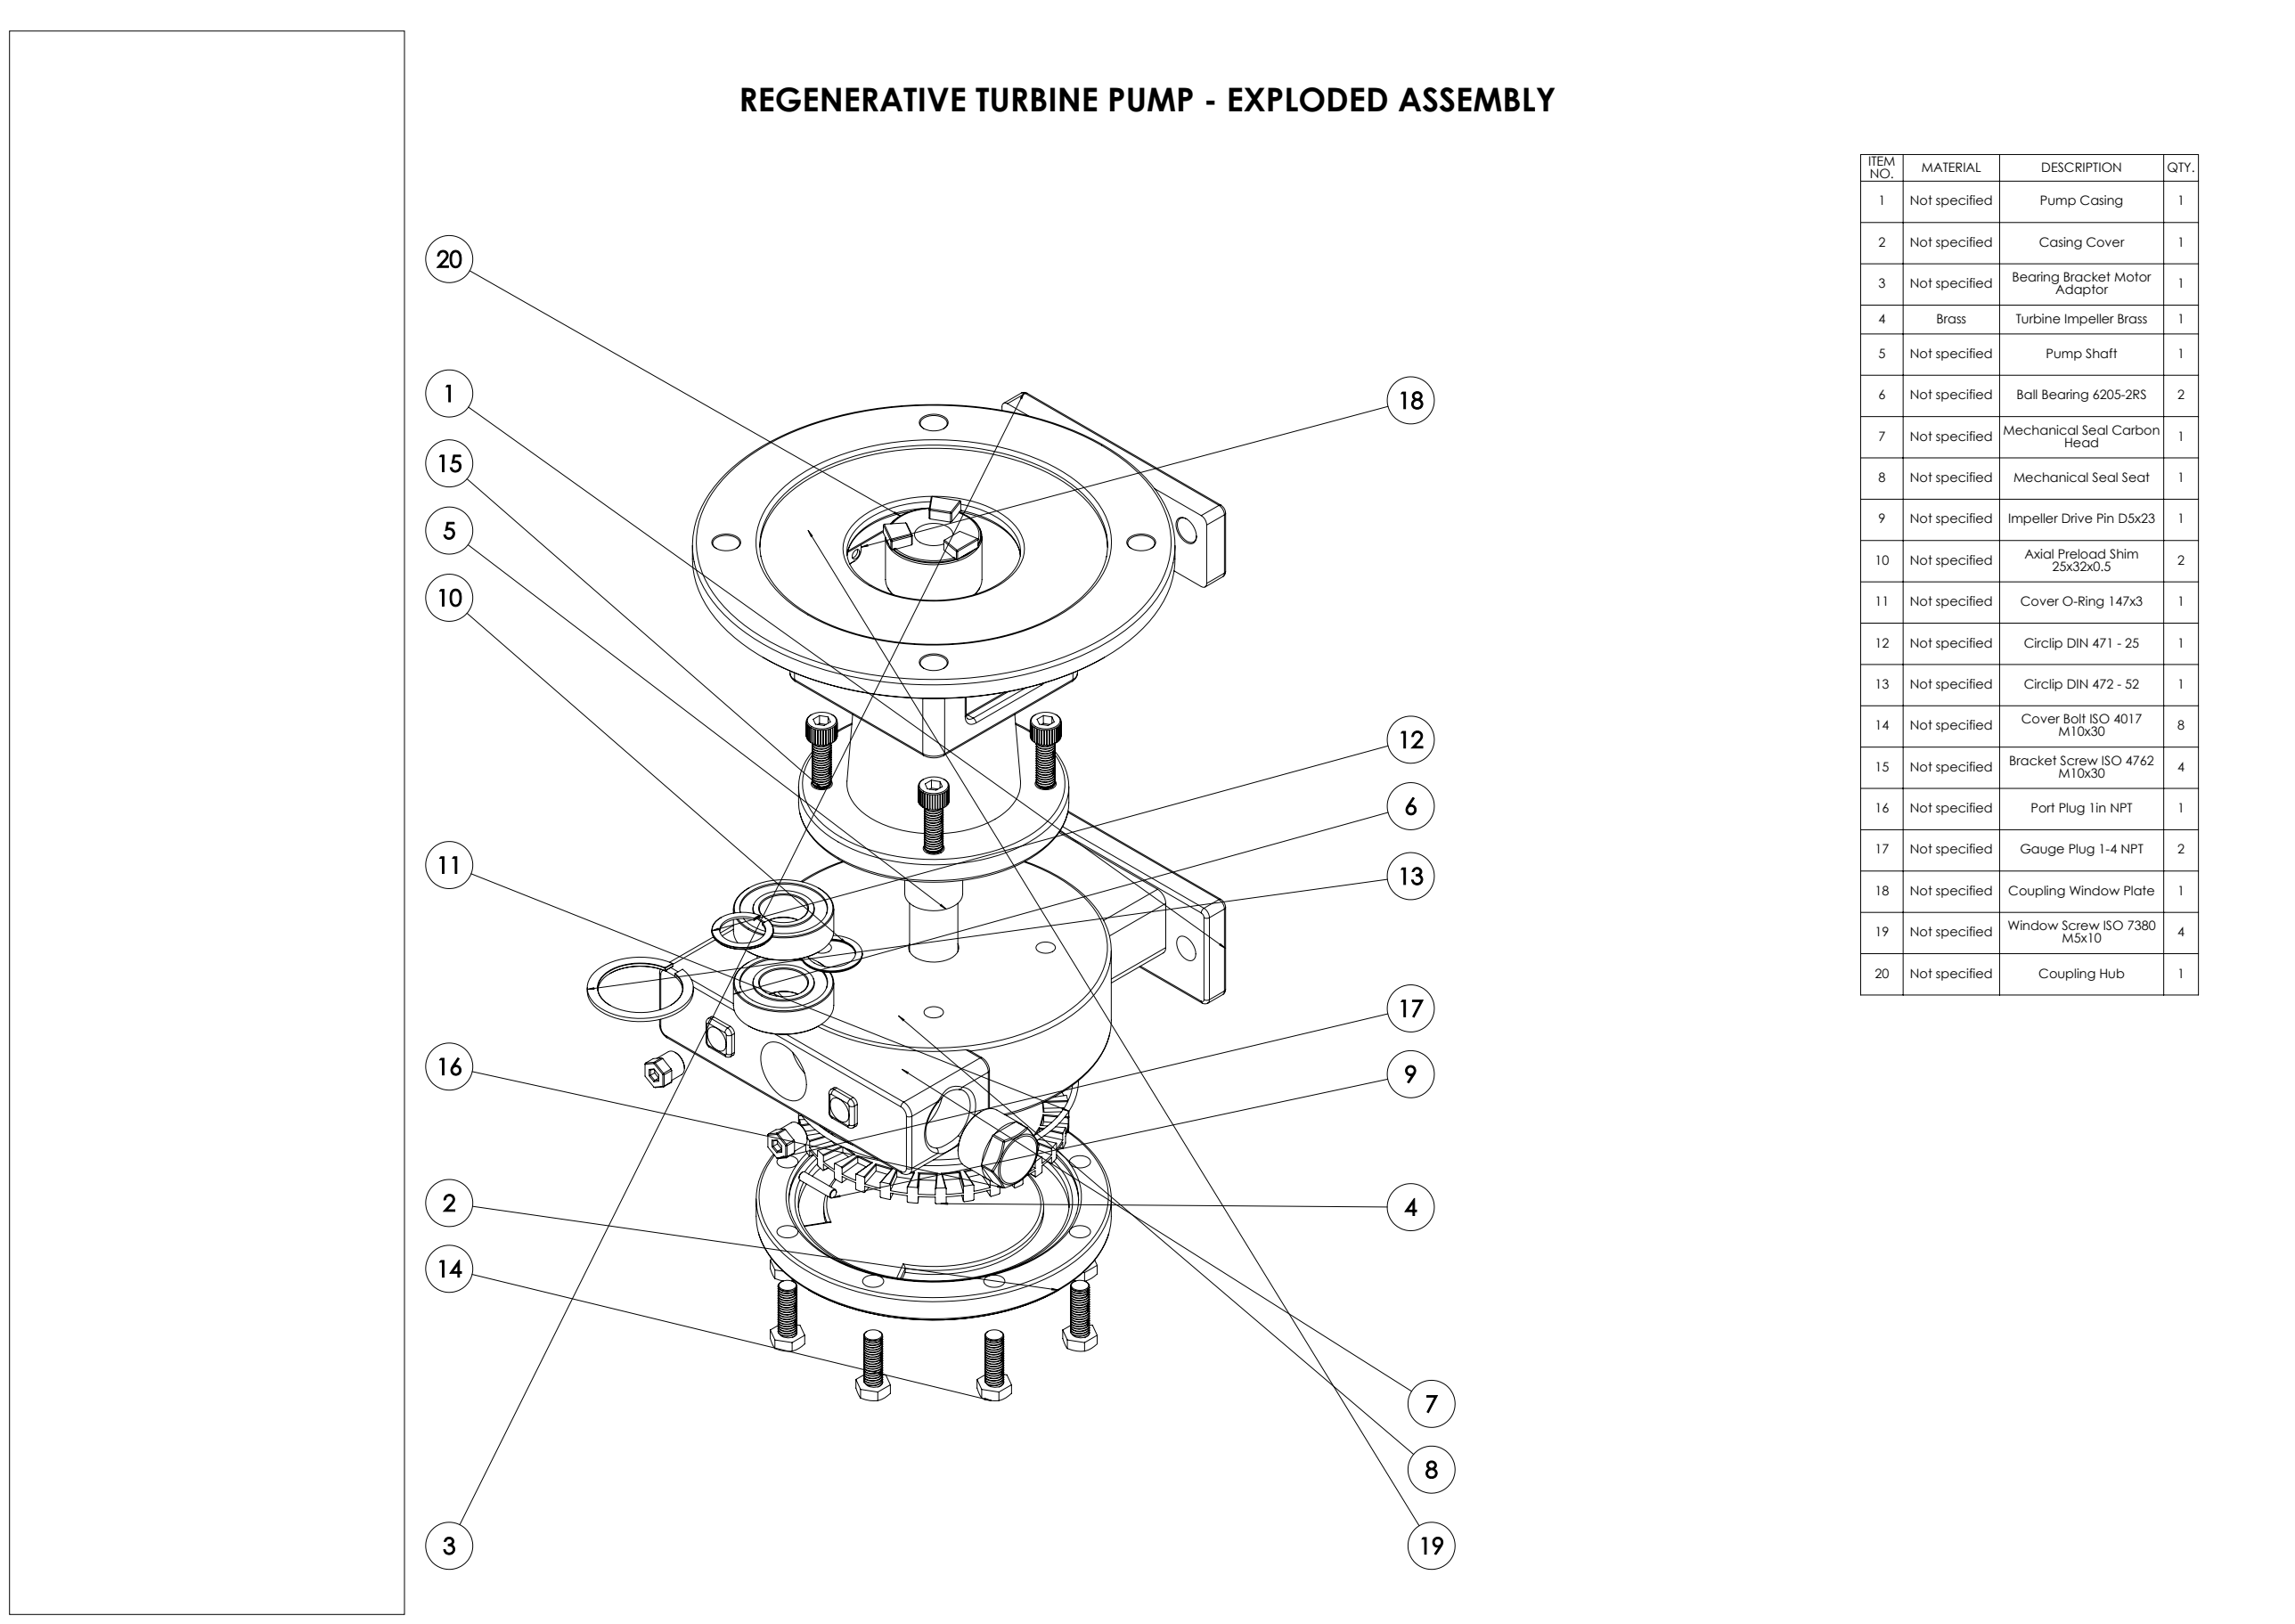
ISO-10303-21;
HEADER;
/* Generated by software containing ST-Developer
 * from STEP Tools, Inc. (www.steptools.com) 
 */

FILE_DESCRIPTION(
/* description */ (''),
/* implementation_level */ '2;1');

FILE_NAME(
/* name */ 'MAS-344',
/* time_stamp */ '2026-10-26T04:15:57-07:00',
/* author */ (''),
/* organization */ (''),
/* preprocessor_version */ 'ST-DEVELOPER v20.2',
/* originating_system */ 'Autodesk Translation Framework v15.15.0.0',
/* authorisation */ '');

FILE_SCHEMA (('AUTOMOTIVE_DESIGN { 1 0 10303 214 3 1 1 }'));
ENDSEC;

DATA;
#10=MECHANICAL_DESIGN_GEOMETRIC_PRESENTATION_REPRESENTATION('',(#452,#453,
#454,#455,#456,#457,#458,#459,#460,#461,#462,#463,#464,#465,#466,#467,#468,
#469,#470,#471),#55737);
#11=ITEM_DEFINED_TRANSFORMATION($,$,#27463,#29940);
#12=ITEM_DEFINED_TRANSFORMATION($,$,#27785,#29941);
#13=ITEM_DEFINED_TRANSFORMATION($,$,#27989,#29942);
#14=ITEM_DEFINED_TRANSFORMATION($,$,#28371,#29943);
#15=ITEM_DEFINED_TRANSFORMATION($,$,#29069,#29944);
#16=ITEM_DEFINED_TRANSFORMATION($,$,#29111,#29945);
#17=ITEM_DEFINED_TRANSFORMATION($,$,#29111,#29946);
#18=ITEM_DEFINED_TRANSFORMATION($,$,#29144,#29947);
#19=ITEM_DEFINED_TRANSFORMATION($,$,#29166,#29948);
#20=ITEM_DEFINED_TRANSFORMATION($,$,#29177,#29949);
#21=ITEM_DEFINED_TRANSFORMATION($,$,#29187,#29950);
#22=ITEM_DEFINED_TRANSFORMATION($,$,#29187,#29951);
#23=ITEM_DEFINED_TRANSFORMATION($,$,#29196,#29952);
#24=ITEM_DEFINED_TRANSFORMATION($,$,#29200,#29953);
#25=ITEM_DEFINED_TRANSFORMATION($,$,#29223,#29954);
#26=ITEM_DEFINED_TRANSFORMATION($,$,#29252,#29955);
#27=ITEM_DEFINED_TRANSFORMATION($,$,#29306,#29956);
#28=ITEM_DEFINED_TRANSFORMATION($,$,#29390,#29957);
#29=ITEM_DEFINED_TRANSFORMATION($,$,#29496,#29958);
#30=ITEM_DEFINED_TRANSFORMATION($,$,#29496,#29959);
#31=ITEM_DEFINED_TRANSFORMATION($,$,#29496,#29960);
#32=ITEM_DEFINED_TRANSFORMATION($,$,#29496,#29961);
#33=ITEM_DEFINED_TRANSFORMATION($,$,#29496,#29962);
#34=ITEM_DEFINED_TRANSFORMATION($,$,#29496,#29963);
#35=ITEM_DEFINED_TRANSFORMATION($,$,#29496,#29964);
#36=ITEM_DEFINED_TRANSFORMATION($,$,#29496,#29965);
#37=ITEM_DEFINED_TRANSFORMATION($,$,#29560,#29966);
#38=ITEM_DEFINED_TRANSFORMATION($,$,#29560,#29967);
#39=ITEM_DEFINED_TRANSFORMATION($,$,#29560,#29968);
#40=ITEM_DEFINED_TRANSFORMATION($,$,#29560,#29969);
#41=ITEM_DEFINED_TRANSFORMATION($,$,#29846,#29970);
#42=ITEM_DEFINED_TRANSFORMATION($,$,#29846,#29971);
#43=ITEM_DEFINED_TRANSFORMATION($,$,#29892,#29972);
#44=ITEM_DEFINED_TRANSFORMATION($,$,#29892,#29973);
#45=ITEM_DEFINED_TRANSFORMATION($,$,#29892,#29974);
#46=ITEM_DEFINED_TRANSFORMATION($,$,#29892,#29975);
#47=(
REPRESENTATION_RELATIONSHIP($,$,#55821,#55820)
REPRESENTATION_RELATIONSHIP_WITH_TRANSFORMATION(#11)
SHAPE_REPRESENTATION_RELATIONSHIP()
);
#48=(
REPRESENTATION_RELATIONSHIP($,$,#55822,#55820)
REPRESENTATION_RELATIONSHIP_WITH_TRANSFORMATION(#12)
SHAPE_REPRESENTATION_RELATIONSHIP()
);
#49=(
REPRESENTATION_RELATIONSHIP($,$,#55823,#55820)
REPRESENTATION_RELATIONSHIP_WITH_TRANSFORMATION(#13)
SHAPE_REPRESENTATION_RELATIONSHIP()
);
#50=(
REPRESENTATION_RELATIONSHIP($,$,#55824,#55820)
REPRESENTATION_RELATIONSHIP_WITH_TRANSFORMATION(#14)
SHAPE_REPRESENTATION_RELATIONSHIP()
);
#51=(
REPRESENTATION_RELATIONSHIP($,$,#55825,#55820)
REPRESENTATION_RELATIONSHIP_WITH_TRANSFORMATION(#15)
SHAPE_REPRESENTATION_RELATIONSHIP()
);
#52=(
REPRESENTATION_RELATIONSHIP($,$,#55826,#55820)
REPRESENTATION_RELATIONSHIP_WITH_TRANSFORMATION(#16)
SHAPE_REPRESENTATION_RELATIONSHIP()
);
#53=(
REPRESENTATION_RELATIONSHIP($,$,#55826,#55820)
REPRESENTATION_RELATIONSHIP_WITH_TRANSFORMATION(#17)
SHAPE_REPRESENTATION_RELATIONSHIP()
);
#54=(
REPRESENTATION_RELATIONSHIP($,$,#55827,#55820)
REPRESENTATION_RELATIONSHIP_WITH_TRANSFORMATION(#18)
SHAPE_REPRESENTATION_RELATIONSHIP()
);
#55=(
REPRESENTATION_RELATIONSHIP($,$,#55828,#55820)
REPRESENTATION_RELATIONSHIP_WITH_TRANSFORMATION(#19)
SHAPE_REPRESENTATION_RELATIONSHIP()
);
#56=(
REPRESENTATION_RELATIONSHIP($,$,#55829,#55820)
REPRESENTATION_RELATIONSHIP_WITH_TRANSFORMATION(#20)
SHAPE_REPRESENTATION_RELATIONSHIP()
);
#57=(
REPRESENTATION_RELATIONSHIP($,$,#55830,#55820)
REPRESENTATION_RELATIONSHIP_WITH_TRANSFORMATION(#21)
SHAPE_REPRESENTATION_RELATIONSHIP()
);
#58=(
REPRESENTATION_RELATIONSHIP($,$,#55830,#55820)
REPRESENTATION_RELATIONSHIP_WITH_TRANSFORMATION(#22)
SHAPE_REPRESENTATION_RELATIONSHIP()
);
#59=(
REPRESENTATION_RELATIONSHIP($,$,#55831,#55820)
REPRESENTATION_RELATIONSHIP_WITH_TRANSFORMATION(#23)
SHAPE_REPRESENTATION_RELATIONSHIP()
);
#60=(
REPRESENTATION_RELATIONSHIP($,$,#55832,#55820)
REPRESENTATION_RELATIONSHIP_WITH_TRANSFORMATION(#24)
SHAPE_REPRESENTATION_RELATIONSHIP()
);
#61=(
REPRESENTATION_RELATIONSHIP($,$,#55833,#55820)
REPRESENTATION_RELATIONSHIP_WITH_TRANSFORMATION(#25)
SHAPE_REPRESENTATION_RELATIONSHIP()
);
#62=(
REPRESENTATION_RELATIONSHIP($,$,#55834,#55820)
REPRESENTATION_RELATIONSHIP_WITH_TRANSFORMATION(#26)
SHAPE_REPRESENTATION_RELATIONSHIP()
);
#63=(
REPRESENTATION_RELATIONSHIP($,$,#55835,#55820)
REPRESENTATION_RELATIONSHIP_WITH_TRANSFORMATION(#27)
SHAPE_REPRESENTATION_RELATIONSHIP()
);
#64=(
REPRESENTATION_RELATIONSHIP($,$,#55836,#55820)
REPRESENTATION_RELATIONSHIP_WITH_TRANSFORMATION(#28)
SHAPE_REPRESENTATION_RELATIONSHIP()
);
#65=(
REPRESENTATION_RELATIONSHIP($,$,#55837,#55820)
REPRESENTATION_RELATIONSHIP_WITH_TRANSFORMATION(#29)
SHAPE_REPRESENTATION_RELATIONSHIP()
);
#66=(
REPRESENTATION_RELATIONSHIP($,$,#55837,#55820)
REPRESENTATION_RELATIONSHIP_WITH_TRANSFORMATION(#30)
SHAPE_REPRESENTATION_RELATIONSHIP()
);
#67=(
REPRESENTATION_RELATIONSHIP($,$,#55837,#55820)
REPRESENTATION_RELATIONSHIP_WITH_TRANSFORMATION(#31)
SHAPE_REPRESENTATION_RELATIONSHIP()
);
#68=(
REPRESENTATION_RELATIONSHIP($,$,#55837,#55820)
REPRESENTATION_RELATIONSHIP_WITH_TRANSFORMATION(#32)
SHAPE_REPRESENTATION_RELATIONSHIP()
);
#69=(
REPRESENTATION_RELATIONSHIP($,$,#55837,#55820)
REPRESENTATION_RELATIONSHIP_WITH_TRANSFORMATION(#33)
SHAPE_REPRESENTATION_RELATIONSHIP()
);
#70=(
REPRESENTATION_RELATIONSHIP($,$,#55837,#55820)
REPRESENTATION_RELATIONSHIP_WITH_TRANSFORMATION(#34)
SHAPE_REPRESENTATION_RELATIONSHIP()
);
#71=(
REPRESENTATION_RELATIONSHIP($,$,#55837,#55820)
REPRESENTATION_RELATIONSHIP_WITH_TRANSFORMATION(#35)
SHAPE_REPRESENTATION_RELATIONSHIP()
);
#72=(
REPRESENTATION_RELATIONSHIP($,$,#55837,#55820)
REPRESENTATION_RELATIONSHIP_WITH_TRANSFORMATION(#36)
SHAPE_REPRESENTATION_RELATIONSHIP()
);
#73=(
REPRESENTATION_RELATIONSHIP($,$,#55838,#55820)
REPRESENTATION_RELATIONSHIP_WITH_TRANSFORMATION(#37)
SHAPE_REPRESENTATION_RELATIONSHIP()
);
#74=(
REPRESENTATION_RELATIONSHIP($,$,#55838,#55820)
REPRESENTATION_RELATIONSHIP_WITH_TRANSFORMATION(#38)
SHAPE_REPRESENTATION_RELATIONSHIP()
);
#75=(
REPRESENTATION_RELATIONSHIP($,$,#55838,#55820)
REPRESENTATION_RELATIONSHIP_WITH_TRANSFORMATION(#39)
SHAPE_REPRESENTATION_RELATIONSHIP()
);
#76=(
REPRESENTATION_RELATIONSHIP($,$,#55838,#55820)
REPRESENTATION_RELATIONSHIP_WITH_TRANSFORMATION(#40)
SHAPE_REPRESENTATION_RELATIONSHIP()
);
#77=(
REPRESENTATION_RELATIONSHIP($,$,#55839,#55820)
REPRESENTATION_RELATIONSHIP_WITH_TRANSFORMATION(#41)
SHAPE_REPRESENTATION_RELATIONSHIP()
);
#78=(
REPRESENTATION_RELATIONSHIP($,$,#55839,#55820)
REPRESENTATION_RELATIONSHIP_WITH_TRANSFORMATION(#42)
SHAPE_REPRESENTATION_RELATIONSHIP()
);
#79=(
REPRESENTATION_RELATIONSHIP($,$,#55840,#55820)
REPRESENTATION_RELATIONSHIP_WITH_TRANSFORMATION(#43)
SHAPE_REPRESENTATION_RELATIONSHIP()
);
#80=(
REPRESENTATION_RELATIONSHIP($,$,#55840,#55820)
REPRESENTATION_RELATIONSHIP_WITH_TRANSFORMATION(#44)
SHAPE_REPRESENTATION_RELATIONSHIP()
);
#81=(
REPRESENTATION_RELATIONSHIP($,$,#55840,#55820)
REPRESENTATION_RELATIONSHIP_WITH_TRANSFORMATION(#45)
SHAPE_REPRESENTATION_RELATIONSHIP()
);
#82=(
REPRESENTATION_RELATIONSHIP($,$,#55840,#55820)
REPRESENTATION_RELATIONSHIP_WITH_TRANSFORMATION(#46)
SHAPE_REPRESENTATION_RELATIONSHIP()
);
#83=CONTEXT_DEPENDENT_SHAPE_REPRESENTATION(#47,#55784);
#84=CONTEXT_DEPENDENT_SHAPE_REPRESENTATION(#48,#55785);
#85=CONTEXT_DEPENDENT_SHAPE_REPRESENTATION(#49,#55786);
#86=CONTEXT_DEPENDENT_SHAPE_REPRESENTATION(#50,#55787);
#87=CONTEXT_DEPENDENT_SHAPE_REPRESENTATION(#51,#55788);
#88=CONTEXT_DEPENDENT_SHAPE_REPRESENTATION(#52,#55789);
#89=CONTEXT_DEPENDENT_SHAPE_REPRESENTATION(#53,#55790);
#90=CONTEXT_DEPENDENT_SHAPE_REPRESENTATION(#54,#55791);
#91=CONTEXT_DEPENDENT_SHAPE_REPRESENTATION(#55,#55792);
#92=CONTEXT_DEPENDENT_SHAPE_REPRESENTATION(#56,#55793);
#93=CONTEXT_DEPENDENT_SHAPE_REPRESENTATION(#57,#55794);
#94=CONTEXT_DEPENDENT_SHAPE_REPRESENTATION(#58,#55795);
#95=CONTEXT_DEPENDENT_SHAPE_REPRESENTATION(#59,#55796);
#96=CONTEXT_DEPENDENT_SHAPE_REPRESENTATION(#60,#55797);
#97=CONTEXT_DEPENDENT_SHAPE_REPRESENTATION(#61,#55798);
#98=CONTEXT_DEPENDENT_SHAPE_REPRESENTATION(#62,#55799);
#99=CONTEXT_DEPENDENT_SHAPE_REPRESENTATION(#63,#55800);
#100=CONTEXT_DEPENDENT_SHAPE_REPRESENTATION(#64,#55801);
#101=CONTEXT_DEPENDENT_SHAPE_REPRESENTATION(#65,#55802);
#102=CONTEXT_DEPENDENT_SHAPE_REPRESENTATION(#66,#55803);
#103=CONTEXT_DEPENDENT_SHAPE_REPRESENTATION(#67,#55804);
#104=CONTEXT_DEPENDENT_SHAPE_REPRESENTATION(#68,#55805);
#105=CONTEXT_DEPENDENT_SHAPE_REPRESENTATION(#69,#55806);
#106=CONTEXT_DEPENDENT_SHAPE_REPRESENTATION(#70,#55807);
#107=CONTEXT_DEPENDENT_SHAPE_REPRESENTATION(#71,#55808);
#108=CONTEXT_DEPENDENT_SHAPE_REPRESENTATION(#72,#55809);
#109=CONTEXT_DEPENDENT_SHAPE_REPRESENTATION(#73,#55810);
#110=CONTEXT_DEPENDENT_SHAPE_REPRESENTATION(#74,#55811);
#111=CONTEXT_DEPENDENT_SHAPE_REPRESENTATION(#75,#55812);
#112=CONTEXT_DEPENDENT_SHAPE_REPRESENTATION(#76,#55813);
#113=CONTEXT_DEPENDENT_SHAPE_REPRESENTATION(#77,#55814);
#114=CONTEXT_DEPENDENT_SHAPE_REPRESENTATION(#78,#55815);
#115=CONTEXT_DEPENDENT_SHAPE_REPRESENTATION(#79,#55816);
#116=CONTEXT_DEPENDENT_SHAPE_REPRESENTATION(#80,#55817);
#117=CONTEXT_DEPENDENT_SHAPE_REPRESENTATION(#81,#55818);
#118=CONTEXT_DEPENDENT_SHAPE_REPRESENTATION(#82,#55819);
#119=NEXT_ASSEMBLY_USAGE_OCCURRENCE('01_Pump_Casing:2',
'01_Pump_Casing:2','01_Pump_Casing:2',#55842,#55843,'01_Pump_Casing:2');
#120=NEXT_ASSEMBLY_USAGE_OCCURRENCE('02_Casing_Cover:2',
'02_Casing_Cover:2','02_Casing_Cover:2',#55842,#55844,
'02_Casing_Cover:2');
#121=NEXT_ASSEMBLY_USAGE_OCCURRENCE(
'03_Bearing_Bracket_Motor_Adaptor:2',
'03_Bearing_Bracket_Motor_Adaptor:2',
'03_Bearing_Bracket_Motor_Adaptor:2',#55842,#55845,
'03_Bearing_Bracket_Motor_Adaptor:2');
#122=NEXT_ASSEMBLY_USAGE_OCCURRENCE('04_Turbine_Impeller_Brass:2',
'04_Turbine_Impeller_Brass:2','04_Turbine_Impeller_Brass:2',#55842,#55846,
'04_Turbine_Impeller_Brass:2');
#123=NEXT_ASSEMBLY_USAGE_OCCURRENCE('05_Pump_Shaft:2','05_Pump_Shaft:2',
'05_Pump_Shaft:2',#55842,#55847,'05_Pump_Shaft:2');
#124=NEXT_ASSEMBLY_USAGE_OCCURRENCE('06_Ball_Bearing_6205-2RS:2',
'06_Ball_Bearing_6205-2RS:2','06_Ball_Bearing_6205-2RS:2',#55842,#55848,
'06_Ball_Bearing_6205-2RS:2');
#125=NEXT_ASSEMBLY_USAGE_OCCURRENCE('06_Ball_Bearing_6205-2RS:3',
'06_Ball_Bearing_6205-2RS:3','06_Ball_Bearing_6205-2RS:3',#55842,#55848,
'06_Ball_Bearing_6205-2RS:3');
#126=NEXT_ASSEMBLY_USAGE_OCCURRENCE('07_Mechanical_Seal_Carbon_Head:2',
'07_Mechanical_Seal_Carbon_Head:2','07_Mechanical_Seal_Carbon_Head:2',#55842,
#55849,'07_Mechanical_Seal_Carbon_Head:2');
#127=NEXT_ASSEMBLY_USAGE_OCCURRENCE('08_Mechanical_Seal_Seat:2',
'08_Mechanical_Seal_Seat:2','08_Mechanical_Seal_Seat:2',#55842,#55850,
'08_Mechanical_Seal_Seat:2');
#128=NEXT_ASSEMBLY_USAGE_OCCURRENCE('09_Impeller_Drive_Pin_D5x23:2',
'09_Impeller_Drive_Pin_D5x23:2','09_Impeller_Drive_Pin_D5x23:2',#55842,
#55851,'09_Impeller_Drive_Pin_D5x23:2');
#129=NEXT_ASSEMBLY_USAGE_OCCURRENCE('10_Axial_Preload_Shim_25x32x0.5:2',
'10_Axial_Preload_Shim_25x32x0.5:2','10_Axial_Preload_Shim_25x32x0.5:2',
#55842,#55852,'10_Axial_Preload_Shim_25x32x0.5:2');
#130=NEXT_ASSEMBLY_USAGE_OCCURRENCE('10_Axial_Preload_Shim_25x32x0.5:3',
'10_Axial_Preload_Shim_25x32x0.5:3','10_Axial_Preload_Shim_25x32x0.5:3',
#55842,#55852,'10_Axial_Preload_Shim_25x32x0.5:3');
#131=NEXT_ASSEMBLY_USAGE_OCCURRENCE('11_Cover_O-Ring_147x3:2',
'11_Cover_O-Ring_147x3:2','11_Cover_O-Ring_147x3:2',#55842,#55853,
'11_Cover_O-Ring_147x3:2');
#132=NEXT_ASSEMBLY_USAGE_OCCURRENCE('12_Circlip_DIN_471_-_25:2',
'12_Circlip_DIN_471_-_25:2','12_Circlip_DIN_471_-_25:2',#55842,#55854,
'12_Circlip_DIN_471_-_25:2');
#133=NEXT_ASSEMBLY_USAGE_OCCURRENCE('13_Circlip_DIN_472_-_52:2',
'13_Circlip_DIN_472_-_52:2','13_Circlip_DIN_472_-_52:2',#55842,#55855,
'13_Circlip_DIN_472_-_52:2');
#134=NEXT_ASSEMBLY_USAGE_OCCURRENCE('16_Port_Plug_1in_NPT:2',
'16_Port_Plug_1in_NPT:2','16_Port_Plug_1in_NPT:2',#55842,#55856,
'16_Port_Plug_1in_NPT:2');
#135=NEXT_ASSEMBLY_USAGE_OCCURRENCE('18_Coupling_Window_Plate:2',
'18_Coupling_Window_Plate:2','18_Coupling_Window_Plate:2',#55842,#55857,
'18_Coupling_Window_Plate:2');
#136=NEXT_ASSEMBLY_USAGE_OCCURRENCE('20_Coupling_Hub:2',
'20_Coupling_Hub:2','20_Coupling_Hub:2',#55842,#55858,
'20_Coupling_Hub:2');
#137=NEXT_ASSEMBLY_USAGE_OCCURRENCE('14_Cover_Bolt_ISO_4017_M10x30:2',
'14_Cover_Bolt_ISO_4017_M10x30:2','14_Cover_Bolt_ISO_4017_M10x30:2',#55842,
#55859,'14_Cover_Bolt_ISO_4017_M10x30:2');
#138=NEXT_ASSEMBLY_USAGE_OCCURRENCE('14_Cover_Bolt_ISO_4017_M10x30:3',
'14_Cover_Bolt_ISO_4017_M10x30:3','14_Cover_Bolt_ISO_4017_M10x30:3',#55842,
#55859,'14_Cover_Bolt_ISO_4017_M10x30:3');
#139=NEXT_ASSEMBLY_USAGE_OCCURRENCE('14_Cover_Bolt_ISO_4017_M10x30:4',
'14_Cover_Bolt_ISO_4017_M10x30:4','14_Cover_Bolt_ISO_4017_M10x30:4',#55842,
#55859,'14_Cover_Bolt_ISO_4017_M10x30:4');
#140=NEXT_ASSEMBLY_USAGE_OCCURRENCE('14_Cover_Bolt_ISO_4017_M10x30:5',
'14_Cover_Bolt_ISO_4017_M10x30:5','14_Cover_Bolt_ISO_4017_M10x30:5',#55842,
#55859,'14_Cover_Bolt_ISO_4017_M10x30:5');
#141=NEXT_ASSEMBLY_USAGE_OCCURRENCE('14_Cover_Bolt_ISO_4017_M10x30:6',
'14_Cover_Bolt_ISO_4017_M10x30:6','14_Cover_Bolt_ISO_4017_M10x30:6',#55842,
#55859,'14_Cover_Bolt_ISO_4017_M10x30:6');
#142=NEXT_ASSEMBLY_USAGE_OCCURRENCE('14_Cover_Bolt_ISO_4017_M10x30:7',
'14_Cover_Bolt_ISO_4017_M10x30:7','14_Cover_Bolt_ISO_4017_M10x30:7',#55842,
#55859,'14_Cover_Bolt_ISO_4017_M10x30:7');
#143=NEXT_ASSEMBLY_USAGE_OCCURRENCE('14_Cover_Bolt_ISO_4017_M10x30:8',
'14_Cover_Bolt_ISO_4017_M10x30:8','14_Cover_Bolt_ISO_4017_M10x30:8',#55842,
#55859,'14_Cover_Bolt_ISO_4017_M10x30:8');
#144=NEXT_ASSEMBLY_USAGE_OCCURRENCE('14_Cover_Bolt_ISO_4017_M10x30:9',
'14_Cover_Bolt_ISO_4017_M10x30:9','14_Cover_Bolt_ISO_4017_M10x30:9',#55842,
#55859,'14_Cover_Bolt_ISO_4017_M10x30:9');
#145=NEXT_ASSEMBLY_USAGE_OCCURRENCE(
'15_Bracket_Screw_ISO_4762_M10x30:2',
'15_Bracket_Screw_ISO_4762_M10x30:2',
'15_Bracket_Screw_ISO_4762_M10x30:2',#55842,#55860,
'15_Bracket_Screw_ISO_4762_M10x30:2');
#146=NEXT_ASSEMBLY_USAGE_OCCURRENCE(
'15_Bracket_Screw_ISO_4762_M10x30:3',
'15_Bracket_Screw_ISO_4762_M10x30:3',
'15_Bracket_Screw_ISO_4762_M10x30:3',#55842,#55860,
'15_Bracket_Screw_ISO_4762_M10x30:3');
#147=NEXT_ASSEMBLY_USAGE_OCCURRENCE(
'15_Bracket_Screw_ISO_4762_M10x30:4',
'15_Bracket_Screw_ISO_4762_M10x30:4',
'15_Bracket_Screw_ISO_4762_M10x30:4',#55842,#55860,
'15_Bracket_Screw_ISO_4762_M10x30:4');
#148=NEXT_ASSEMBLY_USAGE_OCCURRENCE(
'15_Bracket_Screw_ISO_4762_M10x30:5',
'15_Bracket_Screw_ISO_4762_M10x30:5',
'15_Bracket_Screw_ISO_4762_M10x30:5',#55842,#55860,
'15_Bracket_Screw_ISO_4762_M10x30:5');
#149=NEXT_ASSEMBLY_USAGE_OCCURRENCE('17_Gauge_Plug_1-4_NPT:2',
'17_Gauge_Plug_1-4_NPT:2','17_Gauge_Plug_1-4_NPT:2',#55842,#55861,
'17_Gauge_Plug_1-4_NPT:2');
#150=NEXT_ASSEMBLY_USAGE_OCCURRENCE('17_Gauge_Plug_1-4_NPT:3',
'17_Gauge_Plug_1-4_NPT:3','17_Gauge_Plug_1-4_NPT:3',#55842,#55861,
'17_Gauge_Plug_1-4_NPT:3');
#151=NEXT_ASSEMBLY_USAGE_OCCURRENCE('19_Window_Screw_ISO_7380_M5x10:2',
'19_Window_Screw_ISO_7380_M5x10:2','19_Window_Screw_ISO_7380_M5x10:2',#55842,
#55862,'19_Window_Screw_ISO_7380_M5x10:2');
#152=NEXT_ASSEMBLY_USAGE_OCCURRENCE('19_Window_Screw_ISO_7380_M5x10:3',
'19_Window_Screw_ISO_7380_M5x10:3','19_Window_Screw_ISO_7380_M5x10:3',#55842,
#55862,'19_Window_Screw_ISO_7380_M5x10:3');
#153=NEXT_ASSEMBLY_USAGE_OCCURRENCE('19_Window_Screw_ISO_7380_M5x10:4',
'19_Window_Screw_ISO_7380_M5x10:4','19_Window_Screw_ISO_7380_M5x10:4',#55842,
#55862,'19_Window_Screw_ISO_7380_M5x10:4');
#154=NEXT_ASSEMBLY_USAGE_OCCURRENCE('19_Window_Screw_ISO_7380_M5x10:5',
'19_Window_Screw_ISO_7380_M5x10:5','19_Window_Screw_ISO_7380_M5x10:5',#55842,
#55862,'19_Window_Screw_ISO_7380_M5x10:5');
#155=(
BOUNDED_CURVE()
B_SPLINE_CURVE(2,(#41789,#41790,#41791),.UNSPECIFIED.,.F.,.F.)
B_SPLINE_CURVE_WITH_KNOTS((3,3),(0.,1.18679419303782),.UNSPECIFIED.)
CURVE()
GEOMETRIC_REPRESENTATION_ITEM()
RATIONAL_B_SPLINE_CURVE((1.,1.03980835236638,1.06956749269866))
REPRESENTATION_ITEM('')
);
#156=(
BOUNDED_CURVE()
B_SPLINE_CURVE(2,(#41805,#41806,#41807),.UNSPECIFIED.,.F.,.F.)
B_SPLINE_CURVE_WITH_KNOTS((3,3),(8.21579802265979,9.40259221569659),
 .UNSPECIFIED.)
CURVE()
GEOMETRIC_REPRESENTATION_ITEM()
RATIONAL_B_SPLINE_CURVE((1.06956749269861,1.03980835236634,1.))
REPRESENTATION_ITEM('')
);
#157=(
BOUNDED_CURVE()
B_SPLINE_CURVE(2,(#41985,#41986,#41987),.UNSPECIFIED.,.F.,.F.)
B_SPLINE_CURVE_WITH_KNOTS((3,3),(0.,0.694054630120424),.UNSPECIFIED.)
CURVE()
GEOMETRIC_REPRESENTATION_ITEM()
RATIONAL_B_SPLINE_CURVE((1.,1.02328050763935,1.04312410261717))
REPRESENTATION_ITEM('')
);
#158=(
BOUNDED_CURVE()
B_SPLINE_CURVE(2,(#42011,#42012,#42013),.UNSPECIFIED.,.F.,.F.)
B_SPLINE_CURVE_WITH_KNOTS((3,3),(8.21579802265979,9.40259221569658),
 .UNSPECIFIED.)
CURVE()
GEOMETRIC_REPRESENTATION_ITEM()
RATIONAL_B_SPLINE_CURVE((1.06956749269861,1.03980835236634,1.))
REPRESENTATION_ITEM('')
);
#159=(
BOUNDED_CURVE()
B_SPLINE_CURVE(2,(#42017,#42018,#42019),.UNSPECIFIED.,.F.,.F.)
B_SPLINE_CURVE_WITH_KNOTS((3,3),(0.,1.18679419303782),.UNSPECIFIED.)
CURVE()
GEOMETRIC_REPRESENTATION_ITEM()
RATIONAL_B_SPLINE_CURVE((1.,1.03980835236638,1.06956749269866))
REPRESENTATION_ITEM('')
);
#160=(
BOUNDED_CURVE()
B_SPLINE_CURVE(2,(#42032,#42033,#42034),.UNSPECIFIED.,.F.,.F.)
B_SPLINE_CURVE_WITH_KNOTS((3,3),(8.21579802265979,9.40259221569659),
 .UNSPECIFIED.)
CURVE()
GEOMETRIC_REPRESENTATION_ITEM()
RATIONAL_B_SPLINE_CURVE((1.06956749269861,1.03980835236634,1.))
REPRESENTATION_ITEM('')
);
#161=(
BOUNDED_CURVE()
B_SPLINE_CURVE(2,(#42038,#42039,#42040),.UNSPECIFIED.,.F.,.F.)
B_SPLINE_CURVE_WITH_KNOTS((3,3),(0.,1.18679419303782),.UNSPECIFIED.)
CURVE()
GEOMETRIC_REPRESENTATION_ITEM()
RATIONAL_B_SPLINE_CURVE((1.,1.03980835236638,1.06956749269866))
REPRESENTATION_ITEM('')
);
#162=(
BOUNDED_CURVE()
B_SPLINE_CURVE(2,(#42053,#42054,#42055),.UNSPECIFIED.,.F.,.F.)
B_SPLINE_CURVE_WITH_KNOTS((3,3),(8.70853758557616,9.40259221569658),
 .UNSPECIFIED.)
CURVE()
GEOMETRIC_REPRESENTATION_ITEM()
RATIONAL_B_SPLINE_CURVE((1.04312410261717,1.02328050763935,1.))
REPRESENTATION_ITEM('')
);
#163=(
BOUNDED_CURVE()
B_SPLINE_CURVE(2,(#45353,#45354,#45355),.UNSPECIFIED.,.F.,.F.)
B_SPLINE_CURVE_WITH_KNOTS((3,3),(0.25768579992867,0.284744725788376),
 .UNSPECIFIED.)
CURVE()
GEOMETRIC_REPRESENTATION_ITEM()
RATIONAL_B_SPLINE_CURVE((1.00026246290895,1.0001450117334,1.))
REPRESENTATION_ITEM('')
);
#164=(
BOUNDED_CURVE()
B_SPLINE_CURVE(2,(#45362,#45363,#45364),.UNSPECIFIED.,.F.,.F.)
B_SPLINE_CURVE_WITH_KNOTS((3,3),(0.,0.0284560379907694),.UNSPECIFIED.)
CURVE()
GEOMETRIC_REPRESENTATION_ITEM()
RATIONAL_B_SPLINE_CURVE((1.,1.00001378568341,1.))
REPRESENTATION_ITEM('')
);
#165=(
BOUNDED_CURVE()
B_SPLINE_CURVE(2,(#45374,#45375,#45376),.UNSPECIFIED.,.F.,.F.)
B_SPLINE_CURVE_WITH_KNOTS((3,3),(0.,0.0270589258586405),.UNSPECIFIED.)
CURVE()
GEOMETRIC_REPRESENTATION_ITEM()
RATIONAL_B_SPLINE_CURVE((1.,1.00014501173361,1.00026246290934))
REPRESENTATION_ITEM('')
);
#166=(
BOUNDED_CURVE()
B_SPLINE_CURVE(2,(#45385,#45386,#45387),.UNSPECIFIED.,.F.,.F.)
B_SPLINE_CURVE_WITH_KNOTS((3,3),(0.,0.0284560379907693),.UNSPECIFIED.)
CURVE()
GEOMETRIC_REPRESENTATION_ITEM()
RATIONAL_B_SPLINE_CURVE((1.,1.00001378474395,1.))
REPRESENTATION_ITEM('')
);
#167=(
BOUNDED_CURVE()
B_SPLINE_CURVE(2,(#46093,#46094,#46095),.UNSPECIFIED.,.F.,.F.)
B_SPLINE_CURVE_WITH_KNOTS((3,3),(0.,0.0933927438985777),.UNSPECIFIED.)
CURVE()
GEOMETRIC_REPRESENTATION_ITEM()
RATIONAL_B_SPLINE_CURVE((1.,1.00016319148553,1.))
REPRESENTATION_ITEM('')
);
#168=(
BOUNDED_CURVE()
B_SPLINE_CURVE(2,(#46101,#46102,#46103),.UNSPECIFIED.,.F.,.F.)
B_SPLINE_CURVE_WITH_KNOTS((3,3),(0.,0.0933927438985944),.UNSPECIFIED.)
CURVE()
GEOMETRIC_REPRESENTATION_ITEM()
RATIONAL_B_SPLINE_CURVE((1.,1.00016318991919,1.))
REPRESENTATION_ITEM('')
);
#169=(
BOUNDED_CURVE()
B_SPLINE_CURVE(2,(#46107,#46108,#46109),.UNSPECIFIED.,.F.,.F.)
B_SPLINE_CURVE_WITH_KNOTS((3,3),(0.0409294620252543,0.0910167227867222),
 .UNSPECIFIED.)
CURVE()
GEOMETRIC_REPRESENTATION_ITEM()
RATIONAL_B_SPLINE_CURVE((1.00010930039025,1.0001537829794,1.0001434531036))
REPRESENTATION_ITEM('')
);
#170=(
BOUNDED_CURVE()
B_SPLINE_CURVE(2,(#46116,#46117,#46118),.UNSPECIFIED.,.F.,.F.)
B_SPLINE_CURVE_WITH_KNOTS((3,3),(0.0721379811442756,0.122225241901496),
 .UNSPECIFIED.)
CURVE()
GEOMETRIC_REPRESENTATION_ITEM()
RATIONAL_B_SPLINE_CURVE((1.00014345310532,1.00015378298122,1.00010930039153))
REPRESENTATION_ITEM('')
);
#171=(
BOUNDED_CURVE()
B_SPLINE_CURVE(2,(#46120,#46121,#46122),.UNSPECIFIED.,.F.,.F.)
B_SPLINE_CURVE_WITH_KNOTS((3,3),(0.137750552840512,0.208869663053062),
 .UNSPECIFIED.)
CURVE()
GEOMETRIC_REPRESENTATION_ITEM()
RATIONAL_B_SPLINE_CURVE((1.00067579562359,1.00074006560275,1.00069056303564))
REPRESENTATION_ITEM('')
);
#172=(
BOUNDED_CURVE()
B_SPLINE_CURVE(2,(#46124,#46125,#46126),.UNSPECIFIED.,.F.,.F.)
B_SPLINE_CURVE_WITH_KNOTS((3,3),(0.190074031647834,0.281492140864205),
 .UNSPECIFIED.)
CURVE()
GEOMETRIC_REPRESENTATION_ITEM()
RATIONAL_B_SPLINE_CURVE((1.,1.,1.))
REPRESENTATION_ITEM('')
);
#173=(
BOUNDED_CURVE()
B_SPLINE_CURVE(2,(#46130,#46131,#46132),.UNSPECIFIED.,.F.,.F.)
B_SPLINE_CURVE_WITH_KNOTS((3,3),(0.232349708196804,0.282582386132944),
 .UNSPECIFIED.)
CURVE()
GEOMETRIC_REPRESENTATION_ITEM()
RATIONAL_B_SPLINE_CURVE((1.00153573820897,1.00157480000264,1.00155897131611))
REPRESENTATION_ITEM('')
);
#174=(
BOUNDED_CURVE()
B_SPLINE_CURVE(2,(#46136,#46137,#46138),.UNSPECIFIED.,.F.,.F.)
B_SPLINE_CURVE_WITH_KNOTS((3,3),(0.0721379811237271,0.122225241884583),
 .UNSPECIFIED.)
CURVE()
GEOMETRIC_REPRESENTATION_ITEM()
RATIONAL_B_SPLINE_CURVE((1.00014345306605,1.00015378293915,1.00010930036165))
REPRESENTATION_ITEM('')
);
#175=(
BOUNDED_CURVE()
B_SPLINE_CURVE(2,(#46140,#46141,#46142),.UNSPECIFIED.,.F.,.F.)
B_SPLINE_CURVE_WITH_KNOTS((3,3),(0.137750552841826,0.208869663054022),
 .UNSPECIFIED.)
CURVE()
GEOMETRIC_REPRESENTATION_ITEM()
RATIONAL_B_SPLINE_CURVE((1.00067579561801,1.00074006559664,1.00069056302993))
REPRESENTATION_ITEM('')
);
#176=(
BOUNDED_CURVE()
B_SPLINE_CURVE(2,(#46144,#46145,#46146),.UNSPECIFIED.,.F.,.F.)
B_SPLINE_CURVE_WITH_KNOTS((3,3),(0.190074031647831,0.281492140864202),
 .UNSPECIFIED.)
CURVE()
GEOMETRIC_REPRESENTATION_ITEM()
RATIONAL_B_SPLINE_CURVE((1.,1.,1.))
REPRESENTATION_ITEM('')
);
#177=(
BOUNDED_CURVE()
B_SPLINE_CURVE(2,(#46150,#46151,#46152),.UNSPECIFIED.,.F.,.F.)
B_SPLINE_CURVE_WITH_KNOTS((3,3),(0.176442821371904,0.267860930592077),
 .UNSPECIFIED.)
CURVE()
GEOMETRIC_REPRESENTATION_ITEM()
RATIONAL_B_SPLINE_CURVE((1.,1.,1.))
REPRESENTATION_ITEM('')
);
#178=(
BOUNDED_CURVE()
B_SPLINE_CURVE(2,(#46154,#46155,#46156),.UNSPECIFIED.,.F.,.F.)
B_SPLINE_CURVE_WITH_KNOTS((3,3),(0.146981648032891,0.218100758246257),
 .UNSPECIFIED.)
CURVE()
GEOMETRIC_REPRESENTATION_ITEM()
RATIONAL_B_SPLINE_CURVE((1.00069056304666,1.00074006561458,1.00067579563438))
REPRESENTATION_ITEM('')
);
#179=(
BOUNDED_CURVE()
B_SPLINE_CURVE(2,(#46158,#46159,#46160),.UNSPECIFIED.,.F.,.F.)
B_SPLINE_CURVE_WITH_KNOTS((3,3),(0.0409294620291145,0.0910167227899698),
 .UNSPECIFIED.)
CURVE()
GEOMETRIC_REPRESENTATION_ITEM()
RATIONAL_B_SPLINE_CURVE((1.00010930036165,1.00015378293915,1.00014345306605))
REPRESENTATION_ITEM('')
);
#180=(
BOUNDED_CURVE()
B_SPLINE_CURVE(2,(#46164,#46165,#46166),.UNSPECIFIED.,.F.,.F.)
B_SPLINE_CURVE_WITH_KNOTS((3,3),(0.0721379811487405,0.122225241904615),
 .UNSPECIFIED.)
CURVE()
GEOMETRIC_REPRESENTATION_ITEM()
RATIONAL_B_SPLINE_CURVE((1.00014345309917,1.00015378297462,1.00010930038684))
REPRESENTATION_ITEM('')
);
#181=(
BOUNDED_CURVE()
B_SPLINE_CURVE(2,(#46168,#46169,#46170),.UNSPECIFIED.,.F.,.F.)
B_SPLINE_CURVE_WITH_KNOTS((3,3),(0.137750552840201,0.208869663052662),
 .UNSPECIFIED.)
CURVE()
GEOMETRIC_REPRESENTATION_ITEM()
RATIONAL_B_SPLINE_CURVE((1.00067579562257,1.00074006560165,1.0006905630346))
REPRESENTATION_ITEM('')
);
#182=(
BOUNDED_CURVE()
B_SPLINE_CURVE(2,(#46172,#46173,#46174),.UNSPECIFIED.,.F.,.F.)
B_SPLINE_CURVE_WITH_KNOTS((3,3),(0.190074031647822,0.281492140864193),
 .UNSPECIFIED.)
CURVE()
GEOMETRIC_REPRESENTATION_ITEM()
RATIONAL_B_SPLINE_CURVE((1.,1.,1.))
REPRESENTATION_ITEM('')
);
#183=(
BOUNDED_CURVE()
B_SPLINE_CURVE(2,(#46178,#46179,#46180),.UNSPECIFIED.,.F.,.F.)
B_SPLINE_CURVE_WITH_KNOTS((3,3),(0.176442821371898,0.267860930592071),
 .UNSPECIFIED.)
CURVE()
GEOMETRIC_REPRESENTATION_ITEM()
RATIONAL_B_SPLINE_CURVE((1.,1.,1.))
REPRESENTATION_ITEM('')
);
#184=(
BOUNDED_CURVE()
B_SPLINE_CURVE(2,(#46181,#46182,#46183),.UNSPECIFIED.,.F.,.F.)
B_SPLINE_CURVE_WITH_KNOTS((3,3),(0.146981648038779,0.218100758251144),
 .UNSPECIFIED.)
CURVE()
GEOMETRIC_REPRESENTATION_ITEM()
RATIONAL_B_SPLINE_CURVE((1.00069056303571,1.00074006560282,1.00067579562364))
REPRESENTATION_ITEM('')
);
#185=(
BOUNDED_CURVE()
B_SPLINE_CURVE(2,(#46203,#46204,#46205),.UNSPECIFIED.,.F.,.F.)
B_SPLINE_CURVE_WITH_KNOTS((3,3),(0.500185502314131,0.592696752727807),
 .UNSPECIFIED.)
CURVE()
GEOMETRIC_REPRESENTATION_ITEM()
RATIONAL_B_SPLINE_CURVE((1.00953952216291,1.0095311894073,1.00919344691327))
REPRESENTATION_ITEM('')
);
#186=(
BOUNDED_CURVE()
B_SPLINE_CURVE(2,(#46208,#46209,#46210),.UNSPECIFIED.,.F.,.F.)
B_SPLINE_CURVE_WITH_KNOTS((3,3),(0.,0.0933927438985674),.UNSPECIFIED.)
CURVE()
GEOMETRIC_REPRESENTATION_ITEM()
RATIONAL_B_SPLINE_CURVE((1.,1.00016319114243,1.))
REPRESENTATION_ITEM('')
);
#187=(
BOUNDED_CURVE()
B_SPLINE_CURVE(2,(#46213,#46214,#46215),.UNSPECIFIED.,.F.,.F.)
B_SPLINE_CURVE_WITH_KNOTS((3,3),(0.,0.093392743898585),.UNSPECIFIED.)
CURVE()
GEOMETRIC_REPRESENTATION_ITEM()
RATIONAL_B_SPLINE_CURVE((1.,1.0001631911814,1.))
REPRESENTATION_ITEM('')
);
#188=(
BOUNDED_CURVE()
B_SPLINE_CURVE(2,(#46217,#46218,#46219),.UNSPECIFIED.,.F.,.F.)
B_SPLINE_CURVE_WITH_KNOTS((3,3),(0.,0.093392743898585),.UNSPECIFIED.)
CURVE()
GEOMETRIC_REPRESENTATION_ITEM()
RATIONAL_B_SPLINE_CURVE((1.,1.00016319331587,1.))
REPRESENTATION_ITEM('')
);
#189=(
BOUNDED_CURVE()
B_SPLINE_CURVE(2,(#49665,#49666,#49667),.UNSPECIFIED.,.F.,.F.)
B_SPLINE_CURVE_WITH_KNOTS((3,3),(0.15318694727023,1.15036825851539),
 .UNSPECIFIED.)
CURVE()
GEOMETRIC_REPRESENTATION_ITEM()
RATIONAL_B_SPLINE_CURVE((1.05801270189225,1.221687836487,1.05801270189225))
REPRESENTATION_ITEM('')
);
#190=(
BOUNDED_CURVE()
B_SPLINE_CURVE(2,(#49669,#49670,#49671),.UNSPECIFIED.,.F.,.F.)
B_SPLINE_CURVE_WITH_KNOTS((3,3),(0.15318694727023,1.15036825851539),
 .UNSPECIFIED.)
CURVE()
GEOMETRIC_REPRESENTATION_ITEM()
RATIONAL_B_SPLINE_CURVE((1.05801270189225,1.221687836487,1.05801270189225))
REPRESENTATION_ITEM('')
);
#191=(
BOUNDED_CURVE()
B_SPLINE_CURVE(2,(#49673,#49674,#49675),.UNSPECIFIED.,.F.,.F.)
B_SPLINE_CURVE_WITH_KNOTS((3,3),(0.15318694727023,1.15036825851539),
 .UNSPECIFIED.)
CURVE()
GEOMETRIC_REPRESENTATION_ITEM()
RATIONAL_B_SPLINE_CURVE((1.05801270189225,1.221687836487,1.05801270189225))
REPRESENTATION_ITEM('')
);
#192=(
BOUNDED_CURVE()
B_SPLINE_CURVE(2,(#49677,#49678,#49679),.UNSPECIFIED.,.F.,.F.)
B_SPLINE_CURVE_WITH_KNOTS((3,3),(0.15318694727023,1.15036825851539),
 .UNSPECIFIED.)
CURVE()
GEOMETRIC_REPRESENTATION_ITEM()
RATIONAL_B_SPLINE_CURVE((1.05801270189225,1.221687836487,1.05801270189225))
REPRESENTATION_ITEM('')
);
#193=(
BOUNDED_CURVE()
B_SPLINE_CURVE(2,(#49681,#49682,#49683),.UNSPECIFIED.,.F.,.F.)
B_SPLINE_CURVE_WITH_KNOTS((3,3),(0.651777602892793,1.15036825851539),
 .UNSPECIFIED.)
CURVE()
GEOMETRIC_REPRESENTATION_ITEM()
RATIONAL_B_SPLINE_CURVE((1.13985026918963,1.13985026918963,1.05801270189225))
REPRESENTATION_ITEM('')
);
#194=(
BOUNDED_CURVE()
B_SPLINE_CURVE(2,(#49688,#49689,#49690),.UNSPECIFIED.,.F.,.F.)
B_SPLINE_CURVE_WITH_KNOTS((3,3),(0.15318694727023,0.651777602892793),
 .UNSPECIFIED.)
CURVE()
GEOMETRIC_REPRESENTATION_ITEM()
RATIONAL_B_SPLINE_CURVE((1.05801270189225,1.13985026918962,1.13985026918963))
REPRESENTATION_ITEM('')
);
#195=(
BOUNDED_CURVE()
B_SPLINE_CURVE(2,(#49691,#49692,#49693),.UNSPECIFIED.,.F.,.F.)
B_SPLINE_CURVE_WITH_KNOTS((3,3),(0.15318694727023,1.15036825851539),
 .UNSPECIFIED.)
CURVE()
GEOMETRIC_REPRESENTATION_ITEM()
RATIONAL_B_SPLINE_CURVE((1.05801270189225,1.221687836487,1.05801270189225))
REPRESENTATION_ITEM('')
);
#196=(
BOUNDED_CURVE()
B_SPLINE_CURVE(2,(#55655,#55656,#55657),.UNSPECIFIED.,.F.,.F.)
B_SPLINE_CURVE_WITH_KNOTS((3,3),(-1.3174441897901,-0.379169323323544),
 .UNSPECIFIED.)
CURVE()
GEOMETRIC_REPRESENTATION_ITEM()
RATIONAL_B_SPLINE_CURVE((0.987233104755384,0.885817457260044,1.))
REPRESENTATION_ITEM('')
);
#197=ELLIPSE('',#27930,1.60681112727484,1.5);
#198=ELLIPSE('',#27931,1.86380959388014,1.5);
#199=ELLIPSE('',#27932,1.60681112727484,1.5);
#200=ELLIPSE('',#27934,1.62076900489975,1.5);
#201=ELLIPSE('',#27935,1.62076900489975,1.5);
#202=ELLIPSE('',#28373,98.9949493661168,70.);
#203=ELLIPSE('',#28377,98.9949493661169,70.);
#204=ELLIPSE('',#28379,98.994949366116,70.);
#205=ELLIPSE('',#28381,98.9949493661166,70.);
#206=ELLIPSE('',#28383,98.9949493661167,70.);
#207=ELLIPSE('',#28386,98.9949493661165,70.);
#208=ELLIPSE('',#28388,98.9949493661168,70.);
#209=ELLIPSE('',#28390,98.9949493661164,70.);
#210=ELLIPSE('',#28392,98.9949493661164,70.);
#211=ELLIPSE('',#28394,98.9949493661161,70.);
#212=ELLIPSE('',#28396,98.9949493661166,70.);
#213=ELLIPSE('',#28398,98.9949493661183,70.);
#214=ELLIPSE('',#28400,98.9949493661177,70.);
#215=ELLIPSE('',#28402,98.9949493661167,70.);
#216=ELLIPSE('',#28404,98.9949493661162,70.);
#217=ELLIPSE('',#28406,98.9949493661183,70.);
#218=ELLIPSE('',#28408,98.9949493661169,70.);
#219=ELLIPSE('',#28410,98.9949493661158,70.);
#220=ELLIPSE('',#28412,98.9949493661173,70.);
#221=ELLIPSE('',#28414,98.9949493661164,70.);
#222=ELLIPSE('',#28416,98.9949493661164,70.);
#223=ELLIPSE('',#28418,98.9949493661165,70.);
#224=ELLIPSE('',#28420,98.9949493661166,70.);
#225=ELLIPSE('',#28422,98.9949493661157,70.);
#226=ELLIPSE('',#28424,98.9949493661165,70.);
#227=ELLIPSE('',#28426,98.9949493661161,70.);
#228=ELLIPSE('',#28428,98.9949493661176,70.);
#229=ELLIPSE('',#28430,98.9949493661175,70.);
#230=ELLIPSE('',#28432,98.9949493661175,70.);
#231=ELLIPSE('',#28434,98.9949493661157,70.);
#232=ELLIPSE('',#28436,98.9949493661157,70.);
#233=ELLIPSE('',#28438,98.9949493661164,70.);
#234=ELLIPSE('',#28440,98.9949493661164,70.);
#235=ELLIPSE('',#28442,98.9949493661168,70.);
#236=ELLIPSE('',#28444,98.9949493661168,70.);
#237=ELLIPSE('',#28446,98.9949493661169,70.);
#238=ELLIPSE('',#28448,98.9949493661168,70.);
#239=ELLIPSE('',#28450,98.9949493661164,70.);
#240=ELLIPSE('',#28452,98.9949493661169,70.);
#241=ELLIPSE('',#28454,98.9949493661162,70.);
#242=ELLIPSE('',#28456,98.9949493661177,70.);
#243=ELLIPSE('',#28458,98.9949493661175,70.);
#244=ELLIPSE('',#28460,98.9949493661171,70.);
#245=ELLIPSE('',#28462,98.9949493661161,70.);
#246=ELLIPSE('',#28464,98.9949493661165,70.);
#247=ELLIPSE('',#28466,98.9949493661153,70.);
#248=ELLIPSE('',#28468,98.9949493661177,70.);
#249=ELLIPSE('',#28470,98.9949493661165,70.);
#250=ELLIPSE('',#28472,98.9949493661174,70.);
#251=ELLIPSE('',#28474,98.9949493661164,70.);
#252=ELLIPSE('',#28476,98.9949493661164,70.);
#253=ELLIPSE('',#28478,98.9949493661163,70.);
#254=ELLIPSE('',#28480,98.9949493661165,70.);
#255=ELLIPSE('',#28482,98.994949366118,70.);
#256=ELLIPSE('',#28484,98.9949493661142,70.);
#257=ELLIPSE('',#28486,98.9949493661172,70.);
#258=ELLIPSE('',#28488,98.9949493661162,70.);
#259=ELLIPSE('',#28490,98.9949493661172,70.);
#260=ELLIPSE('',#28492,98.9949493661145,70.);
#261=ELLIPSE('',#28494,98.9949493661177,70.);
#262=ELLIPSE('',#28496,98.9949493661172,70.);
#263=ELLIPSE('',#28498,98.9949493661164,70.);
#264=ELLIPSE('',#28500,98.9949493661167,70.);
#265=ELLIPSE('',#28502,98.9949493661168,70.);
#266=ELLIPSE('',#28504,98.9949493661167,70.);
#267=ELLIPSE('',#28507,98.9949493661169,70.);
#268=ELLIPSE('',#28509,98.9949493661168,70.);
#269=ELLIPSE('',#28511,98.9949493661169,70.);
#270=ELLIPSE('',#28513,98.9949493661159,70.);
#271=ELLIPSE('',#28515,98.9949493661171,70.);
#272=ELLIPSE('',#28517,98.994949366117,70.);
#273=ELLIPSE('',#28519,98.9949493661175,70.);
#274=ELLIPSE('',#28521,98.9949493661167,70.);
#275=ELLIPSE('',#28523,98.9949493661162,70.);
#276=ELLIPSE('',#28525,98.9949493661158,70.);
#277=ELLIPSE('',#28527,98.9949493661165,70.);
#278=ELLIPSE('',#28529,98.9949493661165,70.);
#279=ELLIPSE('',#28531,98.9949493661172,70.);
#280=ELLIPSE('',#28533,98.9949493661169,70.);
#281=ELLIPSE('',#28535,98.9949493661167,70.);
#282=ELLIPSE('',#28537,98.9949493661167,70.);
#283=ELLIPSE('',#28539,98.9949493661169,70.);
#284=ELLIPSE('',#28541,98.9949493661168,70.);
#285=ELLIPSE('',#28543,98.9949493661168,70.);
#286=ELLIPSE('',#28545,98.9949493661165,70.);
#287=ELLIPSE('',#28547,98.9949493661166,70.);
#288=ELLIPSE('',#28549,98.9949493661168,70.);
#289=ELLIPSE('',#28551,98.9949493661175,70.);
#290=ELLIPSE('',#28553,98.9949493661167,70.);
#291=ELLIPSE('',#28555,98.994949366117,70.);
#292=ELLIPSE('',#28557,98.9949493661167,70.);
#293=ELLIPSE('',#28559,98.9949493661163,70.);
#294=ELLIPSE('',#28561,98.9949493661166,70.);
#295=ELLIPSE('',#28563,98.9949493661168,70.);
#296=ELLIPSE('',#28565,98.9949493661167,70.);
#297=ELLIPSE('',#28567,98.9949493661168,70.);
#298=ELLIPSE('',#28569,98.9949493661169,70.);
#299=ELLIPSE('',#28571,98.9949493661166,70.);
#300=ELLIPSE('',#28573,98.9949493661162,70.);
#301=ELLIPSE('',#28575,98.994949366117,70.);
#302=ELLIPSE('',#28577,98.9949493661165,70.);
#303=ELLIPSE('',#28579,98.9949493661173,70.);
#304=ELLIPSE('',#28581,98.9949493661167,70.);
#305=ELLIPSE('',#28583,98.9949493661156,70.);
#306=ELLIPSE('',#28585,98.9949493661166,70.);
#307=ELLIPSE('',#28587,98.9949493661165,70.);
#308=ELLIPSE('',#28589,98.9949493661157,70.);
#309=ELLIPSE('',#28591,98.9949493661168,70.);
#310=ELLIPSE('',#28593,98.9949493661167,70.);
#311=ELLIPSE('',#28595,98.9949493661167,70.);
#312=ELLIPSE('',#28597,98.9949493661167,70.);
#313=ELLIPSE('',#28599,98.9949493661168,70.);
#314=ELLIPSE('',#28601,98.9949493661165,70.);
#315=ELLIPSE('',#28603,98.9949493661168,70.);
#316=ELLIPSE('',#28605,98.994949366117,70.);
#317=ELLIPSE('',#28607,98.9949493661166,70.);
#318=ELLIPSE('',#28609,98.9949493661156,70.);
#319=ELLIPSE('',#28611,98.9949493661171,70.);
#320=ELLIPSE('',#28613,98.9949493661167,70.);
#321=ELLIPSE('',#28615,98.9949493661169,70.);
#322=ELLIPSE('',#28899,14.1562777593547,10.01);
#323=ELLIPSE('',#28901,14.1562777593547,10.01);
#324=ELLIPSE('',#28906,14.1562777593547,10.01);
#325=ELLIPSE('',#28907,14.1562777593547,10.01);
#326=ELLIPSE('',#28908,14.1562777593547,10.01);
#327=ELLIPSE('',#28912,14.1562777593547,10.01);
#328=ELLIPSE('',#28914,14.1562777593547,10.01);
#329=ELLIPSE('',#28921,14.1562777593547,10.01);
#330=ELLIPSE('',#29202,16.8998520703585,11.95);
#331=ELLIPSE('',#29207,16.8998520703585,11.95);
#332=ELLIPSE('',#29211,16.8998520703585,11.95);
#333=ELLIPSE('',#29213,16.8998520703585,11.95);
#334=ELLIPSE('',#29227,38.8908729652601,27.5);
#335=ELLIPSE('',#29234,38.8908729652601,27.5);
#336=ELLIPSE('',#29237,38.8908729652601,27.5);
#337=ELLIPSE('',#29243,38.8908729652601,27.5);
#338=SPHERICAL_SURFACE('',#27885,1.5);
#339=CONICAL_SURFACE('',#27821,91.5,0.785398163397447);
#340=CONICAL_SURFACE('',#27879,56.,0.785398163397451);
#341=CONICAL_SURFACE('',#27990,26.26,0.785398163397439);
#342=CONICAL_SURFACE('',#28000,26.26,0.785398163397439);
#343=CONICAL_SURFACE('',#28004,7.25,0.785398163397439);
#344=CONICAL_SURFACE('',#28019,7.25,0.785398163397439);
#345=CONICAL_SURFACE('',#28023,2.8,0.785398163397448);
#346=CONICAL_SURFACE('',#28036,2.8,0.785398163397448);
#347=CONICAL_SURFACE('',#28043,2.8,0.785398163397448);
#348=CONICAL_SURFACE('',#28047,2.8,0.785398163397448);
#349=CONICAL_SURFACE('',#28052,2.8,0.785398163397448);
#350=CONICAL_SURFACE('',#28062,2.8,0.785398163397448);
#351=CONICAL_SURFACE('',#28063,2.8,0.785398163397448);
#352=CONICAL_SURFACE('',#28064,2.8,0.785398163397448);
#353=CONICAL_SURFACE('',#28065,7.25,0.785398163397439);
#354=CONICAL_SURFACE('',#28076,7.25,0.785398163397439);
#355=CONICAL_SURFACE('',#28080,7.25000000000001,0.785398163397448);
#356=CONICAL_SURFACE('',#28084,7.25,0.785398163397448);
#357=CONICAL_SURFACE('',#28088,7.25,0.785398163397439);
#358=CONICAL_SURFACE('',#28096,7.25,0.785398163397439);
#359=CONICAL_SURFACE('',#28122,121.5,1.37340076694501);
#360=CONICAL_SURFACE('',#28124,124.5,0.785398163397457);
#361=CONICAL_SURFACE('',#28129,91.5,1.50724565536944);
#362=CONICAL_SURFACE('',#28370,42.5,0.0693331336882086);
#363=CONICAL_SURFACE('',#29080,9.8,0.785398163397448);
#364=CONICAL_SURFACE('',#29084,11.25,1.37340076694502);
#365=CONICAL_SURFACE('',#29108,9.75,0.785398163397442);
#366=CONICAL_SURFACE('',#29112,15.9,0.278299659005112);
#367=CONICAL_SURFACE('',#29117,22.7,0.278299659005112);
#368=CONICAL_SURFACE('',#29121,25.775,0.785398163397448);
#369=CONICAL_SURFACE('',#29125,25.775,0.785398163397448);
#370=CONICAL_SURFACE('',#29129,22.7,0.278299659005112);
#371=CONICAL_SURFACE('',#29133,15.9,0.278299659005112);
#372=CONICAL_SURFACE('',#29137,12.725,0.785398163397448);
#373=CONICAL_SURFACE('',#29141,12.725,0.785398163397448);
#374=CONICAL_SURFACE('',#29145,17.75,0.785398163397448);
#375=CONICAL_SURFACE('',#29158,17.5,0.785398163397449);
#376=CONICAL_SURFACE('',#29172,19.75,0.785398163397451);
#377=CONICAL_SURFACE('',#29180,2.35,0.785398163397447);
#378=CONICAL_SURFACE('',#29184,2.35,0.785398163397447);
#379=CONICAL_SURFACE('',#29203,15.9,0.78539816339744);
#380=CONICAL_SURFACE('',#29214,15.9,0.78539816339744);
#381=CONICAL_SURFACE('',#29230,22.1,0.785398163397444);
#382=CONICAL_SURFACE('',#29238,22.1,0.785398163397444);
#383=CONICAL_SURFACE('',#29253,13.9397047631572,1.30899058790991);
#384=CONICAL_SURFACE('',#29256,16.15,1.04718484902493);
#385=CONICAL_SURFACE('',#29303,16.45,0.785398163397448);
#386=CONICAL_SURFACE('',#29308,4.90000000000002,0.785398163397446);
#387=CONICAL_SURFACE('',#29312,4.90000000000001,0.785398163397446);
#388=CONICAL_SURFACE('',#29316,4.90000000000003,0.785398163397493);
#389=CONICAL_SURFACE('',#29320,4.9,0.785398163397493);
#390=CONICAL_SURFACE('',#29339,4.9,0.785398163397493);
#391=CONICAL_SURFACE('',#29343,4.90000000000003,0.785398163397493);
#392=CONICAL_SURFACE('',#29347,4.90000000000001,0.785398163397446);
#393=CONICAL_SURFACE('',#29350,4.90000000000002,0.785398163397446);
#394=CONICAL_SURFACE('',#29361,3.90000000000002,0.785398163397454);
#395=CONICAL_SURFACE('',#29365,3.90000000000002,0.785398163397446);
#396=CONICAL_SURFACE('',#29369,3.89999999999998,0.785398163397493);
#397=CONICAL_SURFACE('',#29373,3.89999999999997,0.785398163397493);
#398=CONICAL_SURFACE('',#29391,23.9267766952966,1.17809724509616);
#399=CONICAL_SURFACE('',#29395,24.5,0.785398163397442);
#400=CONICAL_SURFACE('',#29403,23.9267766952966,1.17809724509616);
#401=CONICAL_SURFACE('',#29407,24.5,0.785398163397442);
#402=CONICAL_SURFACE('',#29412,23.9267766952966,1.17809724509616);
#403=CONICAL_SURFACE('',#29414,23.9267766952966,1.17809724509616);
#404=CONICAL_SURFACE('',#29437,24.8232233047034,0.392699081698705);
#405=CONICAL_SURFACE('',#29443,24.8232233047034,0.392699081698705);
#406=CONICAL_SURFACE('',#29545,8.83380215351701,1.04669145110647);
#407=CONICAL_SURFACE('',#29558,4.75,0.78539816339745);
#408=CONICAL_SURFACE('',#29836,4.75,0.78539816339745);
#409=CONICAL_SURFACE('',#29843,7.75,0.785398163397448);
#410=CONICAL_SURFACE('',#29889,6.6,0.785398163397447);
#411=CONICAL_SURFACE('',#29935,2.35,0.785398163397447);
#412=SHAPE_REPRESENTATION_RELATIONSHIP('SRR','None',#55821,#432);
#413=SHAPE_REPRESENTATION_RELATIONSHIP('SRR','None',#55822,#433);
#414=SHAPE_REPRESENTATION_RELATIONSHIP('SRR','None',#55823,#434);
#415=SHAPE_REPRESENTATION_RELATIONSHIP('SRR','None',#55824,#435);
#416=SHAPE_REPRESENTATION_RELATIONSHIP('SRR','None',#55825,#436);
#417=SHAPE_REPRESENTATION_RELATIONSHIP('SRR','None',#55826,#437);
#418=SHAPE_REPRESENTATION_RELATIONSHIP('SRR','None',#55827,#438);
#419=SHAPE_REPRESENTATION_RELATIONSHIP('SRR','None',#55828,#439);
#420=SHAPE_REPRESENTATION_RELATIONSHIP('SRR','None',#55829,#440);
#421=SHAPE_REPRESENTATION_RELATIONSHIP('SRR','None',#55830,#441);
#422=SHAPE_REPRESENTATION_RELATIONSHIP('SRR','None',#55831,#442);
#423=SHAPE_REPRESENTATION_RELATIONSHIP('SRR','None',#55832,#443);
#424=SHAPE_REPRESENTATION_RELATIONSHIP('SRR','None',#55833,#444);
#425=SHAPE_REPRESENTATION_RELATIONSHIP('SRR','None',#55834,#445);
#426=SHAPE_REPRESENTATION_RELATIONSHIP('SRR','None',#55835,#446);
#427=SHAPE_REPRESENTATION_RELATIONSHIP('SRR','None',#55836,#447);
#428=SHAPE_REPRESENTATION_RELATIONSHIP('SRR','None',#55837,#448);
#429=SHAPE_REPRESENTATION_RELATIONSHIP('SRR','None',#55838,#449);
#430=SHAPE_REPRESENTATION_RELATIONSHIP('SRR','None',#55839,#450);
#431=SHAPE_REPRESENTATION_RELATIONSHIP('SRR','None',#55840,#451);
#432=ADVANCED_BREP_SHAPE_REPRESENTATION('',(#472),#55717);
#433=ADVANCED_BREP_SHAPE_REPRESENTATION('',(#473),#55718);
#434=ADVANCED_BREP_SHAPE_REPRESENTATION('',(#474),#55719);
#435=ADVANCED_BREP_SHAPE_REPRESENTATION('',(#475),#55720);
#436=ADVANCED_BREP_SHAPE_REPRESENTATION('',(#476),#55721);
#437=ADVANCED_BREP_SHAPE_REPRESENTATION('',(#477),#55722);
#438=ADVANCED_BREP_SHAPE_REPRESENTATION('',(#478),#55723);
#439=ADVANCED_BREP_SHAPE_REPRESENTATION('',(#479),#55724);
#440=ADVANCED_BREP_SHAPE_REPRESENTATION('',(#480),#55725);
#441=ADVANCED_BREP_SHAPE_REPRESENTATION('',(#481),#55726);
#442=ADVANCED_BREP_SHAPE_REPRESENTATION('',(#482),#55727);
#443=ADVANCED_BREP_SHAPE_REPRESENTATION('',(#483),#55728);
#444=ADVANCED_BREP_SHAPE_REPRESENTATION('',(#484),#55729);
#445=ADVANCED_BREP_SHAPE_REPRESENTATION('',(#485),#55730);
#446=ADVANCED_BREP_SHAPE_REPRESENTATION('',(#486),#55731);
#447=ADVANCED_BREP_SHAPE_REPRESENTATION('',(#487),#55732);
#448=ADVANCED_BREP_SHAPE_REPRESENTATION('',(#488),#55733);
#449=ADVANCED_BREP_SHAPE_REPRESENTATION('',(#489),#55734);
#450=ADVANCED_BREP_SHAPE_REPRESENTATION('',(#490),#55735);
#451=ADVANCED_BREP_SHAPE_REPRESENTATION('',(#491),#55736);
#452=STYLED_ITEM('',(#56005),#472);
#453=STYLED_ITEM('',(#55977),#473);
#454=STYLED_ITEM('',(#55991),#474);
#455=STYLED_ITEM('',(#55984),#475);
#456=STYLED_ITEM('',(#55991),#476);
#457=STYLED_ITEM('',(#55991),#477);
#458=STYLED_ITEM('',(#55998),#478);
#459=STYLED_ITEM('',(#55998),#479);
#460=STYLED_ITEM('',(#55991),#480);
#461=STYLED_ITEM('',(#56005),#481);
#462=STYLED_ITEM('',(#55998),#482);
#463=STYLED_ITEM('',(#55991),#483);
#464=STYLED_ITEM('',(#55991),#484);
#465=STYLED_ITEM('',(#55977),#485);
#466=STYLED_ITEM('',(#55977),#486);
#467=STYLED_ITEM('',(#55984),#487);
#468=STYLED_ITEM('',(#55998),#488);
#469=STYLED_ITEM('',(#55998),#489);
#470=STYLED_ITEM('',(#55984),#490);
#471=STYLED_ITEM('',(#55998),#491);
#472=MANIFOLD_SOLID_BREP('Body1',#27221);
#473=MANIFOLD_SOLID_BREP('Body1',#27222);
#474=MANIFOLD_SOLID_BREP('Body1',#27223);
#475=MANIFOLD_SOLID_BREP('Body1',#27224);
#476=MANIFOLD_SOLID_BREP('Body1',#27225);
#477=MANIFOLD_SOLID_BREP('Body1',#27226);
#478=MANIFOLD_SOLID_BREP('Body1',#27227);
#479=MANIFOLD_SOLID_BREP('Body1',#27228);
#480=MANIFOLD_SOLID_BREP('Body1',#27229);
#481=MANIFOLD_SOLID_BREP('Body1',#27230);
#482=MANIFOLD_SOLID_BREP('Body1',#27231);
#483=MANIFOLD_SOLID_BREP('Body1',#27232);
#484=MANIFOLD_SOLID_BREP('Body1',#27233);
#485=MANIFOLD_SOLID_BREP('Body1',#27234);
#486=MANIFOLD_SOLID_BREP('Body1',#27235);
#487=MANIFOLD_SOLID_BREP('Body1',#27236);
#488=MANIFOLD_SOLID_BREP('Body1',#27237);
#489=MANIFOLD_SOLID_BREP('Body1',#27238);
#490=MANIFOLD_SOLID_BREP('Body1',#27239);
#491=MANIFOLD_SOLID_BREP('Body1',#27240);
#492=B_SPLINE_SURFACE_WITH_KNOTS('',3,3,((#38041,#38042,#38043,#38044,#38045,
#38046,#38047,#38048),(#38049,#38050,#38051,#38052,#38053,#38054,#38055,
#38056),(#38057,#38058,#38059,#38060,#38061,#38062,#38063,#38064),(#38065,
#38066,#38067,#38068,#38069,#38070,#38071,#38072),(#38073,#38074,#38075,
#38076,#38077,#38078,#38079,#38080),(#38081,#38082,#38083,#38084,#38085,
#38086,#38087,#38088)),.UNSPECIFIED.,.F.,.F.,.F.,(4,1,1,4),(4,1,1,1,1,4),
(0.,0.285714285714286,0.571428571428571,1.),(0.,0.532095912060411,0.798143868090616,
1.06419182412082,1.59628773618123,1.86233569221144),.UNSPECIFIED.);
#493=B_SPLINE_SURFACE_WITH_KNOTS('',3,3,((#38114,#38115,#38116,#38117,#38118,
#38119,#38120,#38121),(#38122,#38123,#38124,#38125,#38126,#38127,#38128,
#38129),(#38130,#38131,#38132,#38133,#38134,#38135,#38136,#38137),(#38138,
#38139,#38140,#38141,#38142,#38143,#38144,#38145),(#38146,#38147,#38148,
#38149,#38150,#38151,#38152,#38153),(#38154,#38155,#38156,#38157,#38158,
#38159,#38160,#38161)),.UNSPECIFIED.,.F.,.F.,.F.,(4,1,1,4),(4,1,1,1,1,4),
(0.,0.285714285714286,0.571428571428571,1.),(8.87358627225765E-17,0.532095912059373,
0.798143868089059,1.06419182411875,1.33023978014843,1.8623356922078),
 .UNSPECIFIED.);
#494=B_SPLINE_SURFACE_WITH_KNOTS('',3,3,((#38313,#38314,#38315,#38316,#38317,
#38318,#38319,#38320,#38321),(#38322,#38323,#38324,#38325,#38326,#38327,
#38328,#38329,#38330),(#38331,#38332,#38333,#38334,#38335,#38336,#38337,
#38338,#38339),(#38340,#38341,#38342,#38343,#38344,#38345,#38346,#38347,
#38348),(#38349,#38350,#38351,#38352,#38353,#38354,#38355,#38356,#38357),
(#38358,#38359,#38360,#38361,#38362,#38363,#38364,#38365,#38366)),
 .UNSPECIFIED.,.F.,.F.,.F.,(4,1,1,4),(4,1,1,1,1,1,4),(0.,0.285714285714286,
0.571428571428571,1.),(0.,0.266047956030205,0.798143868090615,1.06419182412082,
1.33023978015103,1.46326375816613,1.86233569221144),.UNSPECIFIED.);
#495=B_SPLINE_SURFACE_WITH_KNOTS('',3,3,((#38384,#38385,#38386,#38387,#38388,
#38389,#38390,#38391),(#38392,#38393,#38394,#38395,#38396,#38397,#38398,
#38399),(#38400,#38401,#38402,#38403,#38404,#38405,#38406,#38407),(#38408,
#38409,#38410,#38411,#38412,#38413,#38414,#38415),(#38416,#38417,#38418,
#38419,#38420,#38421,#38422,#38423),(#38424,#38425,#38426,#38427,#38428,
#38429,#38430,#38431)),.UNSPECIFIED.,.F.,.F.,.F.,(4,1,1,4),(4,1,1,1,1,4),
(0.,0.285714285714286,0.571428571428571,1.),(2.59005157847017E-16,0.532095912059373,
0.79814386808906,1.06419182411875,1.59628773617812,1.86233569220781),
 .UNSPECIFIED.);
#496=B_SPLINE_SURFACE_WITH_KNOTS('',3,3,((#38586,#38587,#38588,#38589,#38590,
#38591),(#38592,#38593,#38594,#38595,#38596,#38597),(#38598,#38599,#38600,
#38601,#38602,#38603),(#38604,#38605,#38606,#38607,#38608,#38609)),
 .UNSPECIFIED.,.F.,.F.,.F.,(4,4),(4,1,1,4),(0.,1.),(0.,0.571428571428571,
0.857142857142857,1.),.UNSPECIFIED.);
#497=B_SPLINE_SURFACE_WITH_KNOTS('',3,3,((#38729,#38730,#38731,#38732,#38733,
#38734),(#38735,#38736,#38737,#38738,#38739,#38740),(#38741,#38742,#38743,
#38744,#38745,#38746),(#38747,#38748,#38749,#38750,#38751,#38752)),
 .UNSPECIFIED.,.F.,.F.,.F.,(4,4),(4,1,1,4),(0.,1.),(-1.75610615531806,-1.00348923161032,
-0.501744615805159,2.22044604925036E-16),.UNSPECIFIED.);
#498=B_SPLINE_SURFACE_WITH_KNOTS('',3,3,((#38856,#38857,#38858,#38859,#38860,
#38861),(#38862,#38863,#38864,#38865,#38866,#38867),(#38868,#38869,#38870,
#38871,#38872,#38873),(#38874,#38875,#38876,#38877,#38878,#38879)),
 .UNSPECIFIED.,.F.,.F.,.F.,(4,4),(4,1,1,4),(0.,1.),(0.,0.571428571428571,
0.857142857142857,1.),.UNSPECIFIED.);
#499=B_SPLINE_SURFACE_WITH_KNOTS('',3,3,((#38940,#38941,#38942,#38943,#38944,
#38945,#38946),(#38947,#38948,#38949,#38950,#38951,#38952,#38953),(#38954,
#38955,#38956,#38957,#38958,#38959,#38960),(#38961,#38962,#38963,#38964,
#38965,#38966,#38967)),.UNSPECIFIED.,.F.,.F.,.F.,(4,4),(4,1,1,1,4),(0.,
1.),(-1.75610615531806,-1.2543615395129,-0.752616923707738,-0.501744615805159,
4.16333634234434E-16),.UNSPECIFIED.);
#500=B_SPLINE_SURFACE_WITH_KNOTS('',3,3,((#38998,#38999,#39000,#39001,#39002,
#39003),(#39004,#39005,#39006,#39007,#39008,#39009),(#39010,#39011,#39012,
#39013,#39014,#39015),(#39016,#39017,#39018,#39019,#39020,#39021)),
 .UNSPECIFIED.,.F.,.F.,.F.,(4,4),(4,1,1,4),(0.,1.),(0.,0.571428571428571,
0.857142857142857,1.),.UNSPECIFIED.);
#501=B_SPLINE_SURFACE_WITH_KNOTS('',3,3,((#39141,#39142,#39143,#39144,#39145,
#39146),(#39147,#39148,#39149,#39150,#39151,#39152),(#39153,#39154,#39155,
#39156,#39157,#39158),(#39159,#39160,#39161,#39162,#39163,#39164)),
 .UNSPECIFIED.,.F.,.F.,.F.,(4,4),(4,1,1,4),(0.,1.),(-1.75610615531806,-1.00348923161032,
-0.501744615805159,2.77555756156289E-17),.UNSPECIFIED.);
#502=B_SPLINE_SURFACE_WITH_KNOTS('',3,3,((#39202,#39203,#39204,#39205,#39206,
#39207),(#39208,#39209,#39210,#39211,#39212,#39213),(#39214,#39215,#39216,
#39217,#39218,#39219),(#39220,#39221,#39222,#39223,#39224,#39225)),
 .UNSPECIFIED.,.F.,.F.,.F.,(4,4),(4,1,1,4),(0.,1.),(0.,0.571428571428571,
0.857142857142857,1.),.UNSPECIFIED.);
#503=B_SPLINE_SURFACE_WITH_KNOTS('',3,3,((#39345,#39346,#39347,#39348,#39349,
#39350),(#39351,#39352,#39353,#39354,#39355,#39356),(#39357,#39358,#39359,
#39360,#39361,#39362),(#39363,#39364,#39365,#39366,#39367,#39368)),
 .UNSPECIFIED.,.F.,.F.,.F.,(4,4),(4,1,1,4),(0.,1.),(-1.75610615531806,-1.00348923161032,
-0.501744615805159,2.77555756156289E-17),.UNSPECIFIED.);
#504=B_SPLINE_SURFACE_WITH_KNOTS('',3,3,((#39469,#39470,#39471,#39472,#39473,
#39474),(#39475,#39476,#39477,#39478,#39479,#39480),(#39481,#39482,#39483,
#39484,#39485,#39486),(#39487,#39488,#39489,#39490,#39491,#39492)),
 .UNSPECIFIED.,.F.,.F.,.F.,(4,4),(4,1,1,4),(0.,1.),(0.,0.571428571428571,
0.857142857142857,1.),.UNSPECIFIED.);
#505=B_SPLINE_SURFACE_WITH_KNOTS('',3,3,((#39553,#39554,#39555,#39556,#39557,
#39558),(#39559,#39560,#39561,#39562,#39563,#39564),(#39565,#39566,#39567,
#39568,#39569,#39570),(#39571,#39572,#39573,#39574,#39575,#39576)),
 .UNSPECIFIED.,.F.,.F.,.F.,(4,4),(4,1,1,4),(0.,1.),(-1.75610615531806,-1.00348923161032,
-0.501744615805159,1.27116549159798E-31),.UNSPECIFIED.);
#506=B_SPLINE_SURFACE_WITH_KNOTS('',3,3,((#39606,#39607,#39608,#39609,#39610,
#39611),(#39612,#39613,#39614,#39615,#39616,#39617),(#39618,#39619,#39620,
#39621,#39622,#39623),(#39624,#39625,#39626,#39627,#39628,#39629)),
 .UNSPECIFIED.,.F.,.F.,.F.,(4,4),(4,1,1,4),(0.,1.),(0.,0.571428571428571,
0.857142857142857,1.),.UNSPECIFIED.);
#507=B_SPLINE_SURFACE_WITH_KNOTS('',3,3,((#39749,#39750,#39751,#39752,#39753,
#39754,#39755),(#39756,#39757,#39758,#39759,#39760,#39761,#39762),(#39763,
#39764,#39765,#39766,#39767,#39768,#39769),(#39770,#39771,#39772,#39773,
#39774,#39775,#39776)),.UNSPECIFIED.,.F.,.F.,.F.,(4,4),(4,1,1,1,4),(0.,
1.),(-1.75610615531805,-1.25436153951289,-0.752616923707736,-0.501744615805158,
1.11022302462516E-16),.UNSPECIFIED.);
#508=B_SPLINE_SURFACE_WITH_KNOTS('',3,3,((#39880,#39881,#39882,#39883,#39884,
#39885),(#39886,#39887,#39888,#39889,#39890,#39891),(#39892,#39893,#39894,
#39895,#39896,#39897),(#39898,#39899,#39900,#39901,#39902,#39903)),
 .UNSPECIFIED.,.F.,.F.,.F.,(4,4),(4,1,1,4),(0.,1.),(0.,0.571428571428571,
0.857142857142857,1.),.UNSPECIFIED.);
#509=B_SPLINE_SURFACE_WITH_KNOTS('',3,3,((#39964,#39965,#39966,#39967,#39968,
#39969,#39970),(#39971,#39972,#39973,#39974,#39975,#39976,#39977),(#39978,
#39979,#39980,#39981,#39982,#39983,#39984),(#39985,#39986,#39987,#39988,
#39989,#39990,#39991)),.UNSPECIFIED.,.F.,.F.,.F.,(4,4),(4,1,1,1,4),(0.,
1.),(-1.75610615531806,-1.2543615395129,-0.752616923707739,-0.501744615805159,
4.10679309198325E-32),.UNSPECIFIED.);
#510=B_SPLINE_SURFACE_WITH_KNOTS('',2,1,((#40770,#40771),(#40772,#40773),
(#40774,#40775)),.UNSPECIFIED.,.F.,.F.,.F.,(3,3),(2,2),(0.,1.),(0.,0.05),
 .UNSPECIFIED.);
#511=B_SPLINE_SURFACE_WITH_KNOTS('',2,1,((#40783,#40784),(#40785,#40786),
(#40787,#40788)),.UNSPECIFIED.,.F.,.F.,.F.,(3,3),(2,2),(0.,1.),(0.,0.05),
 .UNSPECIFIED.);
#512=B_SPLINE_SURFACE_WITH_KNOTS('',2,1,((#40794,#40795),(#40796,#40797),
(#40798,#40799)),.UNSPECIFIED.,.F.,.F.,.F.,(3,3),(2,2),(0.,1.),(0.,0.05),
 .UNSPECIFIED.);
#513=B_SPLINE_SURFACE_WITH_KNOTS('',2,1,((#40805,#40806),(#40807,#40808),
(#40809,#40810)),.UNSPECIFIED.,.F.,.F.,.F.,(3,3),(2,2),(0.,1.),(0.,0.05),
 .UNSPECIFIED.);
#514=B_SPLINE_SURFACE_WITH_KNOTS('',2,1,((#40816,#40817),(#40818,#40819),
(#40820,#40821)),.UNSPECIFIED.,.F.,.F.,.F.,(3,3),(2,2),(0.,1.),(0.,0.05),
 .UNSPECIFIED.);
#515=B_SPLINE_SURFACE_WITH_KNOTS('',2,1,((#40827,#40828),(#40829,#40830),
(#40831,#40832)),.UNSPECIFIED.,.F.,.F.,.F.,(3,3),(2,2),(0.,1.),(0.,0.05),
 .UNSPECIFIED.);
#516=B_SPLINE_SURFACE_WITH_KNOTS('',2,1,((#40838,#40839),(#40840,#40841),
(#40842,#40843)),.UNSPECIFIED.,.F.,.F.,.F.,(3,3),(2,2),(0.,1.),(0.,0.05),
 .UNSPECIFIED.);
#517=B_SPLINE_SURFACE_WITH_KNOTS('',2,1,((#40849,#40850),(#40851,#40852),
(#40853,#40854)),.UNSPECIFIED.,.F.,.F.,.F.,(3,3),(2,2),(0.,1.),(0.,0.05),
 .UNSPECIFIED.);
#518=B_SPLINE_SURFACE_WITH_KNOTS('',2,1,((#40860,#40861),(#40862,#40863),
(#40864,#40865)),.UNSPECIFIED.,.F.,.F.,.F.,(3,3),(2,2),(0.,1.),(0.,0.05),
 .UNSPECIFIED.);
#519=B_SPLINE_SURFACE_WITH_KNOTS('',2,1,((#40871,#40872),(#40873,#40874),
(#40875,#40876)),.UNSPECIFIED.,.F.,.F.,.F.,(3,3),(2,2),(0.,1.),(0.,0.05),
 .UNSPECIFIED.);
#520=B_SPLINE_SURFACE_WITH_KNOTS('',2,1,((#40888,#40889),(#40890,#40891),
(#40892,#40893)),.UNSPECIFIED.,.F.,.F.,.F.,(3,3),(2,2),(0.,1.),(0.,0.05),
 .UNSPECIFIED.);
#521=B_SPLINE_SURFACE_WITH_KNOTS('',2,1,((#40898,#40899),(#40900,#40901),
(#40902,#40903)),.UNSPECIFIED.,.F.,.F.,.F.,(3,3),(2,2),(0.,1.),(0.,0.05),
 .UNSPECIFIED.);
#522=B_SPLINE_SURFACE_WITH_KNOTS('',2,1,((#40911,#40912),(#40913,#40914),
(#40915,#40916)),.UNSPECIFIED.,.F.,.F.,.F.,(3,3),(2,2),(0.,1.),(0.,0.05),
 .UNSPECIFIED.);
#523=B_SPLINE_SURFACE_WITH_KNOTS('',2,1,((#40922,#40923),(#40924,#40925),
(#40926,#40927)),.UNSPECIFIED.,.F.,.F.,.F.,(3,3),(2,2),(0.,1.),(0.,0.05),
 .UNSPECIFIED.);
#524=B_SPLINE_SURFACE_WITH_KNOTS('',2,1,((#40933,#40934),(#40935,#40936),
(#40937,#40938)),.UNSPECIFIED.,.F.,.F.,.F.,(3,3),(2,2),(0.,1.),(0.,0.05),
 .UNSPECIFIED.);
#525=B_SPLINE_SURFACE_WITH_KNOTS('',2,1,((#40944,#40945),(#40946,#40947),
(#40948,#40949)),.UNSPECIFIED.,.F.,.F.,.F.,(3,3),(2,2),(0.,1.),(0.,0.05),
 .UNSPECIFIED.);
#526=B_SPLINE_SURFACE_WITH_KNOTS('',2,1,((#40955,#40956),(#40957,#40958),
(#40959,#40960)),.UNSPECIFIED.,.F.,.F.,.F.,(3,3),(2,2),(0.,1.),(0.,0.05),
 .UNSPECIFIED.);
#527=B_SPLINE_SURFACE_WITH_KNOTS('',2,1,((#40966,#40967),(#40968,#40969),
(#40970,#40971)),.UNSPECIFIED.,.F.,.F.,.F.,(3,3),(2,2),(0.,1.),(0.,0.05),
 .UNSPECIFIED.);
#528=B_SPLINE_SURFACE_WITH_KNOTS('',2,1,((#40977,#40978),(#40979,#40980),
(#40981,#40982)),.UNSPECIFIED.,.F.,.F.,.F.,(3,3),(2,2),(0.,1.),(0.,0.05),
 .UNSPECIFIED.);
#529=B_SPLINE_SURFACE_WITH_KNOTS('',2,1,((#40988,#40989),(#40990,#40991),
(#40992,#40993)),.UNSPECIFIED.,.F.,.F.,.F.,(3,3),(2,2),(0.,1.),(0.,0.05),
 .UNSPECIFIED.);
#530=B_SPLINE_SURFACE_WITH_KNOTS('',2,1,((#40999,#41000),(#41001,#41002),
(#41003,#41004)),.UNSPECIFIED.,.F.,.F.,.F.,(3,3),(2,2),(0.,1.),(0.,0.05),
 .UNSPECIFIED.);
#531=B_SPLINE_SURFACE_WITH_KNOTS('',2,1,((#41010,#41011),(#41012,#41013),
(#41014,#41015)),.UNSPECIFIED.,.F.,.F.,.F.,(3,3),(2,2),(0.,1.),(0.,0.05),
 .UNSPECIFIED.);
#532=B_SPLINE_SURFACE_WITH_KNOTS('',2,1,((#41021,#41022),(#41023,#41024),
(#41025,#41026)),.UNSPECIFIED.,.F.,.F.,.F.,(3,3),(2,2),(0.,1.),(0.,0.05),
 .UNSPECIFIED.);
#533=B_SPLINE_SURFACE_WITH_KNOTS('',2,1,((#41032,#41033),(#41034,#41035),
(#41036,#41037)),.UNSPECIFIED.,.F.,.F.,.F.,(3,3),(2,2),(0.,1.),(0.,0.05),
 .UNSPECIFIED.);
#534=B_SPLINE_SURFACE_WITH_KNOTS('',2,1,((#41047,#41048),(#41049,#41050),
(#41051,#41052)),.UNSPECIFIED.,.F.,.F.,.F.,(3,3),(2,2),(0.,1.),(0.,0.05),
 .UNSPECIFIED.);
#535=B_SPLINE_SURFACE_WITH_KNOTS('',2,1,((#41058,#41059),(#41060,#41061),
(#41062,#41063)),.UNSPECIFIED.,.F.,.F.,.F.,(3,3),(2,2),(0.,1.),(0.,0.05),
 .UNSPECIFIED.);
#536=B_SPLINE_SURFACE_WITH_KNOTS('',2,1,((#41069,#41070),(#41071,#41072),
(#41073,#41074)),.UNSPECIFIED.,.F.,.F.,.F.,(3,3),(2,2),(0.,1.),(0.,0.05),
 .UNSPECIFIED.);
#537=B_SPLINE_SURFACE_WITH_KNOTS('',2,1,((#41080,#41081),(#41082,#41083),
(#41084,#41085)),.UNSPECIFIED.,.F.,.F.,.F.,(3,3),(2,2),(0.,1.),(0.,0.05),
 .UNSPECIFIED.);
#538=B_SPLINE_SURFACE_WITH_KNOTS('',2,1,((#41091,#41092),(#41093,#41094),
(#41095,#41096)),.UNSPECIFIED.,.F.,.F.,.F.,(3,3),(2,2),(0.,1.),(0.,0.05),
 .UNSPECIFIED.);
#539=B_SPLINE_SURFACE_WITH_KNOTS('',2,1,((#41102,#41103),(#41104,#41105),
(#41106,#41107)),.UNSPECIFIED.,.F.,.F.,.F.,(3,3),(2,2),(0.,1.),(0.,0.05),
 .UNSPECIFIED.);
#540=B_SPLINE_SURFACE_WITH_KNOTS('',2,1,((#41113,#41114),(#41115,#41116),
(#41117,#41118)),.UNSPECIFIED.,.F.,.F.,.F.,(3,3),(2,2),(0.,1.),(0.,0.05),
 .UNSPECIFIED.);
#541=B_SPLINE_SURFACE_WITH_KNOTS('',2,1,((#41124,#41125),(#41126,#41127),
(#41128,#41129)),.UNSPECIFIED.,.F.,.F.,.F.,(3,3),(2,2),(0.,1.),(0.,0.05),
 .UNSPECIFIED.);
#542=B_SPLINE_SURFACE_WITH_KNOTS('',2,1,((#41135,#41136),(#41137,#41138),
(#41139,#41140)),.UNSPECIFIED.,.F.,.F.,.F.,(3,3),(2,2),(0.,1.),(0.,0.05),
 .UNSPECIFIED.);
#543=B_SPLINE_SURFACE_WITH_KNOTS('',2,1,((#41146,#41147),(#41148,#41149),
(#41150,#41151)),.UNSPECIFIED.,.F.,.F.,.F.,(3,3),(2,2),(0.,1.),(0.,0.05),
 .UNSPECIFIED.);
#544=B_SPLINE_SURFACE_WITH_KNOTS('',2,1,((#41157,#41158),(#41159,#41160),
(#41161,#41162)),.UNSPECIFIED.,.F.,.F.,.F.,(3,3),(2,2),(0.,1.),(0.,0.05),
 .UNSPECIFIED.);
#545=B_SPLINE_SURFACE_WITH_KNOTS('',2,1,((#41168,#41169),(#41170,#41171),
(#41172,#41173)),.UNSPECIFIED.,.F.,.F.,.F.,(3,3),(2,2),(0.,1.),(0.,0.05),
 .UNSPECIFIED.);
#546=B_SPLINE_SURFACE_WITH_KNOTS('',2,1,((#41179,#41180),(#41181,#41182),
(#41183,#41184)),.UNSPECIFIED.,.F.,.F.,.F.,(3,3),(2,2),(0.,1.),(0.,0.05),
 .UNSPECIFIED.);
#547=B_SPLINE_SURFACE_WITH_KNOTS('',2,1,((#41190,#41191),(#41192,#41193),
(#41194,#41195)),.UNSPECIFIED.,.F.,.F.,.F.,(3,3),(2,2),(0.,1.),(0.,0.05),
 .UNSPECIFIED.);
#548=B_SPLINE_SURFACE_WITH_KNOTS('',2,1,((#41201,#41202),(#41203,#41204),
(#41205,#41206)),.UNSPECIFIED.,.F.,.F.,.F.,(3,3),(2,2),(0.,1.),(0.,0.05),
 .UNSPECIFIED.);
#549=B_SPLINE_SURFACE_WITH_KNOTS('',2,1,((#41212,#41213),(#41214,#41215),
(#41216,#41217)),.UNSPECIFIED.,.F.,.F.,.F.,(3,3),(2,2),(0.,1.),(0.,0.05),
 .UNSPECIFIED.);
#550=B_SPLINE_SURFACE_WITH_KNOTS('',2,1,((#41223,#41224),(#41225,#41226),
(#41227,#41228)),.UNSPECIFIED.,.F.,.F.,.F.,(3,3),(2,2),(0.,1.),(0.,0.05),
 .UNSPECIFIED.);
#551=B_SPLINE_SURFACE_WITH_KNOTS('',2,1,((#41234,#41235),(#41236,#41237),
(#41238,#41239)),.UNSPECIFIED.,.F.,.F.,.F.,(3,3),(2,2),(0.,1.),(0.,0.05),
 .UNSPECIFIED.);
#552=B_SPLINE_SURFACE_WITH_KNOTS('',2,1,((#41249,#41250),(#41251,#41252),
(#41253,#41254)),.UNSPECIFIED.,.F.,.F.,.F.,(3,3),(2,2),(0.,1.),(0.,0.05),
 .UNSPECIFIED.);
#553=B_SPLINE_SURFACE_WITH_KNOTS('',2,1,((#41260,#41261),(#41262,#41263),
(#41264,#41265)),.UNSPECIFIED.,.F.,.F.,.F.,(3,3),(2,2),(0.,1.),(0.,0.05),
 .UNSPECIFIED.);
#554=B_SPLINE_SURFACE_WITH_KNOTS('',2,1,((#41276,#41277),(#41278,#41279),
(#41280,#41281)),.UNSPECIFIED.,.F.,.F.,.F.,(3,3),(2,2),(0.,1.),(0.,0.05),
 .UNSPECIFIED.);
#555=B_SPLINE_SURFACE_WITH_KNOTS('',2,1,((#41287,#41288),(#41289,#41290),
(#41291,#41292)),.UNSPECIFIED.,.F.,.F.,.F.,(3,3),(2,2),(0.,1.),(0.,0.05),
 .UNSPECIFIED.);
#556=B_SPLINE_SURFACE_WITH_KNOTS('',2,1,((#41298,#41299),(#41300,#41301),
(#41302,#41303)),.UNSPECIFIED.,.F.,.F.,.F.,(3,3),(2,2),(0.,1.),(0.,0.05),
 .UNSPECIFIED.);
#557=B_SPLINE_SURFACE_WITH_KNOTS('',2,1,((#41309,#41310),(#41311,#41312),
(#41313,#41314)),.UNSPECIFIED.,.F.,.F.,.F.,(3,3),(2,2),(0.,1.),(0.,0.05),
 .UNSPECIFIED.);
#558=B_SPLINE_SURFACE_WITH_KNOTS('',2,1,((#41326,#41327),(#41328,#41329),
(#41330,#41331)),.UNSPECIFIED.,.F.,.F.,.F.,(3,3),(2,2),(0.,1.),(0.,0.05),
 .UNSPECIFIED.);
#559=B_SPLINE_SURFACE_WITH_KNOTS('',2,1,((#41337,#41338),(#41339,#41340),
(#41341,#41342)),.UNSPECIFIED.,.F.,.F.,.F.,(3,3),(2,2),(0.,1.),(0.,0.05),
 .UNSPECIFIED.);
#560=B_SPLINE_SURFACE_WITH_KNOTS('',2,1,((#41348,#41349),(#41350,#41351),
(#41352,#41353)),.UNSPECIFIED.,.F.,.F.,.F.,(3,3),(2,2),(0.,1.),(0.,0.05),
 .UNSPECIFIED.);
#561=B_SPLINE_SURFACE_WITH_KNOTS('',2,1,((#41359,#41360),(#41361,#41362),
(#41363,#41364)),.UNSPECIFIED.,.F.,.F.,.F.,(3,3),(2,2),(0.,1.),(0.,0.05),
 .UNSPECIFIED.);
#562=B_SPLINE_SURFACE_WITH_KNOTS('',2,1,((#41370,#41371),(#41372,#41373),
(#41374,#41375)),.UNSPECIFIED.,.F.,.F.,.F.,(3,3),(2,2),(0.,1.),(0.,0.05),
 .UNSPECIFIED.);
#563=B_SPLINE_SURFACE_WITH_KNOTS('',2,1,((#41381,#41382),(#41383,#41384),
(#41385,#41386)),.UNSPECIFIED.,.F.,.F.,.F.,(3,3),(2,2),(0.,1.),(0.,0.05),
 .UNSPECIFIED.);
#564=B_SPLINE_SURFACE_WITH_KNOTS('',2,1,((#41392,#41393),(#41394,#41395),
(#41396,#41397)),.UNSPECIFIED.,.F.,.F.,.F.,(3,3),(2,2),(0.,1.),(0.,0.05),
 .UNSPECIFIED.);
#565=B_SPLINE_SURFACE_WITH_KNOTS('',2,1,((#41426,#41427),(#41428,#41429),
(#41430,#41431)),.UNSPECIFIED.,.F.,.F.,.F.,(3,3),(2,2),(0.,1.),(0.,0.05),
 .UNSPECIFIED.);
#566=B_SPLINE_SURFACE_WITH_KNOTS('',2,1,((#41437,#41438),(#41439,#41440),
(#41441,#41442)),.UNSPECIFIED.,.F.,.F.,.F.,(3,3),(2,2),(0.,1.),(0.,0.05),
 .UNSPECIFIED.);
#567=B_SPLINE_SURFACE_WITH_KNOTS('',3,3,((#41593,#41594,#41595,#41596),
(#41597,#41598,#41599,#41600),(#41601,#41602,#41603,#41604),(#41605,#41606,
#41607,#41608)),.UNSPECIFIED.,.F.,.F.,.F.,(4,4),(4,4),(0.,1.),(-3.32291242799128,
-2.9602728791883),.UNSPECIFIED.);
#568=B_SPLINE_SURFACE_WITH_KNOTS('',3,3,((#41671,#41672,#41673,#41674),
(#41675,#41676,#41677,#41678),(#41679,#41680,#41681,#41682),(#41683,#41684,
#41685,#41686)),.UNSPECIFIED.,.F.,.F.,.F.,(4,4),(4,4),(0.,1.),(-0.181319774401488,
0.181319774401493),.UNSPECIFIED.);
#569=B_SPLINE_SURFACE_WITH_KNOTS('',3,3,((#41713,#41714,#41715,#41716),
(#41717,#41718,#41719,#41720),(#41721,#41722,#41723,#41724),(#41725,#41726,
#41727,#41728)),.UNSPECIFIED.,.F.,.F.,.F.,(4,4),(4,4),(0.,1.),(-3.32291242799128,
-2.9602728791883),.UNSPECIFIED.);
#570=B_SPLINE_SURFACE_WITH_KNOTS('',3,3,((#41754,#41755,#41756,#41757),
(#41758,#41759,#41760,#41761),(#41762,#41763,#41764,#41765),(#41766,#41767,
#41768,#41769)),.UNSPECIFIED.,.F.,.F.,.F.,(4,4),(4,4),(0.,1.),(-6.46450508158109,
-6.10186553277809),.UNSPECIFIED.);
#571=B_SPLINE_SURFACE_WITH_KNOTS('',3,3,((#45582,#45583,#45584,#45585,#45586,
#45587),(#45588,#45589,#45590,#45591,#45592,#45593),(#45594,#45595,#45596,
#45597,#45598,#45599),(#45600,#45601,#45602,#45603,#45604,#45605)),
 .UNSPECIFIED.,.F.,.F.,.F.,(4,4),(4,1,1,4),(0.,1.),(0.217693875784178,0.975255008179982,
1.48029576311052,1.98533651804105),.UNSPECIFIED.);
#572=B_SPLINE_SURFACE_WITH_KNOTS('',3,3,((#45618,#45619,#45620,#45621,#45622,
#45623),(#45624,#45625,#45626,#45627,#45628,#45629),(#45630,#45631,#45632,
#45633,#45634,#45635),(#45636,#45637,#45638,#45639,#45640,#45641)),
 .UNSPECIFIED.,.F.,.F.,.F.,(4,4),(4,1,1,4),(0.,1.),(0.217693875784177,0.975255008179981,
1.48029576311052,1.98533651804105),.UNSPECIFIED.);
#573=B_SPLINE_SURFACE_WITH_KNOTS('',3,3,((#45648,#45649,#45650,#45651,#45652,
#45653),(#45654,#45655,#45656,#45657,#45658,#45659),(#45660,#45661,#45662,
#45663,#45664,#45665),(#45666,#45667,#45668,#45669,#45670,#45671)),
 .UNSPECIFIED.,.F.,.F.,.F.,(4,4),(4,1,1,4),(0.,1.),(0.217693875784177,0.975255008179981,
1.48029576311052,1.98533651804105),.UNSPECIFIED.);
#574=B_SPLINE_SURFACE_WITH_KNOTS('',3,3,((#45690,#45691,#45692,#45693,#45694,
#45695),(#45696,#45697,#45698,#45699,#45700,#45701),(#45702,#45703,#45704,
#45705,#45706,#45707),(#45708,#45709,#45710,#45711,#45712,#45713)),
 .UNSPECIFIED.,.F.,.F.,.F.,(4,4),(4,1,1,4),(0.,1.),(0.217693875784176,0.975255008179981,
1.48029576311052,1.98533651804105),.UNSPECIFIED.);
#575=B_SPLINE_SURFACE_WITH_KNOTS('',3,3,((#45720,#45721,#45722,#45723,#45724,
#45725),(#45726,#45727,#45728,#45729,#45730,#45731),(#45732,#45733,#45734,
#45735,#45736,#45737),(#45738,#45739,#45740,#45741,#45742,#45743)),
 .UNSPECIFIED.,.F.,.F.,.F.,(4,4),(4,1,1,4),(0.,1.),(0.217693875784177,0.975255008179981,
1.48029576311052,1.98533651804105),.UNSPECIFIED.);
#576=B_SPLINE_SURFACE_WITH_KNOTS('',3,3,((#45762,#45763,#45764,#45765,#45766,
#45767),(#45768,#45769,#45770,#45771,#45772,#45773),(#45774,#45775,#45776,
#45777,#45778,#45779),(#45780,#45781,#45782,#45783,#45784,#45785)),
 .UNSPECIFIED.,.F.,.F.,.F.,(4,4),(4,1,1,4),(0.,1.),(0.217693875784176,0.975255008179981,
1.48029576311052,1.98533651804105),.UNSPECIFIED.);
#577=B_SPLINE_SURFACE_WITH_KNOTS('',3,3,((#46525,#46526,#46527,#46528,#46529,
#46530,#46531,#46532,#46533,#46534,#46535,#46536,#46537,#46538,#46539,#46540,
#46541,#46542,#46543,#46544,#46545,#46546,#46547,#46548,#46549,#46550,#46551,
#46552,#46553,#46554),(#46555,#46556,#46557,#46558,#46559,#46560,#46561,
#46562,#46563,#46564,#46565,#46566,#46567,#46568,#46569,#46570,#46571,#46572,
#46573,#46574,#46575,#46576,#46577,#46578,#46579,#46580,#46581,#46582,#46583,
#46584),(#46585,#46586,#46587,#46588,#46589,#46590,#46591,#46592,#46593,
#46594,#46595,#46596,#46597,#46598,#46599,#46600,#46601,#46602,#46603,#46604,
#46605,#46606,#46607,#46608,#46609,#46610,#46611,#46612,#46613,#46614),
(#46615,#46616,#46617,#46618,#46619,#46620,#46621,#46622,#46623,#46624,
#46625,#46626,#46627,#46628,#46629,#46630,#46631,#46632,#46633,#46634,#46635,
#46636,#46637,#46638,#46639,#46640,#46641,#46642,#46643,#46644)),
 .UNSPECIFIED.,.F.,.T.,.F.,(4,4),(4,2,2,1,2,1,1,1,1,1,1,1,1,1,2,1,2,2,1,
1,1,4),(0.,1.),(1.53893133527844,1.66717486055154,1.79541838582463,1.92366341643128,
2.05190844703792,2.16412209615196,2.276335745266,2.33244256982302,2.38854939438004,
2.50076304349408,2.52881645577259,2.5568698680511,2.61297669260812,2.72519034172216,
2.94961763995024,3.01374015525356,3.07786267055688,3.20610770116353,3.30229072145174,
3.39847374173995,3.44656525188405,3.59083978231636),.UNSPECIFIED.);
#578=B_SPLINE_SURFACE_WITH_KNOTS('',3,3,((#48148,#48149,#48150,#48151,#48152,
#48153,#48154,#48155,#48156,#48157,#48158,#48159,#48160,#48161,#48162,#48163,
#48164,#48165,#48166,#48167,#48168,#48169,#48170,#48171,#48172,#48173,#48174,
#48175,#48176,#48177,#48178,#48179,#48180,#48181,#48182,#48183,#48184,#48185,
#48186,#48187,#48188,#48189,#48190,#48191,#48192,#48193,#48194,#48195,#48196,
#48197,#48198,#48199,#48200,#48201,#48202,#48203,#48204,#48205,#48206,#48207,
#48208,#48209,#48210,#48211,#48212,#48213,#48214,#48215,#48216,#48217,#48218,
#48219,#48220,#48221,#48222,#48223,#48224,#48225,#48226,#48227,#48228,#48229,
#48230,#48231,#48232,#48233,#48234,#48235,#48236,#48237,#48238,#48239,#48240,
#48241,#48242,#48243,#48244,#48245,#48246,#48247,#48248,#48249,#48250,#48251,
#48252,#48253,#48254,#48255,#48256,#48257,#48258,#48259,#48260,#48261,#48262,
#48263,#48264,#48265,#48266,#48267,#48268,#48269,#48270,#48271,#48272,#48273,
#48274,#48275,#48276,#48277,#48278),(#48279,#48280,#48281,#48282,#48283,
#48284,#48285,#48286,#48287,#48288,#48289,#48290,#48291,#48292,#48293,#48294,
#48295,#48296,#48297,#48298,#48299,#48300,#48301,#48302,#48303,#48304,#48305,
#48306,#48307,#48308,#48309,#48310,#48311,#48312,#48313,#48314,#48315,#48316,
#48317,#48318,#48319,#48320,#48321,#48322,#48323,#48324,#48325,#48326,#48327,
#48328,#48329,#48330,#48331,#48332,#48333,#48334,#48335,#48336,#48337,#48338,
#48339,#48340,#48341,#48342,#48343,#48344,#48345,#48346,#48347,#48348,#48349,
#48350,#48351,#48352,#48353,#48354,#48355,#48356,#48357,#48358,#48359,#48360,
#48361,#48362,#48363,#48364,#48365,#48366,#48367,#48368,#48369,#48370,#48371,
#48372,#48373,#48374,#48375,#48376,#48377,#48378,#48379,#48380,#48381,#48382,
#48383,#48384,#48385,#48386,#48387,#48388,#48389,#48390,#48391,#48392,#48393,
#48394,#48395,#48396,#48397,#48398,#48399,#48400,#48401,#48402,#48403,#48404,
#48405,#48406,#48407,#48408,#48409),(#48410,#48411,#48412,#48413,#48414,
#48415,#48416,#48417,#48418,#48419,#48420,#48421,#48422,#48423,#48424,#48425,
#48426,#48427,#48428,#48429,#48430,#48431,#48432,#48433,#48434,#48435,#48436,
#48437,#48438,#48439,#48440,#48441,#48442,#48443,#48444,#48445,#48446,#48447,
#48448,#48449,#48450,#48451,#48452,#48453,#48454,#48455,#48456,#48457,#48458,
#48459,#48460,#48461,#48462,#48463,#48464,#48465,#48466,#48467,#48468,#48469,
#48470,#48471,#48472,#48473,#48474,#48475,#48476,#48477,#48478,#48479,#48480,
#48481,#48482,#48483,#48484,#48485,#48486,#48487,#48488,#48489,#48490,#48491,
#48492,#48493,#48494,#48495,#48496,#48497,#48498,#48499,#48500,#48501,#48502,
#48503,#48504,#48505,#48506,#48507,#48508,#48509,#48510,#48511,#48512,#48513,
#48514,#48515,#48516,#48517,#48518,#48519,#48520,#48521,#48522,#48523,#48524,
#48525,#48526,#48527,#48528,#48529,#48530,#48531,#48532,#48533,#48534,#48535,
#48536,#48537,#48538,#48539,#48540),(#48541,#48542,#48543,#48544,#48545,
#48546,#48547,#48548,#48549,#48550,#48551,#48552,#48553,#48554,#48555,#48556,
#48557,#48558,#48559,#48560,#48561,#48562,#48563,#48564,#48565,#48566,#48567,
#48568,#48569,#48570,#48571,#48572,#48573,#48574,#48575,#48576,#48577,#48578,
#48579,#48580,#48581,#48582,#48583,#48584,#48585,#48586,#48587,#48588,#48589,
#48590,#48591,#48592,#48593,#48594,#48595,#48596,#48597,#48598,#48599,#48600,
#48601,#48602,#48603,#48604,#48605,#48606,#48607,#48608,#48609,#48610,#48611,
#48612,#48613,#48614,#48615,#48616,#48617,#48618,#48619,#48620,#48621,#48622,
#48623,#48624,#48625,#48626,#48627,#48628,#48629,#48630,#48631,#48632,#48633,
#48634,#48635,#48636,#48637,#48638,#48639,#48640,#48641,#48642,#48643,#48644,
#48645,#48646,#48647,#48648,#48649,#48650,#48651,#48652,#48653,#48654,#48655,
#48656,#48657,#48658,#48659,#48660,#48661,#48662,#48663,#48664,#48665,#48666,
#48667,#48668,#48669,#48670,#48671)),.UNSPECIFIED.,.F.,.F.,.F.,(4,4),(4,
1,1,1,1,1,1,1,1,1,1,1,1,1,1,1,1,1,1,1,1,1,1,1,1,1,1,1,1,1,1,1,1,1,1,1,1,
1,1,1,1,1,1,1,1,1,1,1,1,1,1,1,1,1,1,1,1,1,1,1,1,1,1,1,1,1,1,1,1,1,1,1,1,
1,1,1,1,1,1,1,1,1,1,1,1,1,1,1,1,1,1,1,1,1,1,1,1,1,1,1,1,1,1,1,1,1,1,1,1,
1,1,1,1,1,1,1,1,1,1,1,1,1,1,1,1,1,1,1,4),(0.,0.0986691610045069),(8.3098959515533,
8.80969750862556,9.30949906569782,10.3091021798423,11.3087052939868,12.3083084081313,
13.3079115222759,14.3075146364204,15.3071177505649,16.3067208647094,17.3063239788539,
18.3059270929984,19.3055302071429,20.3051333212874,21.3047364354319,22.3043395495765,
23.303942663721,24.3035457778655,25.30314889201,26.3027520061545,27.302355120299,
28.3019582344435,29.301561348588,30.3011644627325,31.3007675768771,32.3003706910216,
33.2999738051661,34.2995769193106,35.2991800334551,36.2987831475996,37.2983862617441,
38.2979893758886,39.2975924900331,40.2971956041777,41.2967987183222,42.2964018324667,
43.2960049466112,44.2956080607557,45.2952111749002,46.2948142890447,47.2944174031892,
48.2940205173337,49.2936236314783,50.2932267456228,51.2928298597673,52.2924329739118,
53.2920360880563,54.2916392022008,55.2912423163453,56.2908454304898,57.2904485446343,
58.2900516587789,59.2896547729234,60.2892578870679,61.2888610012124,62.2884641153569,
63.2880672295014,64.2876703436459,65.2872734577904,66.2868765719349,67.2864796860794,
68.286082800224,69.2856859143685,70.285289028513,71.2848921426575,72.284495256802,
73.2840983709465,74.283701485091,75.2833045992355,76.28290771338,77.2825108275245,
78.2821139416691,79.2817170558136,80.2813201699581,81.2809232841026,82.2805263982471,
83.2801295123916,84.2797326265361,85.2793357406806,86.2789388548251,87.2785419689697,
88.2781450831142,89.2777481972587,90.2773513114032,91.2769544255477,92.2765575396922,
93.2761606538367,94.2757637679812,95.2753668821258,96.2749699962703,97.2745731104148,
98.2741762245593,99.2737793387038,100.273382452848,101.272985566993,102.272588681137,
103.272191795282,104.271794909426,105.271398023571,106.271001137715,107.27060425186,
108.270207366004,109.269810480149,110.269413594293,111.269016708438,112.268619822582,
113.268222936727,114.267826050871,115.267429165016,116.26703227916,117.266635393305,
118.26623850745,119.265841621594,120.265444735739,121.265047849883,122.264650964028,
123.264254078172,124.263857192317,125.263460306461,126.263063420606,127.26266653475,
128.262269648895,129.261872763039,130.261475877184,131.261078991328,132.260682105473,
133.260285219617,133.760086776689,134.259888333762),.UNSPECIFIED.);
#579=B_SPLINE_SURFACE_WITH_KNOTS('',3,3,((#49021,#49022,#49023,#49024,#49025,
#49026,#49027,#49028,#49029,#49030,#49031,#49032,#49033,#49034,#49035,#49036,
#49037,#49038,#49039,#49040,#49041,#49042,#49043,#49044,#49045,#49046,#49047,
#49048,#49049,#49050,#49051,#49052,#49053,#49054,#49055,#49056,#49057,#49058,
#49059,#49060,#49061,#49062,#49063,#49064,#49065,#49066,#49067,#49068,#49069,
#49070,#49071,#49072,#49073,#49074,#49075,#49076,#49077,#49078,#49079,#49080,
#49081,#49082,#49083,#49084,#49085,#49086,#49087,#49088,#49089,#49090,#49091,
#49092,#49093,#49094,#49095,#49096,#49097,#49098,#49099,#49100,#49101,#49102,
#49103,#49104,#49105,#49106,#49107,#49108,#49109,#49110,#49111,#49112,#49113,
#49114,#49115,#49116,#49117,#49118,#49119,#49120,#49121,#49122,#49123,#49124,
#49125,#49126,#49127,#49128,#49129,#49130,#49131,#49132,#49133,#49134,#49135,
#49136,#49137,#49138,#49139,#49140,#49141,#49142,#49143,#49144,#49145,#49146,
#49147,#49148,#49149,#49150,#49151),(#49152,#49153,#49154,#49155,#49156,
#49157,#49158,#49159,#49160,#49161,#49162,#49163,#49164,#49165,#49166,#49167,
#49168,#49169,#49170,#49171,#49172,#49173,#49174,#49175,#49176,#49177,#49178,
#49179,#49180,#49181,#49182,#49183,#49184,#49185,#49186,#49187,#49188,#49189,
#49190,#49191,#49192,#49193,#49194,#49195,#49196,#49197,#49198,#49199,#49200,
#49201,#49202,#49203,#49204,#49205,#49206,#49207,#49208,#49209,#49210,#49211,
#49212,#49213,#49214,#49215,#49216,#49217,#49218,#49219,#49220,#49221,#49222,
#49223,#49224,#49225,#49226,#49227,#49228,#49229,#49230,#49231,#49232,#49233,
#49234,#49235,#49236,#49237,#49238,#49239,#49240,#49241,#49242,#49243,#49244,
#49245,#49246,#49247,#49248,#49249,#49250,#49251,#49252,#49253,#49254,#49255,
#49256,#49257,#49258,#49259,#49260,#49261,#49262,#49263,#49264,#49265,#49266,
#49267,#49268,#49269,#49270,#49271,#49272,#49273,#49274,#49275,#49276,#49277,
#49278,#49279,#49280,#49281,#49282),(#49283,#49284,#49285,#49286,#49287,
#49288,#49289,#49290,#49291,#49292,#49293,#49294,#49295,#49296,#49297,#49298,
#49299,#49300,#49301,#49302,#49303,#49304,#49305,#49306,#49307,#49308,#49309,
#49310,#49311,#49312,#49313,#49314,#49315,#49316,#49317,#49318,#49319,#49320,
#49321,#49322,#49323,#49324,#49325,#49326,#49327,#49328,#49329,#49330,#49331,
#49332,#49333,#49334,#49335,#49336,#49337,#49338,#49339,#49340,#49341,#49342,
#49343,#49344,#49345,#49346,#49347,#49348,#49349,#49350,#49351,#49352,#49353,
#49354,#49355,#49356,#49357,#49358,#49359,#49360,#49361,#49362,#49363,#49364,
#49365,#49366,#49367,#49368,#49369,#49370,#49371,#49372,#49373,#49374,#49375,
#49376,#49377,#49378,#49379,#49380,#49381,#49382,#49383,#49384,#49385,#49386,
#49387,#49388,#49389,#49390,#49391,#49392,#49393,#49394,#49395,#49396,#49397,
#49398,#49399,#49400,#49401,#49402,#49403,#49404,#49405,#49406,#49407,#49408,
#49409,#49410,#49411,#49412,#49413),(#49414,#49415,#49416,#49417,#49418,
#49419,#49420,#49421,#49422,#49423,#49424,#49425,#49426,#49427,#49428,#49429,
#49430,#49431,#49432,#49433,#49434,#49435,#49436,#49437,#49438,#49439,#49440,
#49441,#49442,#49443,#49444,#49445,#49446,#49447,#49448,#49449,#49450,#49451,
#49452,#49453,#49454,#49455,#49456,#49457,#49458,#49459,#49460,#49461,#49462,
#49463,#49464,#49465,#49466,#49467,#49468,#49469,#49470,#49471,#49472,#49473,
#49474,#49475,#49476,#49477,#49478,#49479,#49480,#49481,#49482,#49483,#49484,
#49485,#49486,#49487,#49488,#49489,#49490,#49491,#49492,#49493,#49494,#49495,
#49496,#49497,#49498,#49499,#49500,#49501,#49502,#49503,#49504,#49505,#49506,
#49507,#49508,#49509,#49510,#49511,#49512,#49513,#49514,#49515,#49516,#49517,
#49518,#49519,#49520,#49521,#49522,#49523,#49524,#49525,#49526,#49527,#49528,
#49529,#49530,#49531,#49532,#49533,#49534,#49535,#49536,#49537,#49538,#49539,
#49540,#49541,#49542,#49543,#49544)),.UNSPECIFIED.,.F.,.F.,.F.,(4,4),(4,
1,1,1,1,1,1,1,1,1,1,1,1,1,1,1,1,1,1,1,1,1,1,1,1,1,1,1,1,1,1,1,1,1,1,1,1,
1,1,1,1,1,1,1,1,1,1,1,1,1,1,1,1,1,1,1,1,1,1,1,1,1,1,1,1,1,1,1,1,1,1,1,1,
1,1,1,1,1,1,1,1,1,1,1,1,1,1,1,1,1,1,1,1,1,1,1,1,1,1,1,1,1,1,1,1,1,1,1,1,
1,1,1,1,1,1,1,1,1,1,1,1,1,1,1,1,1,1,1,4),(0.,0.0986691610045069),(11.6147305479242,
12.1145321049964,12.6143336620687,13.6139367762132,14.6135398903577,15.6131430045022,
16.6127461186467,17.6123492327912,18.6119523469357,19.6115554610803,20.6111585752248,
21.6107616893693,22.6103648035138,23.6099679176583,24.6095710318028,25.6091741459473,
26.6087772600918,27.6083803742363,28.6079834883808,29.6075866025254,30.6071897166699,
31.6067928308144,32.6063959449589,33.6059990591034,34.6056021732479,35.6052052873924,
36.6048084015369,37.6044115156814,38.604014629826,39.6036177439705,40.603220858115,
41.6028239722595,42.602427086404,43.6020302005485,44.601633314693,45.6012364288375,
46.600839542982,47.6004426571266,48.6000457712711,49.5996488854156,50.5992519995601,
51.5988551137046,52.5984582278491,53.5980613419936,54.5976644561381,55.5972675702826,
56.5968706844272,57.5964737985717,58.5960769127162,59.5956800268607,60.5952831410052,
61.5948862551497,62.5944893692942,63.5940924834387,64.5936955975832,65.5932987117278,
66.5929018258723,67.5925049400168,68.5921080541613,69.5917111683058,70.5913142824503,
71.5909173965948,72.5905205107393,73.5901236248838,74.5897267390284,75.5893298531729,
76.5889329673174,77.5885360814619,78.5881391956064,79.5877423097509,80.5873454238954,
81.5869485380399,82.5865516521845,83.586154766329,84.5857578804735,85.585360994618,
86.5849641087625,87.584567222907,88.5841703370515,89.583773451196,90.5833765653405,
91.582979679485,92.5825827936296,93.5821859077741,94.5817890219186,95.5813921360631,
96.5809952502076,97.5805983643521,98.5802014784966,99.5798045926411,100.579407706786,
101.57901082093,102.578613935075,103.578217049219,104.577820163364,105.577423277508,
106.577026391653,107.576629505797,108.576232619942,109.575835734086,110.575438848231,
111.575041962375,112.57464507652,113.574248190664,114.573851304809,115.573454418953,
116.573057533098,117.572660647242,118.572263761387,119.571866875531,120.571469989676,
121.57107310382,122.570676217965,123.570279332109,124.569882446254,125.569485560398,
126.569088674543,127.568691788687,128.568294902832,129.567898016976,130.567501131121,
131.567104245265,132.56670735941,133.566310473554,134.565913587699,135.565516701844,
136.565119815988,137.06492137306,137.564722930133),.UNSPECIFIED.);
#580=B_SPLINE_SURFACE_WITH_KNOTS('',3,3,((#51175,#51176,#51177,#51178,#51179,
#51180,#51181,#51182,#51183,#51184,#51185,#51186,#51187,#51188,#51189,#51190,
#51191,#51192,#51193,#51194,#51195,#51196,#51197,#51198,#51199,#51200,#51201,
#51202,#51203,#51204,#51205,#51206,#51207,#51208,#51209,#51210,#51211,#51212,
#51213,#51214,#51215,#51216,#51217,#51218,#51219,#51220,#51221,#51222,#51223,
#51224,#51225,#51226,#51227,#51228,#51229,#51230,#51231,#51232,#51233,#51234,
#51235,#51236,#51237,#51238,#51239,#51240,#51241,#51242,#51243,#51244,#51245,
#51246,#51247,#51248,#51249,#51250,#51251,#51252,#51253,#51254,#51255,#51256,
#51257,#51258,#51259,#51260,#51261,#51262,#51263,#51264,#51265,#51266,#51267,
#51268,#51269,#51270,#51271,#51272,#51273,#51274,#51275,#51276,#51277,#51278,
#51279,#51280,#51281,#51282,#51283,#51284,#51285,#51286,#51287,#51288,#51289,
#51290,#51291,#51292,#51293,#51294,#51295,#51296,#51297,#51298,#51299,#51300,
#51301,#51302,#51303,#51304,#51305),(#51306,#51307,#51308,#51309,#51310,
#51311,#51312,#51313,#51314,#51315,#51316,#51317,#51318,#51319,#51320,#51321,
#51322,#51323,#51324,#51325,#51326,#51327,#51328,#51329,#51330,#51331,#51332,
#51333,#51334,#51335,#51336,#51337,#51338,#51339,#51340,#51341,#51342,#51343,
#51344,#51345,#51346,#51347,#51348,#51349,#51350,#51351,#51352,#51353,#51354,
#51355,#51356,#51357,#51358,#51359,#51360,#51361,#51362,#51363,#51364,#51365,
#51366,#51367,#51368,#51369,#51370,#51371,#51372,#51373,#51374,#51375,#51376,
#51377,#51378,#51379,#51380,#51381,#51382,#51383,#51384,#51385,#51386,#51387,
#51388,#51389,#51390,#51391,#51392,#51393,#51394,#51395,#51396,#51397,#51398,
#51399,#51400,#51401,#51402,#51403,#51404,#51405,#51406,#51407,#51408,#51409,
#51410,#51411,#51412,#51413,#51414,#51415,#51416,#51417,#51418,#51419,#51420,
#51421,#51422,#51423,#51424,#51425,#51426,#51427,#51428,#51429,#51430,#51431,
#51432,#51433,#51434,#51435,#51436),(#51437,#51438,#51439,#51440,#51441,
#51442,#51443,#51444,#51445,#51446,#51447,#51448,#51449,#51450,#51451,#51452,
#51453,#51454,#51455,#51456,#51457,#51458,#51459,#51460,#51461,#51462,#51463,
#51464,#51465,#51466,#51467,#51468,#51469,#51470,#51471,#51472,#51473,#51474,
#51475,#51476,#51477,#51478,#51479,#51480,#51481,#51482,#51483,#51484,#51485,
#51486,#51487,#51488,#51489,#51490,#51491,#51492,#51493,#51494,#51495,#51496,
#51497,#51498,#51499,#51500,#51501,#51502,#51503,#51504,#51505,#51506,#51507,
#51508,#51509,#51510,#51511,#51512,#51513,#51514,#51515,#51516,#51517,#51518,
#51519,#51520,#51521,#51522,#51523,#51524,#51525,#51526,#51527,#51528,#51529,
#51530,#51531,#51532,#51533,#51534,#51535,#51536,#51537,#51538,#51539,#51540,
#51541,#51542,#51543,#51544,#51545,#51546,#51547,#51548,#51549,#51550,#51551,
#51552,#51553,#51554,#51555,#51556,#51557,#51558,#51559,#51560,#51561,#51562,
#51563,#51564,#51565,#51566,#51567),(#51568,#51569,#51570,#51571,#51572,
#51573,#51574,#51575,#51576,#51577,#51578,#51579,#51580,#51581,#51582,#51583,
#51584,#51585,#51586,#51587,#51588,#51589,#51590,#51591,#51592,#51593,#51594,
#51595,#51596,#51597,#51598,#51599,#51600,#51601,#51602,#51603,#51604,#51605,
#51606,#51607,#51608,#51609,#51610,#51611,#51612,#51613,#51614,#51615,#51616,
#51617,#51618,#51619,#51620,#51621,#51622,#51623,#51624,#51625,#51626,#51627,
#51628,#51629,#51630,#51631,#51632,#51633,#51634,#51635,#51636,#51637,#51638,
#51639,#51640,#51641,#51642,#51643,#51644,#51645,#51646,#51647,#51648,#51649,
#51650,#51651,#51652,#51653,#51654,#51655,#51656,#51657,#51658,#51659,#51660,
#51661,#51662,#51663,#51664,#51665,#51666,#51667,#51668,#51669,#51670,#51671,
#51672,#51673,#51674,#51675,#51676,#51677,#51678,#51679,#51680,#51681,#51682,
#51683,#51684,#51685,#51686,#51687,#51688,#51689,#51690,#51691,#51692,#51693,
#51694,#51695,#51696,#51697,#51698)),.UNSPECIFIED.,.F.,.F.,.F.,(4,4),(4,
1,1,1,1,1,1,1,1,1,1,1,1,1,1,1,1,1,1,1,1,1,1,1,1,1,1,1,1,1,1,1,1,1,1,1,1,
1,1,1,1,1,1,1,1,1,1,1,1,1,1,1,1,1,1,1,1,1,1,1,1,1,1,1,1,1,1,1,1,1,1,1,1,
1,1,1,1,1,1,1,1,1,1,1,1,1,1,1,1,1,1,1,1,1,1,1,1,1,1,1,1,1,1,1,1,1,1,1,1,
1,1,1,1,1,1,1,1,1,1,1,1,1,1,1,1,1,1,1,4),(0.,0.0986691610045069),(8.3098959515533,
8.80969750862556,9.30949906569782,10.3091021798423,11.3087052939868,12.3083084081313,
13.3079115222759,14.3075146364204,15.3071177505649,16.3067208647094,17.3063239788539,
18.3059270929984,19.3055302071429,20.3051333212874,21.3047364354319,22.3043395495765,
23.303942663721,24.3035457778655,25.30314889201,26.3027520061545,27.302355120299,
28.3019582344435,29.301561348588,30.3011644627325,31.3007675768771,32.3003706910216,
33.2999738051661,34.2995769193106,35.2991800334551,36.2987831475996,37.2983862617441,
38.2979893758886,39.2975924900331,40.2971956041777,41.2967987183222,42.2964018324667,
43.2960049466112,44.2956080607557,45.2952111749002,46.2948142890447,47.2944174031892,
48.2940205173337,49.2936236314783,50.2932267456228,51.2928298597673,52.2924329739118,
53.2920360880563,54.2916392022008,55.2912423163453,56.2908454304898,57.2904485446343,
58.2900516587789,59.2896547729234,60.2892578870679,61.2888610012124,62.2884641153569,
63.2880672295014,64.2876703436459,65.2872734577904,66.2868765719349,67.2864796860794,
68.286082800224,69.2856859143685,70.285289028513,71.2848921426575,72.284495256802,
73.2840983709465,74.283701485091,75.2833045992355,76.28290771338,77.2825108275245,
78.2821139416691,79.2817170558136,80.2813201699581,81.2809232841026,82.2805263982471,
83.2801295123916,84.2797326265361,85.2793357406806,86.2789388548251,87.2785419689697,
88.2781450831142,89.2777481972587,90.2773513114032,91.2769544255477,92.2765575396922,
93.2761606538367,94.2757637679812,95.2753668821258,96.2749699962703,97.2745731104148,
98.2741762245593,99.2737793387038,100.273382452848,101.272985566993,102.272588681137,
103.272191795282,104.271794909426,105.271398023571,106.271001137715,107.27060425186,
108.270207366004,109.269810480149,110.269413594293,111.269016708438,112.268619822582,
113.268222936727,114.267826050871,115.267429165016,116.26703227916,117.266635393305,
118.26623850745,119.265841621594,120.265444735739,121.265047849883,122.264650964028,
123.264254078172,124.263857192317,125.263460306461,126.263063420606,127.26266653475,
128.262269648895,129.261872763039,130.261475877184,131.261078991328,132.260682105473,
133.260285219617,133.760086776689,134.259888333762),.UNSPECIFIED.);
#581=B_SPLINE_SURFACE_WITH_KNOTS('',3,3,((#52048,#52049,#52050,#52051,#52052,
#52053,#52054,#52055,#52056,#52057,#52058,#52059,#52060,#52061,#52062,#52063,
#52064,#52065,#52066,#52067,#52068,#52069,#52070,#52071,#52072,#52073,#52074,
#52075,#52076,#52077,#52078,#52079,#52080,#52081,#52082,#52083,#52084,#52085,
#52086,#52087,#52088,#52089,#52090,#52091,#52092,#52093,#52094,#52095,#52096,
#52097,#52098,#52099,#52100,#52101,#52102,#52103,#52104,#52105,#52106,#52107,
#52108,#52109,#52110,#52111,#52112,#52113,#52114,#52115,#52116,#52117,#52118,
#52119,#52120,#52121,#52122,#52123,#52124,#52125,#52126,#52127,#52128,#52129,
#52130,#52131,#52132,#52133,#52134,#52135,#52136,#52137,#52138,#52139,#52140,
#52141,#52142,#52143,#52144,#52145,#52146,#52147,#52148,#52149,#52150,#52151,
#52152,#52153,#52154,#52155,#52156,#52157,#52158,#52159,#52160,#52161,#52162,
#52163,#52164,#52165,#52166,#52167,#52168,#52169,#52170,#52171,#52172,#52173,
#52174,#52175,#52176,#52177,#52178),(#52179,#52180,#52181,#52182,#52183,
#52184,#52185,#52186,#52187,#52188,#52189,#52190,#52191,#52192,#52193,#52194,
#52195,#52196,#52197,#52198,#52199,#52200,#52201,#52202,#52203,#52204,#52205,
#52206,#52207,#52208,#52209,#52210,#52211,#52212,#52213,#52214,#52215,#52216,
#52217,#52218,#52219,#52220,#52221,#52222,#52223,#52224,#52225,#52226,#52227,
#52228,#52229,#52230,#52231,#52232,#52233,#52234,#52235,#52236,#52237,#52238,
#52239,#52240,#52241,#52242,#52243,#52244,#52245,#52246,#52247,#52248,#52249,
#52250,#52251,#52252,#52253,#52254,#52255,#52256,#52257,#52258,#52259,#52260,
#52261,#52262,#52263,#52264,#52265,#52266,#52267,#52268,#52269,#52270,#52271,
#52272,#52273,#52274,#52275,#52276,#52277,#52278,#52279,#52280,#52281,#52282,
#52283,#52284,#52285,#52286,#52287,#52288,#52289,#52290,#52291,#52292,#52293,
#52294,#52295,#52296,#52297,#52298,#52299,#52300,#52301,#52302,#52303,#52304,
#52305,#52306,#52307,#52308,#52309),(#52310,#52311,#52312,#52313,#52314,
#52315,#52316,#52317,#52318,#52319,#52320,#52321,#52322,#52323,#52324,#52325,
#52326,#52327,#52328,#52329,#52330,#52331,#52332,#52333,#52334,#52335,#52336,
#52337,#52338,#52339,#52340,#52341,#52342,#52343,#52344,#52345,#52346,#52347,
#52348,#52349,#52350,#52351,#52352,#52353,#52354,#52355,#52356,#52357,#52358,
#52359,#52360,#52361,#52362,#52363,#52364,#52365,#52366,#52367,#52368,#52369,
#52370,#52371,#52372,#52373,#52374,#52375,#52376,#52377,#52378,#52379,#52380,
#52381,#52382,#52383,#52384,#52385,#52386,#52387,#52388,#52389,#52390,#52391,
#52392,#52393,#52394,#52395,#52396,#52397,#52398,#52399,#52400,#52401,#52402,
#52403,#52404,#52405,#52406,#52407,#52408,#52409,#52410,#52411,#52412,#52413,
#52414,#52415,#52416,#52417,#52418,#52419,#52420,#52421,#52422,#52423,#52424,
#52425,#52426,#52427,#52428,#52429,#52430,#52431,#52432,#52433,#52434,#52435,
#52436,#52437,#52438,#52439,#52440),(#52441,#52442,#52443,#52444,#52445,
#52446,#52447,#52448,#52449,#52450,#52451,#52452,#52453,#52454,#52455,#52456,
#52457,#52458,#52459,#52460,#52461,#52462,#52463,#52464,#52465,#52466,#52467,
#52468,#52469,#52470,#52471,#52472,#52473,#52474,#52475,#52476,#52477,#52478,
#52479,#52480,#52481,#52482,#52483,#52484,#52485,#52486,#52487,#52488,#52489,
#52490,#52491,#52492,#52493,#52494,#52495,#52496,#52497,#52498,#52499,#52500,
#52501,#52502,#52503,#52504,#52505,#52506,#52507,#52508,#52509,#52510,#52511,
#52512,#52513,#52514,#52515,#52516,#52517,#52518,#52519,#52520,#52521,#52522,
#52523,#52524,#52525,#52526,#52527,#52528,#52529,#52530,#52531,#52532,#52533,
#52534,#52535,#52536,#52537,#52538,#52539,#52540,#52541,#52542,#52543,#52544,
#52545,#52546,#52547,#52548,#52549,#52550,#52551,#52552,#52553,#52554,#52555,
#52556,#52557,#52558,#52559,#52560,#52561,#52562,#52563,#52564,#52565,#52566,
#52567,#52568,#52569,#52570,#52571)),.UNSPECIFIED.,.F.,.F.,.F.,(4,4),(4,
1,1,1,1,1,1,1,1,1,1,1,1,1,1,1,1,1,1,1,1,1,1,1,1,1,1,1,1,1,1,1,1,1,1,1,1,
1,1,1,1,1,1,1,1,1,1,1,1,1,1,1,1,1,1,1,1,1,1,1,1,1,1,1,1,1,1,1,1,1,1,1,1,
1,1,1,1,1,1,1,1,1,1,1,1,1,1,1,1,1,1,1,1,1,1,1,1,1,1,1,1,1,1,1,1,1,1,1,1,
1,1,1,1,1,1,1,1,1,1,1,1,1,1,1,1,1,1,1,4),(0.,0.0986691610045069),(11.6147305479242,
12.1145321049964,12.6143336620687,13.6139367762132,14.6135398903577,15.6131430045022,
16.6127461186467,17.6123492327912,18.6119523469357,19.6115554610803,20.6111585752248,
21.6107616893693,22.6103648035138,23.6099679176583,24.6095710318028,25.6091741459473,
26.6087772600918,27.6083803742363,28.6079834883808,29.6075866025254,30.6071897166699,
31.6067928308144,32.6063959449589,33.6059990591034,34.6056021732479,35.6052052873924,
36.6048084015369,37.6044115156814,38.604014629826,39.6036177439705,40.603220858115,
41.6028239722595,42.602427086404,43.6020302005485,44.601633314693,45.6012364288375,
46.600839542982,47.6004426571266,48.6000457712711,49.5996488854156,50.5992519995601,
51.5988551137046,52.5984582278491,53.5980613419936,54.5976644561381,55.5972675702826,
56.5968706844272,57.5964737985717,58.5960769127162,59.5956800268607,60.5952831410052,
61.5948862551497,62.5944893692942,63.5940924834387,64.5936955975832,65.5932987117278,
66.5929018258723,67.5925049400168,68.5921080541613,69.5917111683058,70.5913142824503,
71.5909173965948,72.5905205107393,73.5901236248838,74.5897267390284,75.5893298531729,
76.5889329673174,77.5885360814619,78.5881391956064,79.5877423097509,80.5873454238954,
81.5869485380399,82.5865516521845,83.586154766329,84.5857578804735,85.585360994618,
86.5849641087625,87.584567222907,88.5841703370515,89.583773451196,90.5833765653405,
91.582979679485,92.5825827936296,93.5821859077741,94.5817890219186,95.5813921360631,
96.5809952502076,97.5805983643521,98.5802014784966,99.5798045926411,100.579407706786,
101.57901082093,102.578613935075,103.578217049219,104.577820163364,105.577423277508,
106.577026391653,107.576629505797,108.576232619942,109.575835734086,110.575438848231,
111.575041962375,112.57464507652,113.574248190664,114.573851304809,115.573454418953,
116.573057533098,117.572660647242,118.572263761387,119.571866875531,120.571469989676,
121.57107310382,122.570676217965,123.570279332109,124.569882446254,125.569485560398,
126.569088674543,127.568691788687,128.568294902832,129.567898016976,130.567501131121,
131.567104245265,132.56670735941,133.566310473554,134.565913587699,135.565516701844,
136.565119815988,137.06492137306,137.564722930133),.UNSPECIFIED.);
#582=B_SPLINE_SURFACE_WITH_KNOTS('',3,3,((#54525,#54526,#54527,#54528,#54529,
#54530,#54531,#54532,#54533,#54534,#54535,#54536,#54537,#54538,#54539,#54540,
#54541,#54542,#54543,#54544,#54545,#54546,#54547,#54548,#54549,#54550,#54551,
#54552,#54553,#54554,#54555,#54556,#54557,#54558,#54559,#54560,#54561,#54562,
#54563,#54564,#54565,#54566,#54567,#54568,#54569,#54570,#54571,#54572,#54573,
#54574,#54575,#54576,#54577,#54578,#54579,#54580,#54581,#54582,#54583,#54584,
#54585,#54586,#54587,#54588,#54589,#54590,#54591,#54592,#54593,#54594,#54595,
#54596,#54597,#54598,#54599,#54600,#54601,#54602,#54603,#54604,#54605,#54606),
(#54607,#54608,#54609,#54610,#54611,#54612,#54613,#54614,#54615,#54616,
#54617,#54618,#54619,#54620,#54621,#54622,#54623,#54624,#54625,#54626,#54627,
#54628,#54629,#54630,#54631,#54632,#54633,#54634,#54635,#54636,#54637,#54638,
#54639,#54640,#54641,#54642,#54643,#54644,#54645,#54646,#54647,#54648,#54649,
#54650,#54651,#54652,#54653,#54654,#54655,#54656,#54657,#54658,#54659,#54660,
#54661,#54662,#54663,#54664,#54665,#54666,#54667,#54668,#54669,#54670,#54671,
#54672,#54673,#54674,#54675,#54676,#54677,#54678,#54679,#54680,#54681,#54682,
#54683,#54684,#54685,#54686,#54687,#54688),(#54689,#54690,#54691,#54692,
#54693,#54694,#54695,#54696,#54697,#54698,#54699,#54700,#54701,#54702,#54703,
#54704,#54705,#54706,#54707,#54708,#54709,#54710,#54711,#54712,#54713,#54714,
#54715,#54716,#54717,#54718,#54719,#54720,#54721,#54722,#54723,#54724,#54725,
#54726,#54727,#54728,#54729,#54730,#54731,#54732,#54733,#54734,#54735,#54736,
#54737,#54738,#54739,#54740,#54741,#54742,#54743,#54744,#54745,#54746,#54747,
#54748,#54749,#54750,#54751,#54752,#54753,#54754,#54755,#54756,#54757,#54758,
#54759,#54760,#54761,#54762,#54763,#54764,#54765,#54766,#54767,#54768,#54769,
#54770),(#54771,#54772,#54773,#54774,#54775,#54776,#54777,#54778,#54779,
#54780,#54781,#54782,#54783,#54784,#54785,#54786,#54787,#54788,#54789,#54790,
#54791,#54792,#54793,#54794,#54795,#54796,#54797,#54798,#54799,#54800,#54801,
#54802,#54803,#54804,#54805,#54806,#54807,#54808,#54809,#54810,#54811,#54812,
#54813,#54814,#54815,#54816,#54817,#54818,#54819,#54820,#54821,#54822,#54823,
#54824,#54825,#54826,#54827,#54828,#54829,#54830,#54831,#54832,#54833,#54834,
#54835,#54836,#54837,#54838,#54839,#54840,#54841,#54842,#54843,#54844,#54845,
#54846,#54847,#54848,#54849,#54850,#54851,#54852)),.UNSPECIFIED.,.F.,.F.,
 .F.,(4,4),(4,1,1,1,1,1,1,1,1,1,1,1,1,1,1,1,1,1,1,1,1,1,1,1,1,1,1,1,1,1,
1,1,1,1,1,1,1,1,1,1,1,1,1,1,1,1,1,1,1,1,1,1,1,1,1,1,1,1,1,1,1,1,1,1,1,1,
1,1,1,1,1,1,1,1,1,1,1,1,1,4),(0.,0.0526254770366343),(8.30815772716264,
9.30358800046718,10.2990182737717,11.2944485470763,12.2898788203808,13.2853090936853,
14.2807393669899,15.2761696402944,16.271599913599,17.2670301869035,18.262460460208,
19.2578907335126,20.2533210068171,21.2487512801216,22.2441815534262,23.2396118267307,
24.2350421000353,25.2304723733398,26.2259026466443,27.2213329199489,28.2167631932534,
29.212193466558,30.2076237398625,31.203054013167,32.1984842864716,33.1939145597761,
34.1893448330807,35.1847751063852,36.1802053796897,37.1756356529943,38.1710659262988,
39.1664961996033,40.1619264729079,41.1573567462124,42.152787019517,43.1482172928215,
44.143647566126,45.1390778394306,46.1345081127351,47.1299383860397,48.1253686593442,
49.1207989326487,50.1162292059533,51.1116594792578,52.1070897525623,53.1025200258669,
54.0979502991714,55.093380572476,56.0888108457805,57.084241119085,58.0796713923896,
59.0751016656941,60.0705319389987,61.0659622123032,62.0613924856077,63.0568227589123,
64.0522530322168,65.0476833055214,66.0431135788259,67.0385438521304,68.033974125435,
69.0294043987395,70.0248346720441,71.0202649453486,72.0156952186531,73.0111254919577,
74.0065557652622,75.0019860385667,75.9974163118713,76.9928465851758,77.9882768584804,
78.9837071317849,79.9791374050894,80.974567678394,81.9699979516985,82.9654282250031,
83.9608584983076,84.9562887716121,85.9517190449167,86.9471493182212),
 .UNSPECIFIED.);
#583=B_SPLINE_SURFACE_WITH_KNOTS('',3,3,((#55138,#55139,#55140,#55141,#55142,
#55143,#55144,#55145,#55146,#55147,#55148,#55149,#55150,#55151,#55152,#55153,
#55154,#55155,#55156,#55157,#55158,#55159,#55160,#55161,#55162,#55163,#55164,
#55165,#55166,#55167,#55168,#55169,#55170,#55171,#55172,#55173,#55174,#55175,
#55176,#55177,#55178,#55179,#55180,#55181,#55182,#55183,#55184,#55185,#55186,
#55187,#55188,#55189,#55190,#55191,#55192,#55193,#55194,#55195,#55196,#55197,
#55198,#55199,#55200,#55201,#55202,#55203,#55204,#55205,#55206,#55207,#55208,
#55209,#55210,#55211,#55212,#55213,#55214,#55215,#55216,#55217,#55218,#55219),
(#55220,#55221,#55222,#55223,#55224,#55225,#55226,#55227,#55228,#55229,
#55230,#55231,#55232,#55233,#55234,#55235,#55236,#55237,#55238,#55239,#55240,
#55241,#55242,#55243,#55244,#55245,#55246,#55247,#55248,#55249,#55250,#55251,
#55252,#55253,#55254,#55255,#55256,#55257,#55258,#55259,#55260,#55261,#55262,
#55263,#55264,#55265,#55266,#55267,#55268,#55269,#55270,#55271,#55272,#55273,
#55274,#55275,#55276,#55277,#55278,#55279,#55280,#55281,#55282,#55283,#55284,
#55285,#55286,#55287,#55288,#55289,#55290,#55291,#55292,#55293,#55294,#55295,
#55296,#55297,#55298,#55299,#55300,#55301),(#55302,#55303,#55304,#55305,
#55306,#55307,#55308,#55309,#55310,#55311,#55312,#55313,#55314,#55315,#55316,
#55317,#55318,#55319,#55320,#55321,#55322,#55323,#55324,#55325,#55326,#55327,
#55328,#55329,#55330,#55331,#55332,#55333,#55334,#55335,#55336,#55337,#55338,
#55339,#55340,#55341,#55342,#55343,#55344,#55345,#55346,#55347,#55348,#55349,
#55350,#55351,#55352,#55353,#55354,#55355,#55356,#55357,#55358,#55359,#55360,
#55361,#55362,#55363,#55364,#55365,#55366,#55367,#55368,#55369,#55370,#55371,
#55372,#55373,#55374,#55375,#55376,#55377,#55378,#55379,#55380,#55381,#55382,
#55383),(#55384,#55385,#55386,#55387,#55388,#55389,#55390,#55391,#55392,
#55393,#55394,#55395,#55396,#55397,#55398,#55399,#55400,#55401,#55402,#55403,
#55404,#55405,#55406,#55407,#55408,#55409,#55410,#55411,#55412,#55413,#55414,
#55415,#55416,#55417,#55418,#55419,#55420,#55421,#55422,#55423,#55424,#55425,
#55426,#55427,#55428,#55429,#55430,#55431,#55432,#55433,#55434,#55435,#55436,
#55437,#55438,#55439,#55440,#55441,#55442,#55443,#55444,#55445,#55446,#55447,
#55448,#55449,#55450,#55451,#55452,#55453,#55454,#55455,#55456,#55457,#55458,
#55459,#55460,#55461,#55462,#55463,#55464,#55465)),.UNSPECIFIED.,.F.,.F.,
 .F.,(4,4),(4,1,1,1,1,1,1,1,1,1,1,1,1,1,1,1,1,1,1,1,1,1,1,1,1,1,1,1,1,1,
1,1,1,1,1,1,1,1,1,1,1,1,1,1,1,1,1,1,1,1,1,1,1,1,1,1,1,1,1,1,1,1,1,1,1,1,
1,1,1,1,1,1,1,1,1,1,1,1,1,4),(0.,0.0526254770366344),(11.6163931973414,
12.611823470646,13.6072537439505,14.6026840172551,15.5981142905596,16.5935445638641,
17.5889748371687,18.5844051104732,19.5798353837777,20.5752656570823,21.5706959303868,
22.5661262036914,23.5615564769959,24.5569867503004,25.552417023605,26.5478472969095,
27.5432775702141,28.5387078435186,29.5341381168231,30.5295683901277,31.5249986634322,
32.5204289367368,33.5158592100413,34.5112894833458,35.5067197566504,36.5021500299549,
37.4975803032595,38.493010576564,39.4884408498685,40.4838711231731,41.4793013964776,
42.4747316697821,43.4701619430867,44.4655922163912,45.4610224896958,46.4564527630003,
47.4518830363048,48.4473133096094,49.4427435829139,50.4381738562185,51.433604129523,
52.4290344028275,53.4244646761321,54.4198949494366,55.4153252227412,56.4107554960457,
57.4061857693502,58.4016160426548,59.3970463159593,60.3924765892639,61.3879068625684,
62.3833371358729,63.3787674091775,64.374197682482,65.3696279557865,66.3650582290911,
67.3604885023956,68.3559187757002,69.3513490490047,70.3467793223092,71.3422095956138,
72.3376398689183,73.3330701422229,74.3285004155274,75.3239306888319,76.3193609621365,
77.314791235441,78.3102215087456,79.3056517820501,80.3010820553546,81.2965123286592,
82.2919426019637,83.2873728752682,84.2828031485728,85.2782334218773,86.2736636951819,
87.2690939684864,88.2645242417909,89.2599545150955,90.2553847884),
 .UNSPECIFIED.);
#584=(
BOUNDED_SURFACE()
B_SPLINE_SURFACE(2,2,((#37536,#37537,#37538),(#37539,#37540,#37541),(#37542,
#37543,#37544)),.UNSPECIFIED.,.F.,.F.,.F.)
B_SPLINE_SURFACE_WITH_KNOTS((3,3),(3,3),(-1.5707963267949,0.),(-3.14159265358979,
-1.5707963267949),.UNSPECIFIED.)
GEOMETRIC_REPRESENTATION_ITEM()
RATIONAL_B_SPLINE_SURFACE(((1.,0.707106781186549,1.),(0.707106781186545,
0.499999999999999,0.707106781186545),(1.,0.707106781186549,1.)))
REPRESENTATION_ITEM('')
SURFACE()
);
#585=(
BOUNDED_SURFACE()
B_SPLINE_SURFACE(2,2,((#37556,#37557,#37558),(#37559,#37560,#37561),(#37562,
#37563,#37564)),.UNSPECIFIED.,.F.,.F.,.F.)
B_SPLINE_SURFACE_WITH_KNOTS((3,3),(3,3),(-1.5707963267949,0.),(-1.5707963267949,
-4.44089209850058E-15),.UNSPECIFIED.)
GEOMETRIC_REPRESENTATION_ITEM()
RATIONAL_B_SPLINE_SURFACE(((1.,0.707106781186549,1.),(0.707106781186545,
0.499999999999999,0.707106781186545),(1.,0.707106781186549,1.)))
REPRESENTATION_ITEM('')
SURFACE()
);
#586=(
BOUNDED_SURFACE()
B_SPLINE_SURFACE(2,2,((#37576,#37577,#37578),(#37579,#37580,#37581),(#37582,
#37583,#37584)),.UNSPECIFIED.,.F.,.F.,.F.)
B_SPLINE_SURFACE_WITH_KNOTS((3,3),(3,3),(-1.5707963267949,0.),(4.4408920985006E-15,
1.57079632679489),.UNSPECIFIED.)
GEOMETRIC_REPRESENTATION_ITEM()
RATIONAL_B_SPLINE_SURFACE(((1.,0.70710678118655,1.),(0.707106781186545,
0.5,0.707106781186545),(1.,0.70710678118655,1.)))
REPRESENTATION_ITEM('')
SURFACE()
);
#587=(
BOUNDED_SURFACE()
B_SPLINE_SURFACE(2,2,((#37596,#37597,#37598),(#37599,#37600,#37601),(#37602,
#37603,#37604)),.UNSPECIFIED.,.F.,.F.,.F.)
B_SPLINE_SURFACE_WITH_KNOTS((3,3),(3,3),(-1.5707963267949,0.),(1.5707963267949,
3.14159265358979),.UNSPECIFIED.)
GEOMETRIC_REPRESENTATION_ITEM()
RATIONAL_B_SPLINE_SURFACE(((1.,0.707106781186549,1.),(0.707106781186545,
0.499999999999999,0.707106781186545),(1.,0.707106781186549,1.)))
REPRESENTATION_ITEM('')
SURFACE()
);
#588=(
BOUNDED_SURFACE()
B_SPLINE_SURFACE(2,2,((#37639,#37640,#37641),(#37642,#37643,#37644),(#37645,
#37646,#37647)),.UNSPECIFIED.,.F.,.F.,.F.)
B_SPLINE_SURFACE_WITH_KNOTS((3,3),(3,3),(0.,1.5707963267949),(-1.5707963267949,
-4.44089209850058E-15),.UNSPECIFIED.)
GEOMETRIC_REPRESENTATION_ITEM()
RATIONAL_B_SPLINE_SURFACE(((1.,0.707106781186549,1.),(0.707106781186545,
0.499999999999999,0.707106781186545),(1.,0.707106781186549,1.)))
REPRESENTATION_ITEM('')
SURFACE()
);
#589=(
BOUNDED_SURFACE()
B_SPLINE_SURFACE(2,2,((#37658,#37659,#37660),(#37661,#37662,#37663),(#37664,
#37665,#37666)),.UNSPECIFIED.,.F.,.F.,.F.)
B_SPLINE_SURFACE_WITH_KNOTS((3,3),(3,3),(0.,1.5707963267949),(4.4408920985006E-15,
1.57079632679489),.UNSPECIFIED.)
GEOMETRIC_REPRESENTATION_ITEM()
RATIONAL_B_SPLINE_SURFACE(((1.,0.70710678118655,1.),(0.707106781186545,
0.5,0.707106781186545),(1.,0.70710678118655,1.)))
REPRESENTATION_ITEM('')
SURFACE()
);
#590=(
BOUNDED_SURFACE()
B_SPLINE_SURFACE(2,2,((#37674,#37675,#37676),(#37677,#37678,#37679),(#37680,
#37681,#37682)),.UNSPECIFIED.,.F.,.F.,.F.)
B_SPLINE_SURFACE_WITH_KNOTS((3,3),(3,3),(0.,1.5707963267949),(1.5707963267949,
3.14159265358979),.UNSPECIFIED.)
GEOMETRIC_REPRESENTATION_ITEM()
RATIONAL_B_SPLINE_SURFACE(((1.,0.707106781186548,1.),(0.707106781186545,
0.499999999999999,0.707106781186545),(1.,0.707106781186548,1.)))
REPRESENTATION_ITEM('')
SURFACE()
);
#591=(
BOUNDED_SURFACE()
B_SPLINE_SURFACE(2,2,((#37690,#37691,#37692),(#37693,#37694,#37695),(#37696,
#37697,#37698)),.UNSPECIFIED.,.F.,.F.,.F.)
B_SPLINE_SURFACE_WITH_KNOTS((3,3),(3,3),(0.,1.5707963267949),(-3.14159265358979,
-1.5707963267949),.UNSPECIFIED.)
GEOMETRIC_REPRESENTATION_ITEM()
RATIONAL_B_SPLINE_SURFACE(((1.,0.70710678118655,1.),(0.707106781186545,
0.5,0.707106781186545),(1.,0.70710678118655,1.)))
REPRESENTATION_ITEM('')
SURFACE()
);
#592=(
BOUNDED_SURFACE()
B_SPLINE_SURFACE(2,2,((#37737,#37738,#37739),(#37740,#37741,#37742),(#37743,
#37744,#37745)),.UNSPECIFIED.,.F.,.F.,.F.)
B_SPLINE_SURFACE_WITH_KNOTS((3,3),(3,3),(0.,1.5707963267949),(-3.14159265358979,
-1.5707963267949),.UNSPECIFIED.)
GEOMETRIC_REPRESENTATION_ITEM()
RATIONAL_B_SPLINE_SURFACE(((1.,0.707106781186548,1.),(0.707106781186545,
0.499999999999999,0.707106781186545),(1.,0.707106781186548,1.)))
REPRESENTATION_ITEM('')
SURFACE()
);
#593=(
BOUNDED_SURFACE()
B_SPLINE_SURFACE(2,2,((#37757,#37758,#37759),(#37760,#37761,#37762),(#37763,
#37764,#37765)),.UNSPECIFIED.,.F.,.F.,.F.)
B_SPLINE_SURFACE_WITH_KNOTS((3,3),(3,3),(0.,1.5707963267949),(-1.5707963267949,
1.5832964389939E-15),.UNSPECIFIED.)
GEOMETRIC_REPRESENTATION_ITEM()
RATIONAL_B_SPLINE_SURFACE(((1.,0.707106781186545,1.),(0.707106781186551,
0.500000000000001,0.707106781186551),(1.,0.707106781186545,1.)))
REPRESENTATION_ITEM('')
SURFACE()
);
#594=(
BOUNDED_SURFACE()
B_SPLINE_SURFACE(2,2,((#37777,#37778,#37779),(#37780,#37781,#37782),(#37783,
#37784,#37785)),.UNSPECIFIED.,.F.,.F.,.F.)
B_SPLINE_SURFACE_WITH_KNOTS((3,3),(3,3),(0.,1.5707963267949),(-1.3322676295502E-14,
1.5707963267949),.UNSPECIFIED.)
GEOMETRIC_REPRESENTATION_ITEM()
RATIONAL_B_SPLINE_SURFACE(((1.,0.707106781186541,1.),(0.707106781186549,
0.499999999999996,0.707106781186549),(1.,0.707106781186541,1.)))
REPRESENTATION_ITEM('')
SURFACE()
);
#595=(
BOUNDED_SURFACE()
B_SPLINE_SURFACE(2,2,((#37797,#37798,#37799),(#37800,#37801,#37802),(#37803,
#37804,#37805)),.UNSPECIFIED.,.F.,.F.,.F.)
B_SPLINE_SURFACE_WITH_KNOTS((3,3),(3,3),(0.,1.5707963267949),(1.5707963267949,
3.1415926535898),.UNSPECIFIED.)
GEOMETRIC_REPRESENTATION_ITEM()
RATIONAL_B_SPLINE_SURFACE(((1.,0.707106781186546,1.),(0.707106781186545,
0.499999999999997,0.707106781186545),(1.,0.707106781186546,1.)))
REPRESENTATION_ITEM('')
SURFACE()
);
#596=(
BOUNDED_SURFACE()
B_SPLINE_SURFACE(2,2,((#37838,#37839,#37840),(#37841,#37842,#37843),(#37844,
#37845,#37846)),.UNSPECIFIED.,.F.,.F.,.F.)
B_SPLINE_SURFACE_WITH_KNOTS((3,3),(3,3),(0.,1.5707963267949),(-3.14159265358979,
-1.57079632679489),.UNSPECIFIED.)
GEOMETRIC_REPRESENTATION_ITEM()
RATIONAL_B_SPLINE_SURFACE(((1.,0.707106781186547,1.),(0.707106781186556,
0.500000000000006,0.707106781186556),(1.,0.707106781186547,1.)))
REPRESENTATION_ITEM('')
SURFACE()
);
#597=(
BOUNDED_SURFACE()
B_SPLINE_SURFACE(2,2,((#37858,#37859,#37860),(#37861,#37862,#37863),(#37864,
#37865,#37866)),.UNSPECIFIED.,.F.,.F.,.F.)
B_SPLINE_SURFACE_WITH_KNOTS((3,3),(3,3),(0.,1.5707963267949),(-1.5707963267949,
0.),.UNSPECIFIED.)
GEOMETRIC_REPRESENTATION_ITEM()
RATIONAL_B_SPLINE_SURFACE(((1.,0.707106781186548,1.),(0.707106781186545,
0.499999999999998,0.707106781186545),(1.,0.707106781186548,1.)))
REPRESENTATION_ITEM('')
SURFACE()
);
#598=(
BOUNDED_SURFACE()
B_SPLINE_SURFACE(2,2,((#37878,#37879,#37880),(#37881,#37882,#37883),(#37884,
#37885,#37886)),.UNSPECIFIED.,.F.,.F.,.F.)
B_SPLINE_SURFACE_WITH_KNOTS((3,3),(3,3),(0.,1.5707963267949),(-4.4408920985006E-15,
1.5707963267949),.UNSPECIFIED.)
GEOMETRIC_REPRESENTATION_ITEM()
RATIONAL_B_SPLINE_SURFACE(((1.,0.707106781186546,1.),(0.707106781186545,
0.499999999999997,0.707106781186545),(1.,0.707106781186546,1.)))
REPRESENTATION_ITEM('')
SURFACE()
);
#599=(
BOUNDED_SURFACE()
B_SPLINE_SURFACE(2,2,((#37898,#37899,#37900),(#37901,#37902,#37903),(#37904,
#37905,#37906)),.UNSPECIFIED.,.F.,.F.,.F.)
B_SPLINE_SURFACE_WITH_KNOTS((3,3),(3,3),(0.,1.5707963267949),(1.57079632679489,
3.14159265358981),.UNSPECIFIED.)
GEOMETRIC_REPRESENTATION_ITEM()
RATIONAL_B_SPLINE_SURFACE(((1.,0.70710678118654,1.),(0.707106781186558,
0.500000000000002,0.707106781186558),(1.,0.70710678118654,1.)))
REPRESENTATION_ITEM('')
SURFACE()
);
#600=(
BOUNDED_SURFACE()
B_SPLINE_SURFACE(2,2,((#42113,#42114,#42115),(#42116,#42117,#42118),(#42119,
#42120,#42121)),.UNSPECIFIED.,.F.,.F.,.F.)
B_SPLINE_SURFACE_WITH_KNOTS((3,3),(3,3),(-1.5707963267949,0.),(-3.14159265358979,
-1.5707963267949),.UNSPECIFIED.)
GEOMETRIC_REPRESENTATION_ITEM()
RATIONAL_B_SPLINE_SURFACE(((1.,0.707106781186548,1.),(0.707106781186538,
0.499999999999993,0.707106781186538),(1.,0.707106781186548,1.)))
REPRESENTATION_ITEM('')
SURFACE()
);
#601=(
BOUNDED_SURFACE()
B_SPLINE_SURFACE(2,2,((#42129,#42130,#42131),(#42132,#42133,#42134),(#42135,
#42136,#42137)),.UNSPECIFIED.,.F.,.F.,.F.)
B_SPLINE_SURFACE_WITH_KNOTS((3,3),(3,3),(-1.57079632679491,0.),(-1.5707963267949,
0.),.UNSPECIFIED.)
GEOMETRIC_REPRESENTATION_ITEM()
RATIONAL_B_SPLINE_SURFACE(((1.,0.707106781186546,1.),(0.707106781186548,
0.499999999999999,0.707106781186548),(1.,0.707106781186546,1.)))
REPRESENTATION_ITEM('')
SURFACE()
);
#602=(
BOUNDED_SURFACE()
B_SPLINE_SURFACE(2,2,((#42145,#42146,#42147),(#42148,#42149,#42150),(#42151,
#42152,#42153)),.UNSPECIFIED.,.F.,.F.,.F.)
B_SPLINE_SURFACE_WITH_KNOTS((3,3),(3,3),(-1.5707963267949,0.),(0.,1.5707963267949),
 .UNSPECIFIED.)
GEOMETRIC_REPRESENTATION_ITEM()
RATIONAL_B_SPLINE_SURFACE(((1.,0.707106781186548,1.),(0.707106781186538,
0.499999999999993,0.707106781186538),(1.,0.707106781186548,1.)))
REPRESENTATION_ITEM('')
SURFACE()
);
#603=(
BOUNDED_SURFACE()
B_SPLINE_SURFACE(2,2,((#42161,#42162,#42163),(#42164,#42165,#42166),(#42167,
#42168,#42169)),.UNSPECIFIED.,.F.,.F.,.F.)
B_SPLINE_SURFACE_WITH_KNOTS((3,3),(3,3),(-1.57079632679491,0.),(1.57079632679489,
3.14159265358979),.UNSPECIFIED.)
GEOMETRIC_REPRESENTATION_ITEM()
RATIONAL_B_SPLINE_SURFACE(((1.,0.707106781186546,1.),(0.707106781186548,
0.499999999999999,0.707106781186548),(1.,0.707106781186546,1.)))
REPRESENTATION_ITEM('')
SURFACE()
);
#604=(
BOUNDED_SURFACE()
B_SPLINE_SURFACE(2,2,((#55628,#55629,#55630,#55631,#55632,#55633,#55634,
#55635,#55636),(#55637,#55638,#55639,#55640,#55641,#55642,#55643,#55644,
#55645),(#55646,#55647,#55648,#55649,#55650,#55651,#55652,#55653,#55654)),
 .UNSPECIFIED.,.F.,.T.,.F.)
B_SPLINE_SURFACE_WITH_KNOTS((3,3),(3,2,2,2,3),(0.379169323323544,1.37300521707777),
(-3.14159265358979,-1.5707963267949,0.,1.5707963267949,3.14159265358979),
 .UNSPECIFIED.)
GEOMETRIC_REPRESENTATION_ITEM()
RATIONAL_B_SPLINE_SURFACE(((1.,0.707106781186548,1.,0.707106781186548,1.,
0.707106781186548,1.,0.707106781186548,1.),(0.879056006431844,0.621586463190722,
0.879056006431844,0.621586463190722,0.879056006431844,0.621586463190722,
0.879056006431844,0.621586463190722,0.879056006431844),(1.,0.707106781186548,
1.,0.707106781186548,1.,0.707106781186548,1.,0.707106781186548,1.)))
REPRESENTATION_ITEM('')
SURFACE()
);
#605=FACE_BOUND('',#8400,.T.);
#606=FACE_BOUND('',#8401,.T.);
#607=FACE_BOUND('',#8402,.T.);
#608=FACE_BOUND('',#8403,.T.);
#609=FACE_BOUND('',#8404,.T.);
#610=FACE_BOUND('',#8407,.T.);
#611=FACE_BOUND('',#8408,.T.);
#612=FACE_BOUND('',#8409,.T.);
#613=FACE_BOUND('',#8410,.T.);
#614=FACE_BOUND('',#8411,.T.);
#615=FACE_BOUND('',#8412,.T.);
#616=FACE_BOUND('',#8413,.T.);
#617=FACE_BOUND('',#8414,.T.);
#618=FACE_BOUND('',#8415,.T.);
#619=FACE_BOUND('',#8429,.T.);
#620=FACE_BOUND('',#8430,.T.);
#621=FACE_BOUND('',#8443,.T.);
#622=FACE_BOUND('',#8444,.T.);
#623=FACE_BOUND('',#8445,.T.);
#624=FACE_BOUND('',#8459,.T.);
#625=FACE_BOUND('',#8473,.T.);
#626=FACE_BOUND('',#8478,.T.);
#627=FACE_BOUND('',#8511,.T.);
#628=FACE_BOUND('',#8512,.T.);
#629=FACE_BOUND('',#8513,.T.);
#630=FACE_BOUND('',#8558,.T.);
#631=FACE_BOUND('',#8624,.T.);
#632=FACE_BOUND('',#8625,.T.);
#633=FACE_BOUND('',#8626,.T.);
#634=FACE_BOUND('',#8627,.T.);
#635=FACE_BOUND('',#8628,.T.);
#636=FACE_BOUND('',#8629,.T.);
#637=FACE_BOUND('',#8630,.T.);
#638=FACE_BOUND('',#8631,.T.);
#639=FACE_BOUND('',#8632,.T.);
#640=FACE_BOUND('',#8639,.T.);
#641=FACE_BOUND('',#8643,.T.);
#642=FACE_BOUND('',#8644,.T.);
#643=FACE_BOUND('',#8645,.T.);
#644=FACE_BOUND('',#8646,.T.);
#645=FACE_BOUND('',#8647,.T.);
#646=FACE_BOUND('',#8778,.T.);
#647=FACE_BOUND('',#8787,.T.);
#648=FACE_BOUND('',#8790,.T.);
#649=FACE_BOUND('',#8793,.T.);
#650=FACE_BOUND('',#8794,.T.);
#651=FACE_BOUND('',#8795,.T.);
#652=FACE_BOUND('',#8802,.T.);
#653=FACE_BOUND('',#8816,.T.);
#654=FACE_BOUND('',#8817,.T.);
#655=FACE_BOUND('',#8818,.T.);
#656=FACE_BOUND('',#8819,.T.);
#657=FACE_BOUND('',#8820,.T.);
#658=FACE_BOUND('',#8826,.T.);
#659=FACE_BOUND('',#8827,.T.);
#660=FACE_BOUND('',#8828,.T.);
#661=FACE_BOUND('',#8829,.T.);
#662=FACE_BOUND('',#8830,.T.);
#663=FACE_BOUND('',#8840,.T.);
#664=FACE_BOUND('',#8841,.T.);
#665=FACE_BOUND('',#8846,.T.);
#666=FACE_BOUND('',#8847,.T.);
#667=FACE_BOUND('',#8848,.T.);
#668=FACE_BOUND('',#8849,.T.);
#669=FACE_BOUND('',#8850,.T.);
#670=FACE_BOUND('',#8853,.T.);
#671=FACE_BOUND('',#8854,.T.);
#672=FACE_BOUND('',#8855,.T.);
#673=FACE_BOUND('',#8856,.T.);
#674=FACE_BOUND('',#8857,.T.);
#675=FACE_BOUND('',#8893,.T.);
#676=FACE_BOUND('',#8907,.T.);
#677=FACE_BOUND('',#8920,.T.);
#678=FACE_BOUND('',#8933,.T.);
#679=FACE_BOUND('',#8968,.T.);
#680=FACE_BOUND('',#8971,.T.);
#681=FACE_BOUND('',#9022,.T.);
#682=FACE_BOUND('',#9161,.T.);
#683=FACE_BOUND('',#9449,.T.);
#684=FACE_BOUND('',#9453,.T.);
#685=FACE_BOUND('',#9456,.T.);
#686=FACE_BOUND('',#9459,.T.);
#687=FACE_BOUND('',#9462,.T.);
#688=FACE_BOUND('',#9465,.T.);
#689=FACE_BOUND('',#9467,.T.);
#690=FACE_BOUND('',#9472,.T.);
#691=FACE_BOUND('',#9475,.T.);
#692=FACE_BOUND('',#9480,.T.);
#693=FACE_BOUND('',#9483,.T.);
#694=FACE_BOUND('',#9486,.T.);
#695=FACE_BOUND('',#9491,.T.);
#696=FACE_BOUND('',#9495,.T.);
#697=FACE_BOUND('',#9498,.T.);
#698=FACE_BOUND('',#9502,.T.);
#699=FACE_BOUND('',#9505,.T.);
#700=FACE_BOUND('',#9508,.T.);
#701=FACE_BOUND('',#9512,.T.);
#702=FACE_BOUND('',#9520,.T.);
#703=FACE_BOUND('',#9523,.T.);
#704=FACE_BOUND('',#9610,.T.);
#705=FACE_BOUND('',#9611,.T.);
#706=FACE_BOUND('',#9612,.T.);
#707=FACE_BOUND('',#9613,.T.);
#708=FACE_BOUND('',#9614,.T.);
#709=FACE_BOUND('',#9627,.T.);
#710=FACE_BOUND('',#9628,.T.);
#711=FACE_BOUND('',#9629,.T.);
#712=FACE_BOUND('',#9630,.T.);
#713=FACE_BOUND('',#9658,.T.);
#714=FACE_BOUND('',#9684,.T.);
#715=FACE_BOUND('',#9736,.T.);
#716=FACE_BOUND('',#9786,.T.);
#717=FACE_BOUND('',#9993,.T.);
#718=FACE_BOUND('',#9995,.T.);
#719=FACE_BOUND('',#9996,.T.);
#720=FACE_BOUND('',#9997,.T.);
#721=FACE_BOUND('',#9998,.T.);
#722=FACE_BOUND('',#9999,.T.);
#723=FACE_BOUND('',#10000,.T.);
#724=FACE_BOUND('',#10001,.T.);
#725=FACE_BOUND('',#10002,.T.);
#726=FACE_BOUND('',#10003,.T.);
#727=FACE_BOUND('',#10004,.T.);
#728=FACE_BOUND('',#10005,.T.);
#729=FACE_BOUND('',#10006,.T.);
#730=FACE_BOUND('',#10007,.T.);
#731=FACE_BOUND('',#10008,.T.);
#732=FACE_BOUND('',#10009,.T.);
#733=FACE_BOUND('',#10010,.T.);
#734=FACE_BOUND('',#10011,.T.);
#735=FACE_BOUND('',#10012,.T.);
#736=FACE_BOUND('',#10013,.T.);
#737=FACE_BOUND('',#10014,.T.);
#738=FACE_BOUND('',#10015,.T.);
#739=FACE_BOUND('',#10016,.T.);
#740=FACE_BOUND('',#10017,.T.);
#741=FACE_BOUND('',#10018,.T.);
#742=FACE_BOUND('',#10019,.T.);
#743=FACE_BOUND('',#10020,.T.);
#744=FACE_BOUND('',#10021,.T.);
#745=FACE_BOUND('',#10022,.T.);
#746=FACE_BOUND('',#10023,.T.);
#747=FACE_BOUND('',#10024,.T.);
#748=FACE_BOUND('',#10025,.T.);
#749=FACE_BOUND('',#10026,.T.);
#750=FACE_BOUND('',#10027,.T.);
#751=FACE_BOUND('',#10028,.T.);
#752=FACE_BOUND('',#10029,.T.);
#753=FACE_BOUND('',#10032,.T.);
#754=FACE_BOUND('',#10055,.T.);
#755=FACE_BOUND('',#10070,.T.);
#756=FACE_BOUND('',#10117,.T.);
#757=PLANE('',#27475);
#758=PLANE('',#27486);
#759=PLANE('',#27518);
#760=PLANE('',#27521);
#761=PLANE('',#27522);
#762=PLANE('',#27543);
#763=PLANE('',#27545);
#764=PLANE('',#27546);
#765=PLANE('',#27575);
#766=PLANE('',#27578);
#767=PLANE('',#27579);
#768=PLANE('',#27603);
#769=PLANE('',#27606);
#770=PLANE('',#27607);
#771=PLANE('',#27620);
#772=PLANE('',#27628);
#773=PLANE('',#27631);
#774=PLANE('',#27646);
#775=PLANE('',#27664);
#776=PLANE('',#27665);
#777=PLANE('',#27688);
#778=PLANE('',#27690);
#779=PLANE('',#27713);
#780=PLANE('',#27716);
#781=PLANE('',#27719);
#782=PLANE('',#27720);
#783=PLANE('',#27721);
#784=PLANE('',#27722);
#785=PLANE('',#27723);
#786=PLANE('',#27726);
#787=PLANE('',#27729);
#788=PLANE('',#27732);
#789=PLANE('',#27735);
#790=PLANE('',#27738);
#791=PLANE('',#27741);
#792=PLANE('',#27744);
#793=PLANE('',#27747);
#794=PLANE('',#27750);
#795=PLANE('',#27753);
#796=PLANE('',#27756);
#797=PLANE('',#27759);
#798=PLANE('',#27760);
#799=PLANE('',#27761);
#800=PLANE('',#27765);
#801=PLANE('',#27767);
#802=PLANE('',#27769);
#803=PLANE('',#27771);
#804=PLANE('',#27774);
#805=PLANE('',#27776);
#806=PLANE('',#27778);
#807=PLANE('',#27780);
#808=PLANE('',#27781);
#809=PLANE('',#27783);
#810=PLANE('',#27786);
#811=PLANE('',#27787);
#812=PLANE('',#27791);
#813=PLANE('',#27792);
#814=PLANE('',#27794);
#815=PLANE('',#27795);
#816=PLANE('',#27796);
#817=PLANE('',#27800);
#818=PLANE('',#27801);
#819=PLANE('',#27802);
#820=PLANE('',#27805);
#821=PLANE('',#27806);
#822=PLANE('',#27808);
#823=PLANE('',#27809);
#824=PLANE('',#27810);
#825=PLANE('',#27813);
#826=PLANE('',#27814);
#827=PLANE('',#27816);
#828=PLANE('',#27828);
#829=PLANE('',#27843);
#830=PLANE('',#27845);
#831=PLANE('',#27849);
#832=PLANE('',#27881);
#833=PLANE('',#27888);
#834=PLANE('',#27894);
#835=PLANE('',#27900);
#836=PLANE('',#27936);
#837=PLANE('',#27937);
#838=PLANE('',#27938);
#839=PLANE('',#27939);
#840=PLANE('',#27940);
#841=PLANE('',#27941);
#842=PLANE('',#27942);
#843=PLANE('',#27943);
#844=PLANE('',#27944);
#845=PLANE('',#27945);
#846=PLANE('',#27946);
#847=PLANE('',#27947);
#848=PLANE('',#27948);
#849=PLANE('',#27949);
#850=PLANE('',#27950);
#851=PLANE('',#27951);
#852=PLANE('',#27952);
#853=PLANE('',#27953);
#854=PLANE('',#27954);
#855=PLANE('',#27955);
#856=PLANE('',#27956);
#857=PLANE('',#27957);
#858=PLANE('',#27958);
#859=PLANE('',#27959);
#860=PLANE('',#27960);
#861=PLANE('',#27961);
#862=PLANE('',#27962);
#863=PLANE('',#27963);
#864=PLANE('',#27964);
#865=PLANE('',#27965);
#866=PLANE('',#27966);
#867=PLANE('',#27967);
#868=PLANE('',#27968);
#869=PLANE('',#27969);
#870=PLANE('',#27970);
#871=PLANE('',#27971);
#872=PLANE('',#27972);
#873=PLANE('',#27973);
#874=PLANE('',#27974);
#875=PLANE('',#27975);
#876=PLANE('',#27976);
#877=PLANE('',#27977);
#878=PLANE('',#27982);
#879=PLANE('',#27985);
#880=PLANE('',#27986);
#881=PLANE('',#27987);
#882=PLANE('',#27988);
#883=PLANE('',#27995);
#884=PLANE('',#28002);
#885=PLANE('',#28007);
#886=PLANE('',#28026);
#887=PLANE('',#28054);
#888=PLANE('',#28068);
#889=PLANE('',#28090);
#890=PLANE('',#28103);
#891=PLANE('',#28112);
#892=PLANE('',#28137);
#893=PLANE('',#28140);
#894=PLANE('',#28143);
#895=PLANE('',#28161);
#896=PLANE('',#28163);
#897=PLANE('',#28175);
#898=PLANE('',#28177);
#899=PLANE('',#28179);
#900=PLANE('',#28180);
#901=PLANE('',#28193);
#902=PLANE('',#28220);
#903=PLANE('',#28223);
#904=PLANE('',#28224);
#905=PLANE('',#28248);
#906=PLANE('',#28250);
#907=PLANE('',#28276);
#908=PLANE('',#28282);
#909=PLANE('',#28306);
#910=PLANE('',#28309);
#911=PLANE('',#28329);
#912=PLANE('',#28331);
#913=PLANE('',#28332);
#914=PLANE('',#28333);
#915=PLANE('',#28334);
#916=PLANE('',#28339);
#917=PLANE('',#28340);
#918=PLANE('',#28341);
#919=PLANE('',#28345);
#920=PLANE('',#28350);
#921=PLANE('',#28352);
#922=PLANE('',#28354);
#923=PLANE('',#28356);
#924=PLANE('',#28358);
#925=PLANE('',#28360);
#926=PLANE('',#28362);
#927=PLANE('',#28364);
#928=PLANE('',#28366);
#929=PLANE('',#28372);
#930=PLANE('',#28374);
#931=PLANE('',#28617);
#932=PLANE('',#28618);
#933=PLANE('',#28619);
#934=PLANE('',#28620);
#935=PLANE('',#28621);
#936=PLANE('',#28622);
#937=PLANE('',#28623);
#938=PLANE('',#28624);
#939=PLANE('',#28625);
#940=PLANE('',#28626);
#941=PLANE('',#28627);
#942=PLANE('',#28628);
#943=PLANE('',#28629);
#944=PLANE('',#28630);
#945=PLANE('',#28631);
#946=PLANE('',#28632);
#947=PLANE('',#28633);
#948=PLANE('',#28634);
#949=PLANE('',#28635);
#950=PLANE('',#28636);
#951=PLANE('',#28637);
#952=PLANE('',#28638);
#953=PLANE('',#28639);
#954=PLANE('',#28640);
#955=PLANE('',#28643);
#956=PLANE('',#28644);
#957=PLANE('',#28645);
#958=PLANE('',#28646);
#959=PLANE('',#28647);
#960=PLANE('',#28648);
#961=PLANE('',#28649);
#962=PLANE('',#28650);
#963=PLANE('',#28651);
#964=PLANE('',#28652);
#965=PLANE('',#28653);
#966=PLANE('',#28654);
#967=PLANE('',#28655);
#968=PLANE('',#28656);
#969=PLANE('',#28657);
#970=PLANE('',#28658);
#971=PLANE('',#28659);
#972=PLANE('',#28660);
#973=PLANE('',#28661);
#974=PLANE('',#28662);
#975=PLANE('',#28663);
#976=PLANE('',#28664);
#977=PLANE('',#28665);
#978=PLANE('',#28666);
#979=PLANE('',#28667);
#980=PLANE('',#28668);
#981=PLANE('',#28669);
#982=PLANE('',#28670);
#983=PLANE('',#28671);
#984=PLANE('',#28672);
#985=PLANE('',#28673);
#986=PLANE('',#28674);
#987=PLANE('',#28675);
#988=PLANE('',#28676);
#989=PLANE('',#28677);
#990=PLANE('',#28678);
#991=PLANE('',#28679);
#992=PLANE('',#28680);
#993=PLANE('',#28681);
#994=PLANE('',#28682);
#995=PLANE('',#28683);
#996=PLANE('',#28684);
#997=PLANE('',#28685);
#998=PLANE('',#28686);
#999=PLANE('',#28687);
#1000=PLANE('',#28688);
#1001=PLANE('',#28689);
#1002=PLANE('',#28690);
#1003=PLANE('',#28691);
#1004=PLANE('',#28692);
#1005=PLANE('',#28693);
#1006=PLANE('',#28694);
#1007=PLANE('',#28695);
#1008=PLANE('',#28696);
#1009=PLANE('',#28697);
#1010=PLANE('',#28698);
#1011=PLANE('',#28699);
#1012=PLANE('',#28700);
#1013=PLANE('',#28701);
#1014=PLANE('',#28702);
#1015=PLANE('',#28703);
#1016=PLANE('',#28704);
#1017=PLANE('',#28705);
#1018=PLANE('',#28706);
#1019=PLANE('',#28707);
#1020=PLANE('',#28708);
#1021=PLANE('',#28709);
#1022=PLANE('',#28710);
#1023=PLANE('',#28711);
#1024=PLANE('',#28712);
#1025=PLANE('',#28713);
#1026=PLANE('',#28714);
#1027=PLANE('',#28715);
#1028=PLANE('',#28716);
#1029=PLANE('',#28717);
#1030=PLANE('',#28718);
#1031=PLANE('',#28719);
#1032=PLANE('',#28720);
#1033=PLANE('',#28721);
#1034=PLANE('',#28722);
#1035=PLANE('',#28723);
#1036=PLANE('',#28724);
#1037=PLANE('',#28725);
#1038=PLANE('',#28726);
#1039=PLANE('',#28727);
#1040=PLANE('',#28728);
#1041=PLANE('',#28729);
#1042=PLANE('',#28730);
#1043=PLANE('',#28731);
#1044=PLANE('',#28732);
#1045=PLANE('',#28733);
#1046=PLANE('',#28734);
#1047=PLANE('',#28735);
#1048=PLANE('',#28736);
#1049=PLANE('',#28737);
#1050=PLANE('',#28738);
#1051=PLANE('',#28739);
#1052=PLANE('',#28740);
#1053=PLANE('',#28741);
#1054=PLANE('',#28742);
#1055=PLANE('',#28743);
#1056=PLANE('',#28744);
#1057=PLANE('',#28745);
#1058=PLANE('',#28746);
#1059=PLANE('',#28747);
#1060=PLANE('',#28748);
#1061=PLANE('',#28749);
#1062=PLANE('',#28750);
#1063=PLANE('',#28751);
#1064=PLANE('',#28752);
#1065=PLANE('',#28753);
#1066=PLANE('',#28754);
#1067=PLANE('',#28755);
#1068=PLANE('',#28756);
#1069=PLANE('',#28757);
#1070=PLANE('',#28758);
#1071=PLANE('',#28759);
#1072=PLANE('',#28760);
#1073=PLANE('',#28761);
#1074=PLANE('',#28762);
#1075=PLANE('',#28763);
#1076=PLANE('',#28764);
#1077=PLANE('',#28765);
#1078=PLANE('',#28766);
#1079=PLANE('',#28767);
#1080=PLANE('',#28768);
#1081=PLANE('',#28769);
#1082=PLANE('',#28770);
#1083=PLANE('',#28771);
#1084=PLANE('',#28772);
#1085=PLANE('',#28773);
#1086=PLANE('',#28774);
#1087=PLANE('',#28775);
#1088=PLANE('',#28776);
#1089=PLANE('',#28777);
#1090=PLANE('',#28778);
#1091=PLANE('',#28779);
#1092=PLANE('',#28780);
#1093=PLANE('',#28783);
#1094=PLANE('',#28784);
#1095=PLANE('',#28785);
#1096=PLANE('',#28786);
#1097=PLANE('',#28787);
#1098=PLANE('',#28788);
#1099=PLANE('',#28789);
#1100=PLANE('',#28790);
#1101=PLANE('',#28791);
#1102=PLANE('',#28792);
#1103=PLANE('',#28793);
#1104=PLANE('',#28794);
#1105=PLANE('',#28795);
#1106=PLANE('',#28796);
#1107=PLANE('',#28797);
#1108=PLANE('',#28798);
#1109=PLANE('',#28799);
#1110=PLANE('',#28800);
#1111=PLANE('',#28801);
#1112=PLANE('',#28802);
#1113=PLANE('',#28803);
#1114=PLANE('',#28804);
#1115=PLANE('',#28805);
#1116=PLANE('',#28806);
#1117=PLANE('',#28807);
#1118=PLANE('',#28808);
#1119=PLANE('',#28809);
#1120=PLANE('',#28810);
#1121=PLANE('',#28811);
#1122=PLANE('',#28812);
#1123=PLANE('',#28813);
#1124=PLANE('',#28814);
#1125=PLANE('',#28815);
#1126=PLANE('',#28816);
#1127=PLANE('',#28817);
#1128=PLANE('',#28818);
#1129=PLANE('',#28819);
#1130=PLANE('',#28820);
#1131=PLANE('',#28821);
#1132=PLANE('',#28822);
#1133=PLANE('',#28823);
#1134=PLANE('',#28824);
#1135=PLANE('',#28825);
#1136=PLANE('',#28826);
#1137=PLANE('',#28827);
#1138=PLANE('',#28828);
#1139=PLANE('',#28829);
#1140=PLANE('',#28830);
#1141=PLANE('',#28831);
#1142=PLANE('',#28832);
#1143=PLANE('',#28833);
#1144=PLANE('',#28834);
#1145=PLANE('',#28835);
#1146=PLANE('',#28836);
#1147=PLANE('',#28837);
#1148=PLANE('',#28838);
#1149=PLANE('',#28839);
#1150=PLANE('',#28840);
#1151=PLANE('',#28841);
#1152=PLANE('',#28842);
#1153=PLANE('',#28843);
#1154=PLANE('',#28844);
#1155=PLANE('',#28845);
#1156=PLANE('',#28846);
#1157=PLANE('',#28847);
#1158=PLANE('',#28848);
#1159=PLANE('',#28849);
#1160=PLANE('',#28850);
#1161=PLANE('',#28851);
#1162=PLANE('',#28852);
#1163=PLANE('',#28853);
#1164=PLANE('',#28854);
#1165=PLANE('',#28855);
#1166=PLANE('',#28856);
#1167=PLANE('',#28857);
#1168=PLANE('',#28858);
#1169=PLANE('',#28859);
#1170=PLANE('',#28860);
#1171=PLANE('',#28861);
#1172=PLANE('',#28862);
#1173=PLANE('',#28863);
#1174=PLANE('',#28864);
#1175=PLANE('',#28865);
#1176=PLANE('',#28866);
#1177=PLANE('',#28867);
#1178=PLANE('',#28868);
#1179=PLANE('',#28869);
#1180=PLANE('',#28870);
#1181=PLANE('',#28871);
#1182=PLANE('',#28872);
#1183=PLANE('',#28873);
#1184=PLANE('',#28874);
#1185=PLANE('',#28875);
#1186=PLANE('',#28876);
#1187=PLANE('',#28877);
#1188=PLANE('',#28878);
#1189=PLANE('',#28879);
#1190=PLANE('',#28880);
#1191=PLANE('',#28881);
#1192=PLANE('',#28882);
#1193=PLANE('',#28883);
#1194=PLANE('',#28884);
#1195=PLANE('',#28885);
#1196=PLANE('',#28886);
#1197=PLANE('',#28887);
#1198=PLANE('',#28888);
#1199=PLANE('',#28889);
#1200=PLANE('',#28890);
#1201=PLANE('',#28891);
#1202=PLANE('',#28892);
#1203=PLANE('',#28893);
#1204=PLANE('',#28894);
#1205=PLANE('',#28895);
#1206=PLANE('',#28896);
#1207=PLANE('',#28897);
#1208=PLANE('',#28898);
#1209=PLANE('',#28900);
#1210=PLANE('',#28902);
#1211=PLANE('',#28903);
#1212=PLANE('',#28904);
#1213=PLANE('',#28909);
#1214=PLANE('',#28910);
#1215=PLANE('',#28911);
#1216=PLANE('',#28913);
#1217=PLANE('',#28915);
#1218=PLANE('',#28916);
#1219=PLANE('',#28917);
#1220=PLANE('',#28918);
#1221=PLANE('',#28919);
#1222=PLANE('',#28920);
#1223=PLANE('',#28922);
#1224=PLANE('',#28923);
#1225=PLANE('',#28924);
#1226=PLANE('',#28925);
#1227=PLANE('',#28926);
#1228=PLANE('',#28927);
#1229=PLANE('',#28928);
#1230=PLANE('',#28929);
#1231=PLANE('',#28930);
#1232=PLANE('',#28931);
#1233=PLANE('',#28932);
#1234=PLANE('',#28933);
#1235=PLANE('',#28934);
#1236=PLANE('',#28935);
#1237=PLANE('',#28936);
#1238=PLANE('',#28937);
#1239=PLANE('',#28938);
#1240=PLANE('',#28939);
#1241=PLANE('',#28940);
#1242=PLANE('',#28941);
#1243=PLANE('',#28942);
#1244=PLANE('',#28943);
#1245=PLANE('',#28944);
#1246=PLANE('',#28945);
#1247=PLANE('',#28946);
#1248=PLANE('',#28947);
#1249=PLANE('',#28948);
#1250=PLANE('',#28949);
#1251=PLANE('',#28950);
#1252=PLANE('',#28951);
#1253=PLANE('',#28952);
#1254=PLANE('',#28953);
#1255=PLANE('',#28954);
#1256=PLANE('',#28955);
#1257=PLANE('',#28956);
#1258=PLANE('',#28957);
#1259=PLANE('',#28958);
#1260=PLANE('',#28959);
#1261=PLANE('',#28960);
#1262=PLANE('',#28961);
#1263=PLANE('',#28962);
#1264=PLANE('',#28963);
#1265=PLANE('',#28964);
#1266=PLANE('',#28965);
#1267=PLANE('',#28966);
#1268=PLANE('',#28967);
#1269=PLANE('',#28968);
#1270=PLANE('',#28969);
#1271=PLANE('',#28970);
#1272=PLANE('',#28971);
#1273=PLANE('',#28972);
#1274=PLANE('',#28973);
#1275=PLANE('',#28974);
#1276=PLANE('',#28975);
#1277=PLANE('',#28976);
#1278=PLANE('',#28977);
#1279=PLANE('',#28978);
#1280=PLANE('',#28979);
#1281=PLANE('',#28980);
#1282=PLANE('',#28981);
#1283=PLANE('',#28982);
#1284=PLANE('',#28983);
#1285=PLANE('',#28984);
#1286=PLANE('',#28985);
#1287=PLANE('',#28986);
#1288=PLANE('',#28987);
#1289=PLANE('',#28988);
#1290=PLANE('',#28989);
#1291=PLANE('',#28990);
#1292=PLANE('',#28991);
#1293=PLANE('',#28992);
#1294=PLANE('',#28993);
#1295=PLANE('',#28994);
#1296=PLANE('',#28995);
#1297=PLANE('',#28996);
#1298=PLANE('',#28997);
#1299=PLANE('',#28998);
#1300=PLANE('',#28999);
#1301=PLANE('',#29000);
#1302=PLANE('',#29001);
#1303=PLANE('',#29002);
#1304=PLANE('',#29003);
#1305=PLANE('',#29004);
#1306=PLANE('',#29005);
#1307=PLANE('',#29006);
#1308=PLANE('',#29007);
#1309=PLANE('',#29008);
#1310=PLANE('',#29009);
#1311=PLANE('',#29010);
#1312=PLANE('',#29011);
#1313=PLANE('',#29012);
#1314=PLANE('',#29013);
#1315=PLANE('',#29014);
#1316=PLANE('',#29015);
#1317=PLANE('',#29016);
#1318=PLANE('',#29017);
#1319=PLANE('',#29018);
#1320=PLANE('',#29019);
#1321=PLANE('',#29020);
#1322=PLANE('',#29021);
#1323=PLANE('',#29022);
#1324=PLANE('',#29023);
#1325=PLANE('',#29024);
#1326=PLANE('',#29025);
#1327=PLANE('',#29026);
#1328=PLANE('',#29027);
#1329=PLANE('',#29028);
#1330=PLANE('',#29029);
#1331=PLANE('',#29030);
#1332=PLANE('',#29031);
#1333=PLANE('',#29032);
#1334=PLANE('',#29033);
#1335=PLANE('',#29034);
#1336=PLANE('',#29035);
#1337=PLANE('',#29036);
#1338=PLANE('',#29037);
#1339=PLANE('',#29038);
#1340=PLANE('',#29039);
#1341=PLANE('',#29040);
#1342=PLANE('',#29041);
#1343=PLANE('',#29042);
#1344=PLANE('',#29043);
#1345=PLANE('',#29044);
#1346=PLANE('',#29045);
#1347=PLANE('',#29046);
#1348=PLANE('',#29047);
#1349=PLANE('',#29048);
#1350=PLANE('',#29049);
#1351=PLANE('',#29050);
#1352=PLANE('',#29051);
#1353=PLANE('',#29052);
#1354=PLANE('',#29053);
#1355=PLANE('',#29054);
#1356=PLANE('',#29055);
#1357=PLANE('',#29056);
#1358=PLANE('',#29057);
#1359=PLANE('',#29058);
#1360=PLANE('',#29059);
#1361=PLANE('',#29060);
#1362=PLANE('',#29061);
#1363=PLANE('',#29062);
#1364=PLANE('',#29063);
#1365=PLANE('',#29064);
#1366=PLANE('',#29065);
#1367=PLANE('',#29066);
#1368=PLANE('',#29067);
#1369=PLANE('',#29070);
#1370=PLANE('',#29072);
#1371=PLANE('',#29073);
#1372=PLANE('',#29074);
#1373=PLANE('',#29076);
#1374=PLANE('',#29078);
#1375=PLANE('',#29088);
#1376=PLANE('',#29092);
#1377=PLANE('',#29096);
#1378=PLANE('',#29100);
#1379=PLANE('',#29104);
#1380=PLANE('',#29110);
#1381=PLANE('',#29115);
#1382=PLANE('',#29119);
#1383=PLANE('',#29127);
#1384=PLANE('',#29131);
#1385=PLANE('',#29135);
#1386=PLANE('',#29143);
#1387=PLANE('',#29151);
#1388=PLANE('',#29156);
#1389=PLANE('',#29161);
#1390=PLANE('',#29165);
#1391=PLANE('',#29170);
#1392=PLANE('',#29176);
#1393=PLANE('',#29178);
#1394=PLANE('',#29186);
#1395=PLANE('',#29191);
#1396=PLANE('',#29195);
#1397=PLANE('',#29201);
#1398=PLANE('',#29206);
#1399=PLANE('',#29208);
#1400=PLANE('',#29210);
#1401=PLANE('',#29212);
#1402=PLANE('',#29217);
#1403=PLANE('',#29219);
#1404=PLANE('',#29222);
#1405=PLANE('',#29224);
#1406=PLANE('',#29225);
#1407=PLANE('',#29226);
#1408=PLANE('',#29228);
#1409=PLANE('',#29229);
#1410=PLANE('',#29233);
#1411=PLANE('',#29235);
#1412=PLANE('',#29236);
#1413=PLANE('',#29241);
#1414=PLANE('',#29242);
#1415=PLANE('',#29244);
#1416=PLANE('',#29246);
#1417=PLANE('',#29250);
#1418=PLANE('',#29251);
#1419=PLANE('',#29257);
#1420=PLANE('',#29258);
#1421=PLANE('',#29259);
#1422=PLANE('',#29260);
#1423=PLANE('',#29261);
#1424=PLANE('',#29262);
#1425=PLANE('',#29263);
#1426=PLANE('',#29264);
#1427=PLANE('',#29265);
#1428=PLANE('',#29266);
#1429=PLANE('',#29267);
#1430=PLANE('',#29268);
#1431=PLANE('',#29269);
#1432=PLANE('',#29270);
#1433=PLANE('',#29272);
#1434=PLANE('',#29273);
#1435=PLANE('',#29275);
#1436=PLANE('',#29276);
#1437=PLANE('',#29278);
#1438=PLANE('',#29279);
#1439=PLANE('',#29280);
#1440=PLANE('',#29281);
#1441=PLANE('',#29283);
#1442=PLANE('',#29285);
#1443=PLANE('',#29287);
#1444=PLANE('',#29288);
#1445=PLANE('',#29290);
#1446=PLANE('',#29292);
#1447=PLANE('',#29294);
#1448=PLANE('',#29296);
#1449=PLANE('',#29298);
#1450=PLANE('',#29301);
#1451=PLANE('',#29307);
#1452=PLANE('',#29311);
#1453=PLANE('',#29315);
#1454=PLANE('',#29319);
#1455=PLANE('',#29325);
#1456=PLANE('',#29328);
#1457=PLANE('',#29329);
#1458=PLANE('',#29338);
#1459=PLANE('',#29342);
#1460=PLANE('',#29346);
#1461=PLANE('',#29349);
#1462=PLANE('',#29353);
#1463=PLANE('',#29355);
#1464=PLANE('',#29360);
#1465=PLANE('',#29364);
#1466=PLANE('',#29368);
#1467=PLANE('',#29372);
#1468=PLANE('',#29377);
#1469=PLANE('',#29379);
#1470=PLANE('',#29380);
#1471=PLANE('',#29382);
#1472=PLANE('',#29384);
#1473=PLANE('',#29389);
#1474=PLANE('',#29410);
#1475=PLANE('',#29416);
#1476=PLANE('',#29417);
#1477=PLANE('',#29418);
#1478=PLANE('',#29419);
#1479=PLANE('',#29420);
#1480=PLANE('',#29421);
#1481=PLANE('',#29422);
#1482=PLANE('',#29423);
#1483=PLANE('',#29424);
#1484=PLANE('',#29425);
#1485=PLANE('',#29426);
#1486=PLANE('',#29427);
#1487=PLANE('',#29428);
#1488=PLANE('',#29429);
#1489=PLANE('',#29430);
#1490=PLANE('',#29431);
#1491=PLANE('',#29432);
#1492=PLANE('',#29433);
#1493=PLANE('',#29434);
#1494=PLANE('',#29435);
#1495=PLANE('',#29436);
#1496=PLANE('',#29444);
#1497=PLANE('',#29445);
#1498=PLANE('',#29446);
#1499=PLANE('',#29447);
#1500=PLANE('',#29448);
#1501=PLANE('',#29449);
#1502=PLANE('',#29450);
#1503=PLANE('',#29451);
#1504=PLANE('',#29452);
#1505=PLANE('',#29453);
#1506=PLANE('',#29454);
#1507=PLANE('',#29455);
#1508=PLANE('',#29456);
#1509=PLANE('',#29457);
#1510=PLANE('',#29458);
#1511=PLANE('',#29459);
#1512=PLANE('',#29460);
#1513=PLANE('',#29461);
#1514=PLANE('',#29462);
#1515=PLANE('',#29463);
#1516=PLANE('',#29464);
#1517=PLANE('',#29465);
#1518=PLANE('',#29466);
#1519=PLANE('',#29467);
#1520=PLANE('',#29468);
#1521=PLANE('',#29469);
#1522=PLANE('',#29470);
#1523=PLANE('',#29471);
#1524=PLANE('',#29472);
#1525=PLANE('',#29473);
#1526=PLANE('',#29474);
#1527=PLANE('',#29475);
#1528=PLANE('',#29476);
#1529=PLANE('',#29477);
#1530=PLANE('',#29478);
#1531=PLANE('',#29479);
#1532=PLANE('',#29480);
#1533=PLANE('',#29481);
#1534=PLANE('',#29482);
#1535=PLANE('',#29486);
#1536=PLANE('',#29487);
#1537=PLANE('',#29488);
#1538=PLANE('',#29489);
#1539=PLANE('',#29490);
#1540=PLANE('',#29491);
#1541=PLANE('',#29492);
#1542=PLANE('',#29495);
#1543=PLANE('',#29540);
#1544=PLANE('',#29547);
#1545=PLANE('',#29548);
#1546=PLANE('',#29549);
#1547=PLANE('',#29550);
#1548=PLANE('',#29552);
#1549=PLANE('',#29553);
#1550=PLANE('',#29554);
#1551=PLANE('',#29555);
#1552=PLANE('',#29556);
#1553=PLANE('',#29604);
#1554=PLANE('',#29609);
#1555=PLANE('',#29610);
#1556=PLANE('',#29612);
#1557=PLANE('',#29613);
#1558=PLANE('',#29615);
#1559=PLANE('',#29616);
#1560=PLANE('',#29618);
#1561=PLANE('',#29619);
#1562=PLANE('',#29621);
#1563=PLANE('',#29622);
#1564=PLANE('',#29624);
#1565=PLANE('',#29625);
#1566=PLANE('',#29627);
#1567=PLANE('',#29628);
#1568=PLANE('',#29630);
#1569=PLANE('',#29631);
#1570=PLANE('',#29633);
#1571=PLANE('',#29634);
#1572=PLANE('',#29636);
#1573=PLANE('',#29637);
#1574=PLANE('',#29639);
#1575=PLANE('',#29640);
#1576=PLANE('',#29642);
#1577=PLANE('',#29643);
#1578=PLANE('',#29645);
#1579=PLANE('',#29646);
#1580=PLANE('',#29648);
#1581=PLANE('',#29649);
#1582=PLANE('',#29651);
#1583=PLANE('',#29652);
#1584=PLANE('',#29654);
#1585=PLANE('',#29655);
#1586=PLANE('',#29657);
#1587=PLANE('',#29658);
#1588=PLANE('',#29660);
#1589=PLANE('',#29661);
#1590=PLANE('',#29663);
#1591=PLANE('',#29664);
#1592=PLANE('',#29666);
#1593=PLANE('',#29667);
#1594=PLANE('',#29669);
#1595=PLANE('',#29670);
#1596=PLANE('',#29672);
#1597=PLANE('',#29673);
#1598=PLANE('',#29675);
#1599=PLANE('',#29676);
#1600=PLANE('',#29678);
#1601=PLANE('',#29679);
#1602=PLANE('',#29681);
#1603=PLANE('',#29682);
#1604=PLANE('',#29684);
#1605=PLANE('',#29685);
#1606=PLANE('',#29687);
#1607=PLANE('',#29688);
#1608=PLANE('',#29690);
#1609=PLANE('',#29691);
#1610=PLANE('',#29693);
#1611=PLANE('',#29694);
#1612=PLANE('',#29696);
#1613=PLANE('',#29697);
#1614=PLANE('',#29699);
#1615=PLANE('',#29700);
#1616=PLANE('',#29702);
#1617=PLANE('',#29703);
#1618=PLANE('',#29705);
#1619=PLANE('',#29706);
#1620=PLANE('',#29708);
#1621=PLANE('',#29709);
#1622=PLANE('',#29711);
#1623=PLANE('',#29712);
#1624=PLANE('',#29715);
#1625=PLANE('',#29716);
#1626=PLANE('',#29719);
#1627=PLANE('',#29720);
#1628=PLANE('',#29722);
#1629=PLANE('',#29723);
#1630=PLANE('',#29725);
#1631=PLANE('',#29726);
#1632=PLANE('',#29728);
#1633=PLANE('',#29729);
#1634=PLANE('',#29731);
#1635=PLANE('',#29732);
#1636=PLANE('',#29734);
#1637=PLANE('',#29735);
#1638=PLANE('',#29737);
#1639=PLANE('',#29738);
#1640=PLANE('',#29740);
#1641=PLANE('',#29741);
#1642=PLANE('',#29743);
#1643=PLANE('',#29744);
#1644=PLANE('',#29746);
#1645=PLANE('',#29747);
#1646=PLANE('',#29749);
#1647=PLANE('',#29750);
#1648=PLANE('',#29752);
#1649=PLANE('',#29753);
#1650=PLANE('',#29755);
#1651=PLANE('',#29756);
#1652=PLANE('',#29758);
#1653=PLANE('',#29759);
#1654=PLANE('',#29761);
#1655=PLANE('',#29762);
#1656=PLANE('',#29764);
#1657=PLANE('',#29765);
#1658=PLANE('',#29767);
#1659=PLANE('',#29768);
#1660=PLANE('',#29770);
#1661=PLANE('',#29771);
#1662=PLANE('',#29773);
#1663=PLANE('',#29774);
#1664=PLANE('',#29776);
#1665=PLANE('',#29777);
#1666=PLANE('',#29779);
#1667=PLANE('',#29780);
#1668=PLANE('',#29782);
#1669=PLANE('',#29783);
#1670=PLANE('',#29785);
#1671=PLANE('',#29786);
#1672=PLANE('',#29788);
#1673=PLANE('',#29789);
#1674=PLANE('',#29791);
#1675=PLANE('',#29792);
#1676=PLANE('',#29794);
#1677=PLANE('',#29795);
#1678=PLANE('',#29797);
#1679=PLANE('',#29798);
#1680=PLANE('',#29800);
#1681=PLANE('',#29801);
#1682=PLANE('',#29803);
#1683=PLANE('',#29804);
#1684=PLANE('',#29806);
#1685=PLANE('',#29807);
#1686=PLANE('',#29809);
#1687=PLANE('',#29810);
#1688=PLANE('',#29812);
#1689=PLANE('',#29813);
#1690=PLANE('',#29815);
#1691=PLANE('',#29816);
#1692=PLANE('',#29818);
#1693=PLANE('',#29819);
#1694=PLANE('',#29821);
#1695=PLANE('',#29822);
#1696=PLANE('',#29824);
#1697=PLANE('',#29825);
#1698=PLANE('',#29827);
#1699=PLANE('',#29828);
#1700=PLANE('',#29829);
#1701=PLANE('',#29830);
#1702=PLANE('',#29831);
#1703=PLANE('',#29832);
#1704=PLANE('',#29833);
#1705=PLANE('',#29834);
#1706=PLANE('',#29839);
#1707=PLANE('',#29845);
#1708=PLANE('',#29847);
#1709=PLANE('',#29848);
#1710=PLANE('',#29849);
#1711=PLANE('',#29850);
#1712=PLANE('',#29851);
#1713=PLANE('',#29852);
#1714=PLANE('',#29853);
#1715=PLANE('',#29854);
#1716=PLANE('',#29855);
#1717=PLANE('',#29856);
#1718=PLANE('',#29857);
#1719=PLANE('',#29858);
#1720=PLANE('',#29859);
#1721=PLANE('',#29860);
#1722=PLANE('',#29861);
#1723=PLANE('',#29862);
#1724=PLANE('',#29863);
#1725=PLANE('',#29864);
#1726=PLANE('',#29865);
#1727=PLANE('',#29866);
#1728=PLANE('',#29867);
#1729=PLANE('',#29868);
#1730=PLANE('',#29869);
#1731=PLANE('',#29870);
#1732=PLANE('',#29871);
#1733=PLANE('',#29872);
#1734=PLANE('',#29873);
#1735=PLANE('',#29874);
#1736=PLANE('',#29875);
#1737=PLANE('',#29876);
#1738=PLANE('',#29877);
#1739=PLANE('',#29878);
#1740=PLANE('',#29879);
#1741=PLANE('',#29880);
#1742=PLANE('',#29881);
#1743=PLANE('',#29882);
#1744=PLANE('',#29884);
#1745=PLANE('',#29885);
#1746=PLANE('',#29886);
#1747=PLANE('',#29887);
#1748=PLANE('',#29921);
#1749=PLANE('',#29926);
#1750=PLANE('',#29927);
#1751=PLANE('',#29928);
#1752=PLANE('',#29929);
#1753=PLANE('',#29930);
#1754=PLANE('',#29931);
#1755=PLANE('',#29932);
#1756=PLANE('',#29933);
#1757=PLANE('',#29938);
#1758=LINE('',#37415,#4129);
#1759=LINE('',#37432,#4130);
#1760=LINE('',#37458,#4131);
#1761=LINE('',#37484,#4132);
#1762=LINE('',#37532,#4133);
#1763=LINE('',#37535,#4134);
#1764=LINE('',#37554,#4135);
#1765=LINE('',#37555,#4136);
#1766=LINE('',#37574,#4137);
#1767=LINE('',#37575,#4138);
#1768=LINE('',#37594,#4139);
#1769=LINE('',#37595,#4140);
#1770=LINE('',#37609,#4141);
#1771=LINE('',#37612,#4142);
#1772=LINE('',#37615,#4143);
#1773=LINE('',#37616,#4144);
#1774=LINE('',#37619,#4145);
#1775=LINE('',#37623,#4146);
#1776=LINE('',#37624,#4147);
#1777=LINE('',#37635,#4148);
#1778=LINE('',#37638,#4149);
#1779=LINE('',#37656,#4150);
#1780=LINE('',#37657,#4151);
#1781=LINE('',#37673,#4152);
#1782=LINE('',#37689,#4153);
#1783=LINE('',#37702,#4154);
#1784=LINE('',#37704,#4155);
#1785=LINE('',#37706,#4156);
#1786=LINE('',#37712,#4157);
#1787=LINE('',#37716,#4158);
#1788=LINE('',#37720,#4159);
#1789=LINE('',#37723,#4160);
#1790=LINE('',#37733,#4161);
#1791=LINE('',#37736,#4162);
#1792=LINE('',#37755,#4163);
#1793=LINE('',#37756,#4164);
#1794=LINE('',#37775,#4165);
#1795=LINE('',#37776,#4166);
#1796=LINE('',#37795,#4167);
#1797=LINE('',#37796,#4168);
#1798=LINE('',#37810,#4169);
#1799=LINE('',#37813,#4170);
#1800=LINE('',#37816,#4171);
#1801=LINE('',#37817,#4172);
#1802=LINE('',#37820,#4173);
#1803=LINE('',#37824,#4174);
#1804=LINE('',#37825,#4175);
#1805=LINE('',#37834,#4176);
#1806=LINE('',#37837,#4177);
#1807=LINE('',#37856,#4178);
#1808=LINE('',#37857,#4179);
#1809=LINE('',#37876,#4180);
#1810=LINE('',#37877,#4181);
#1811=LINE('',#37896,#4182);
#1812=LINE('',#37897,#4183);
#1813=LINE('',#37911,#4184);
#1814=LINE('',#37914,#4185);
#1815=LINE('',#37917,#4186);
#1816=LINE('',#37918,#4187);
#1817=LINE('',#37921,#4188);
#1818=LINE('',#37925,#4189);
#1819=LINE('',#37926,#4190);
#1820=LINE('',#37936,#4191);
#1821=LINE('',#37940,#4192);
#1822=LINE('',#37966,#4193);
#1823=LINE('',#37976,#4194);
#1824=LINE('',#37978,#4195);
#1825=LINE('',#37982,#4196);
#1826=LINE('',#37986,#4197);
#1827=LINE('',#38019,#4198);
#1828=LINE('',#38022,#4199);
#1829=LINE('',#38023,#4200);
#1830=LINE('',#38026,#4201);
#1831=LINE('',#38029,#4202);
#1832=LINE('',#38180,#4203);
#1833=LINE('',#38184,#4204);
#1834=LINE('',#38187,#4205);
#1835=LINE('',#38190,#4206);
#1836=LINE('',#38191,#4207);
#1837=LINE('',#38194,#4208);
#1838=LINE('',#38198,#4209);
#1839=LINE('',#38201,#4210);
#1840=LINE('',#38207,#4211);
#1841=LINE('',#38210,#4212);
#1842=LINE('',#38218,#4213);
#1843=LINE('',#38219,#4214);
#1844=LINE('',#38225,#4215);
#1845=LINE('',#38229,#4216);
#1846=LINE('',#38240,#4217);
#1847=LINE('',#38242,#4218);
#1848=LINE('',#38243,#4219);
#1849=LINE('',#38249,#4220);
#1850=LINE('',#38252,#4221);
#1851=LINE('',#38260,#4222);
#1852=LINE('',#38268,#4223);
#1853=LINE('',#38279,#4224);
#1854=LINE('',#38280,#4225);
#1855=LINE('',#38286,#4226);
#1856=LINE('',#38292,#4227);
#1857=LINE('',#38295,#4228);
#1858=LINE('',#38299,#4229);
#1859=LINE('',#38302,#4230);
#1860=LINE('',#38449,#4231);
#1861=LINE('',#38450,#4232);
#1862=LINE('',#38453,#4233);
#1863=LINE('',#38456,#4234);
#1864=LINE('',#38458,#4235);
#1865=LINE('',#38461,#4236);
#1866=LINE('',#38466,#4237);
#1867=LINE('',#38471,#4238);
#1868=LINE('',#38479,#4239);
#1869=LINE('',#38480,#4240);
#1870=LINE('',#38483,#4241);
#1871=LINE('',#38488,#4242);
#1872=LINE('',#38493,#4243);
#1873=LINE('',#38498,#4244);
#1874=LINE('',#38503,#4245);
#1875=LINE('',#38508,#4246);
#1876=LINE('',#38513,#4247);
#1877=LINE('',#38518,#4248);
#1878=LINE('',#38523,#4249);
#1879=LINE('',#38528,#4250);
#1880=LINE('',#38533,#4251);
#1881=LINE('',#38538,#4252);
#1882=LINE('',#38546,#4253);
#1883=LINE('',#38548,#4254);
#1884=LINE('',#38550,#4255);
#1885=LINE('',#38552,#4256);
#1886=LINE('',#38555,#4257);
#1887=LINE('',#38557,#4258);
#1888=LINE('',#38559,#4259);
#1889=LINE('',#38563,#4260);
#1890=LINE('',#38564,#4261);
#1891=LINE('',#38566,#4262);
#1892=LINE('',#38568,#4263);
#1893=LINE('',#38570,#4264);
#1894=LINE('',#38572,#4265);
#1895=LINE('',#38574,#4266);
#1896=LINE('',#38576,#4267);
#1897=LINE('',#38580,#4268);
#1898=LINE('',#38583,#4269);
#1899=LINE('',#38728,#4270);
#1900=LINE('',#38761,#4271);
#1901=LINE('',#38771,#4272);
#1902=LINE('',#38772,#4273);
#1903=LINE('',#38773,#4274);
#1904=LINE('',#38776,#4275);
#1905=LINE('',#38778,#4276);
#1906=LINE('',#38780,#4277);
#1907=LINE('',#38785,#4278);
#1908=LINE('',#38788,#4279);
#1909=LINE('',#38854,#4280);
#1910=LINE('',#38855,#4281);
#1911=LINE('',#38969,#4282);
#1912=LINE('',#38979,#4283);
#1913=LINE('',#38980,#4284);
#1914=LINE('',#38983,#4285);
#1915=LINE('',#38996,#4286);
#1916=LINE('',#38997,#4287);
#1917=LINE('',#39140,#4288);
#1918=LINE('',#39173,#4289);
#1919=LINE('',#39183,#4290);
#1920=LINE('',#39184,#4291);
#1921=LINE('',#39185,#4292);
#1922=LINE('',#39188,#4293);
#1923=LINE('',#39190,#4294);
#1924=LINE('',#39193,#4295);
#1925=LINE('',#39196,#4296);
#1926=LINE('',#39200,#4297);
#1927=LINE('',#39201,#4298);
#1928=LINE('',#39344,#4299);
#1929=LINE('',#39377,#4300);
#1930=LINE('',#39387,#4301);
#1931=LINE('',#39388,#4302);
#1932=LINE('',#39389,#4303);
#1933=LINE('',#39392,#4304);
#1934=LINE('',#39394,#4305);
#1935=LINE('',#39396,#4306);
#1936=LINE('',#39399,#4307);
#1937=LINE('',#39402,#4308);
#1938=LINE('',#39467,#4309);
#1939=LINE('',#39468,#4310);
#1940=LINE('',#39578,#4311);
#1941=LINE('',#39587,#4312);
#1942=LINE('',#39588,#4313);
#1943=LINE('',#39591,#4314);
#1944=LINE('',#39604,#4315);
#1945=LINE('',#39605,#4316);
#1946=LINE('',#39748,#4317);
#1947=LINE('',#39786,#4318);
#1948=LINE('',#39797,#4319);
#1949=LINE('',#39798,#4320);
#1950=LINE('',#39799,#4321);
#1951=LINE('',#39802,#4322);
#1952=LINE('',#39804,#4323);
#1953=LINE('',#39806,#4324);
#1954=LINE('',#39809,#4325);
#1955=LINE('',#39812,#4326);
#1956=LINE('',#39878,#4327);
#1957=LINE('',#39879,#4328);
#1958=LINE('',#39993,#4329);
#1959=LINE('',#40003,#4330);
#1960=LINE('',#40004,#4331);
#1961=LINE('',#40007,#4332);
#1962=LINE('',#40020,#4333);
#1963=LINE('',#40021,#4334);
#1964=LINE('',#40030,#4335);
#1965=LINE('',#40035,#4336);
#1966=LINE('',#40058,#4337);
#1967=LINE('',#40062,#4338);
#1968=LINE('',#40065,#4339);
#1969=LINE('',#40068,#4340);
#1970=LINE('',#40071,#4341);
#1971=LINE('',#40085,#4342);
#1972=LINE('',#40087,#4343);
#1973=LINE('',#40100,#4344);
#1974=LINE('',#40102,#4345);
#1975=LINE('',#40167,#4346);
#1976=LINE('',#40183,#4347);
#1977=LINE('',#40257,#4348);
#1978=LINE('',#40307,#4349);
#1979=LINE('',#40309,#4350);
#1980=LINE('',#40311,#4351);
#1981=LINE('',#40313,#4352);
#1982=LINE('',#40315,#4353);
#1983=LINE('',#40317,#4354);
#1984=LINE('',#40319,#4355);
#1985=LINE('',#40329,#4356);
#1986=LINE('',#40330,#4357);
#1987=LINE('',#40333,#4358);
#1988=LINE('',#40335,#4359);
#1989=LINE('',#40337,#4360);
#1990=LINE('',#40339,#4361);
#1991=LINE('',#40341,#4362);
#1992=LINE('',#40343,#4363);
#1993=LINE('',#40345,#4364);
#1994=LINE('',#40347,#4365);
#1995=LINE('',#40349,#4366);
#1996=LINE('',#40351,#4367);
#1997=LINE('',#40353,#4368);
#1998=LINE('',#40354,#4369);
#1999=LINE('',#40357,#4370);
#2000=LINE('',#40403,#4371);
#2001=LINE('',#40404,#4372);
#2002=LINE('',#40407,#4373);
#2003=LINE('',#40437,#4374);
#2004=LINE('',#40439,#4375);
#2005=LINE('',#40441,#4376);
#2006=LINE('',#40443,#4377);
#2007=LINE('',#40445,#4378);
#2008=LINE('',#40447,#4379);
#2009=LINE('',#40449,#4380);
#2010=LINE('',#40451,#4381);
#2011=LINE('',#40453,#4382);
#2012=LINE('',#40455,#4383);
#2013=LINE('',#40473,#4384);
#2014=LINE('',#40475,#4385);
#2015=LINE('',#40477,#4386);
#2016=LINE('',#40478,#4387);
#2017=LINE('',#40491,#4388);
#2018=LINE('',#40495,#4389);
#2019=LINE('',#40500,#4390);
#2020=LINE('',#40512,#4391);
#2021=LINE('',#40519,#4392);
#2022=LINE('',#40530,#4393);
#2023=LINE('',#40531,#4394);
#2024=LINE('',#40533,#4395);
#2025=LINE('',#40572,#4396);
#2026=LINE('',#40584,#4397);
#2027=LINE('',#40587,#4398);
#2028=LINE('',#40599,#4399);
#2029=LINE('',#40612,#4400);
#2030=LINE('',#40615,#4401);
#2031=LINE('',#40618,#4402);
#2032=LINE('',#40658,#4403);
#2033=LINE('',#40660,#4404);
#2034=LINE('',#40662,#4405);
#2035=LINE('',#40664,#4406);
#2036=LINE('',#40668,#4407);
#2037=LINE('',#40674,#4408);
#2038=LINE('',#40680,#4409);
#2039=LINE('',#40686,#4410);
#2040=LINE('',#40694,#4411);
#2041=LINE('',#40700,#4412);
#2042=LINE('',#40703,#4413);
#2043=LINE('',#40705,#4414);
#2044=LINE('',#40706,#4415);
#2045=LINE('',#40709,#4416);
#2046=LINE('',#40710,#4417);
#2047=LINE('',#40712,#4418);
#2048=LINE('',#40714,#4419);
#2049=LINE('',#40717,#4420);
#2050=LINE('',#40718,#4421);
#2051=LINE('',#40720,#4422);
#2052=LINE('',#40722,#4423);
#2053=LINE('',#40723,#4424);
#2054=LINE('',#40725,#4425);
#2055=LINE('',#40729,#4426);
#2056=LINE('',#40731,#4427);
#2057=LINE('',#40732,#4428);
#2058=LINE('',#40735,#4429);
#2059=LINE('',#40736,#4430);
#2060=LINE('',#40739,#4431);
#2061=LINE('',#40740,#4432);
#2062=LINE('',#40743,#4433);
#2063=LINE('',#40744,#4434);
#2064=LINE('',#40747,#4435);
#2065=LINE('',#40748,#4436);
#2066=LINE('',#40751,#4437);
#2067=LINE('',#40752,#4438);
#2068=LINE('',#40755,#4439);
#2069=LINE('',#40756,#4440);
#2070=LINE('',#40759,#4441);
#2071=LINE('',#40760,#4442);
#2072=LINE('',#40762,#4443);
#2073=LINE('',#40765,#4444);
#2074=LINE('',#40766,#4445);
#2075=LINE('',#40768,#4446);
#2076=LINE('',#40777,#4447);
#2077=LINE('',#40782,#4448);
#2078=LINE('',#40790,#4449);
#2079=LINE('',#40801,#4450);
#2080=LINE('',#40812,#4451);
#2081=LINE('',#40823,#4452);
#2082=LINE('',#40834,#4453);
#2083=LINE('',#40845,#4454);
#2084=LINE('',#40856,#4455);
#2085=LINE('',#40867,#4456);
#2086=LINE('',#40878,#4457);
#2087=LINE('',#40883,#4458);
#2088=LINE('',#40886,#4459);
#2089=LINE('',#40887,#4460);
#2090=LINE('',#40905,#4461);
#2091=LINE('',#40910,#4462);
#2092=LINE('',#40918,#4463);
#2093=LINE('',#40929,#4464);
#2094=LINE('',#40940,#4465);
#2095=LINE('',#40951,#4466);
#2096=LINE('',#40962,#4467);
#2097=LINE('',#40973,#4468);
#2098=LINE('',#40984,#4469);
#2099=LINE('',#40995,#4470);
#2100=LINE('',#41006,#4471);
#2101=LINE('',#41017,#4472);
#2102=LINE('',#41028,#4473);
#2103=LINE('',#41039,#4474);
#2104=LINE('',#41045,#4475);
#2105=LINE('',#41046,#4476);
#2106=LINE('',#41054,#4477);
#2107=LINE('',#41065,#4478);
#2108=LINE('',#41076,#4479);
#2109=LINE('',#41087,#4480);
#2110=LINE('',#41098,#4481);
#2111=LINE('',#41109,#4482);
#2112=LINE('',#41120,#4483);
#2113=LINE('',#41131,#4484);
#2114=LINE('',#41142,#4485);
#2115=LINE('',#41153,#4486);
#2116=LINE('',#41164,#4487);
#2117=LINE('',#41175,#4488);
#2118=LINE('',#41186,#4489);
#2119=LINE('',#41197,#4490);
#2120=LINE('',#41208,#4491);
#2121=LINE('',#41219,#4492);
#2122=LINE('',#41230,#4493);
#2123=LINE('',#41241,#4494);
#2124=LINE('',#41247,#4495);
#2125=LINE('',#41248,#4496);
#2126=LINE('',#41256,#4497);
#2127=LINE('',#41272,#4498);
#2128=LINE('',#41274,#4499);
#2129=LINE('',#41275,#4500);
#2130=LINE('',#41283,#4501);
#2131=LINE('',#41294,#4502);
#2132=LINE('',#41305,#4503);
#2133=LINE('',#41316,#4504);
#2134=LINE('',#41321,#4505);
#2135=LINE('',#41324,#4506);
#2136=LINE('',#41325,#4507);
#2137=LINE('',#41333,#4508);
#2138=LINE('',#41344,#4509);
#2139=LINE('',#41355,#4510);
#2140=LINE('',#41366,#4511);
#2141=LINE('',#41377,#4512);
#2142=LINE('',#41388,#4513);
#2143=LINE('',#41399,#4514);
#2144=LINE('',#41404,#4515);
#2145=LINE('',#41407,#4516);
#2146=LINE('',#41408,#4517);
#2147=LINE('',#41410,#4518);
#2148=LINE('',#41414,#4519);
#2149=LINE('',#41416,#4520);
#2150=LINE('',#41417,#4521);
#2151=LINE('',#41420,#4522);
#2152=LINE('',#41421,#4523);
#2153=LINE('',#41424,#4524);
#2154=LINE('',#41425,#4525);
#2155=LINE('',#41433,#4526);
#2156=LINE('',#41444,#4527);
#2157=LINE('',#41450,#4528);
#2158=LINE('',#41451,#4529);
#2159=LINE('',#41454,#4530);
#2160=LINE('',#41455,#4531);
#2161=LINE('',#41458,#4532);
#2162=LINE('',#41459,#4533);
#2163=LINE('',#41462,#4534);
#2164=LINE('',#41463,#4535);
#2165=LINE('',#41466,#4536);
#2166=LINE('',#41467,#4537);
#2167=LINE('',#41469,#4538);
#2168=LINE('',#41472,#4539);
#2169=LINE('',#41474,#4540);
#2170=LINE('',#41476,#4541);
#2171=LINE('',#41478,#4542);
#2172=LINE('',#41482,#4543);
#2173=LINE('',#41485,#4544);
#2174=LINE('',#41487,#4545);
#2175=LINE('',#41489,#4546);
#2176=LINE('',#41497,#4547);
#2177=LINE('',#41502,#4548);
#2178=LINE('',#41508,#4549);
#2179=LINE('',#41512,#4550);
#2180=LINE('',#41516,#4551);
#2181=LINE('',#41519,#4552);
#2182=LINE('',#41522,#4553);
#2183=LINE('',#41531,#4554);
#2184=LINE('',#41538,#4555);
#2185=LINE('',#41542,#4556);
#2186=LINE('',#41546,#4557);
#2187=LINE('',#41548,#4558);
#2188=LINE('',#41550,#4559);
#2189=LINE('',#41553,#4560);
#2190=LINE('',#41558,#4561);
#2191=LINE('',#41562,#4562);
#2192=LINE('',#41566,#4563);
#2193=LINE('',#41570,#4564);
#2194=LINE('',#41574,#4565);
#2195=LINE('',#41578,#4566);
#2196=LINE('',#41582,#4567);
#2197=LINE('',#41587,#4568);
#2198=LINE('',#41591,#4569);
#2199=LINE('',#41624,#4570);
#2200=LINE('',#41627,#4571);
#2201=LINE('',#41629,#4572);
#2202=LINE('',#41633,#4573);
#2203=LINE('',#41637,#4574);
#2204=LINE('',#41639,#4575);
#2205=LINE('',#41641,#4576);
#2206=LINE('',#41642,#4577);
#2207=LINE('',#41645,#4578);
#2208=LINE('',#41649,#4579);
#2209=LINE('',#41653,#4580);
#2210=LINE('',#41657,#4581);
#2211=LINE('',#41662,#4582);
#2212=LINE('',#41665,#4583);
#2213=LINE('',#41670,#4584);
#2214=LINE('',#41697,#4585);
#2215=LINE('',#41706,#4586);
#2216=LINE('',#41709,#4587);
#2217=LINE('',#41712,#4588);
#2218=LINE('',#41745,#4589);
#2219=LINE('',#41748,#4590);
#2220=LINE('',#41753,#4591);
#2221=LINE('',#41777,#4592);
#2222=LINE('',#41781,#4593);
#2223=LINE('',#41785,#4594);
#2224=LINE('',#41787,#4595);
#2225=LINE('',#41798,#4596);
#2226=LINE('',#41808,#4597);
#2227=LINE('',#41815,#4598);
#2228=LINE('',#41819,#4599);
#2229=LINE('',#41823,#4600);
#2230=LINE('',#41827,#4601);
#2231=LINE('',#41832,#4602);
#2232=LINE('',#41834,#4603);
#2233=LINE('',#41836,#4604);
#2234=LINE('',#41841,#4605);
#2235=LINE('',#41857,#4606);
#2236=LINE('',#41860,#4607);
#2237=LINE('',#41865,#4608);
#2238=LINE('',#41868,#4609);
#2239=LINE('',#41873,#4610);
#2240=LINE('',#41876,#4611);
#2241=LINE('',#41881,#4612);
#2242=LINE('',#41885,#4613);
#2243=LINE('',#41889,#4614);
#2244=LINE('',#41893,#4615);
#2245=LINE('',#41897,#4616);
#2246=LINE('',#41901,#4617);
#2247=LINE('',#41906,#4618);
#2248=LINE('',#41915,#4619);
#2249=LINE('',#41951,#4620);
#2250=LINE('',#41955,#4621);
#2251=LINE('',#41962,#4622);
#2252=LINE('',#42089,#4623);
#2253=LINE('',#42103,#4624);
#2254=LINE('',#42112,#4625);
#2255=LINE('',#42128,#4626);
#2256=LINE('',#42144,#4627);
#2257=LINE('',#42160,#4628);
#2258=LINE('',#42172,#4629);
#2259=LINE('',#42173,#4630);
#2260=LINE('',#42175,#4631);
#2261=LINE('',#42177,#4632);
#2262=LINE('',#42179,#4633);
#2263=LINE('',#42185,#4634);
#2264=LINE('',#42186,#4635);
#2265=LINE('',#42200,#4636);
#2266=LINE('',#42203,#4637);
#2267=LINE('',#42206,#4638);
#2268=LINE('',#42209,#4639);
#2269=LINE('',#42211,#4640);
#2270=LINE('',#42214,#4641);
#2271=LINE('',#42219,#4642);
#2272=LINE('',#42229,#4643);
#2273=LINE('',#42240,#4644);
#2274=LINE('',#42243,#4645);
#2275=LINE('',#42254,#4646);
#2276=LINE('',#42255,#4647);
#2277=LINE('',#42266,#4648);
#2278=LINE('',#42267,#4649);
#2279=LINE('',#42278,#4650);
#2280=LINE('',#42279,#4651);
#2281=LINE('',#42285,#4652);
#2282=LINE('',#42288,#4653);
#2283=LINE('',#42291,#4654);
#2284=LINE('',#42292,#4655);
#2285=LINE('',#42295,#4656);
#2286=LINE('',#42299,#4657);
#2287=LINE('',#42300,#4658);
#2288=LINE('',#42304,#4659);
#2289=LINE('',#42305,#4660);
#2290=LINE('',#42306,#4661);
#2291=LINE('',#42312,#4662);
#2292=LINE('',#42323,#4663);
#2293=LINE('',#42324,#4664);
#2294=LINE('',#42334,#4665);
#2295=LINE('',#42335,#4666);
#2296=LINE('',#42343,#4667);
#2297=LINE('',#42347,#4668);
#2298=LINE('',#42348,#4669);
#2299=LINE('',#42350,#4670);
#2300=LINE('',#42353,#4671);
#2301=LINE('',#42354,#4672);
#2302=LINE('',#42360,#4673);
#2303=LINE('',#42371,#4674);
#2304=LINE('',#42372,#4675);
#2305=LINE('',#42381,#4676);
#2306=LINE('',#42392,#4677);
#2307=LINE('',#42393,#4678);
#2308=LINE('',#42398,#4679);
#2309=LINE('',#42400,#4680);
#2310=LINE('',#42404,#4681);
#2311=LINE('',#42408,#4682);
#2312=LINE('',#42412,#4683);
#2313=LINE('',#42422,#4684);
#2314=LINE('',#42431,#4685);
#2315=LINE('',#42439,#4686);
#2316=LINE('',#42447,#4687);
#2317=LINE('',#42452,#4688);
#2318=LINE('',#42455,#4689);
#2319=LINE('',#42458,#4690);
#2320=LINE('',#42459,#4691);
#2321=LINE('',#42462,#4692);
#2322=LINE('',#42466,#4693);
#2323=LINE('',#42467,#4694);
#2324=LINE('',#42478,#4695);
#2325=LINE('',#42485,#4696);
#2326=LINE('',#42492,#4697);
#2327=LINE('',#42493,#4698);
#2328=LINE('',#42495,#4699);
#2329=LINE('',#42502,#4700);
#2330=LINE('',#42504,#4701);
#2331=LINE('',#42506,#4702);
#2332=LINE('',#42508,#4703);
#2333=LINE('',#42517,#4704);
#2334=LINE('',#42524,#4705);
#2335=LINE('',#42526,#4706);
#2336=LINE('',#42528,#4707);
#2337=LINE('',#42531,#4708);
#2338=LINE('',#42534,#4709);
#2339=LINE('',#42536,#4710);
#2340=LINE('',#42538,#4711);
#2341=LINE('',#42541,#4712);
#2342=LINE('',#42542,#4713);
#2343=LINE('',#42544,#4714);
#2344=LINE('',#42546,#4715);
#2345=LINE('',#42548,#4716);
#2346=LINE('',#42550,#4717);
#2347=LINE('',#42552,#4718);
#2348=LINE('',#42554,#4719);
#2349=LINE('',#42557,#4720);
#2350=LINE('',#42558,#4721);
#2351=LINE('',#42562,#4722);
#2352=LINE('',#42564,#4723);
#2353=LINE('',#42571,#4724);
#2354=LINE('',#42573,#4725);
#2355=LINE('',#42574,#4726);
#2356=LINE('',#42577,#4727);
#2357=LINE('',#42579,#4728);
#2358=LINE('',#42580,#4729);
#2359=LINE('',#42587,#4730);
#2360=LINE('',#42591,#4731);
#2361=LINE('',#42599,#4732);
#2362=LINE('',#42603,#4733);
#2363=LINE('',#42609,#4734);
#2364=LINE('',#42615,#4735);
#2365=LINE('',#42619,#4736);
#2366=LINE('',#42627,#4737);
#2367=LINE('',#42631,#4738);
#2368=LINE('',#42639,#4739);
#2369=LINE('',#42643,#4740);
#2370=LINE('',#42651,#4741);
#2371=LINE('',#42655,#4742);
#2372=LINE('',#42663,#4743);
#2373=LINE('',#42667,#4744);
#2374=LINE('',#42675,#4745);
#2375=LINE('',#42679,#4746);
#2376=LINE('',#42687,#4747);
#2377=LINE('',#42691,#4748);
#2378=LINE('',#42699,#4749);
#2379=LINE('',#42703,#4750);
#2380=LINE('',#42711,#4751);
#2381=LINE('',#42715,#4752);
#2382=LINE('',#42723,#4753);
#2383=LINE('',#42727,#4754);
#2384=LINE('',#42735,#4755);
#2385=LINE('',#42739,#4756);
#2386=LINE('',#42747,#4757);
#2387=LINE('',#42751,#4758);
#2388=LINE('',#42759,#4759);
#2389=LINE('',#42763,#4760);
#2390=LINE('',#42771,#4761);
#2391=LINE('',#42775,#4762);
#2392=LINE('',#42783,#4763);
#2393=LINE('',#42787,#4764);
#2394=LINE('',#42795,#4765);
#2395=LINE('',#42799,#4766);
#2396=LINE('',#42807,#4767);
#2397=LINE('',#42811,#4768);
#2398=LINE('',#42819,#4769);
#2399=LINE('',#42823,#4770);
#2400=LINE('',#42831,#4771);
#2401=LINE('',#42835,#4772);
#2402=LINE('',#42843,#4773);
#2403=LINE('',#42847,#4774);
#2404=LINE('',#42855,#4775);
#2405=LINE('',#42859,#4776);
#2406=LINE('',#42867,#4777);
#2407=LINE('',#42871,#4778);
#2408=LINE('',#42879,#4779);
#2409=LINE('',#42883,#4780);
#2410=LINE('',#42891,#4781);
#2411=LINE('',#42895,#4782);
#2412=LINE('',#42903,#4783);
#2413=LINE('',#42907,#4784);
#2414=LINE('',#42915,#4785);
#2415=LINE('',#42919,#4786);
#2416=LINE('',#42927,#4787);
#2417=LINE('',#42931,#4788);
#2418=LINE('',#42939,#4789);
#2419=LINE('',#42943,#4790);
#2420=LINE('',#42951,#4791);
#2421=LINE('',#42955,#4792);
#2422=LINE('',#42963,#4793);
#2423=LINE('',#42967,#4794);
#2424=LINE('',#42976,#4795);
#2425=LINE('',#42980,#4796);
#2426=LINE('',#42988,#4797);
#2427=LINE('',#42992,#4798);
#2428=LINE('',#43000,#4799);
#2429=LINE('',#43004,#4800);
#2430=LINE('',#43012,#4801);
#2431=LINE('',#43016,#4802);
#2432=LINE('',#43024,#4803);
#2433=LINE('',#43028,#4804);
#2434=LINE('',#43036,#4805);
#2435=LINE('',#43040,#4806);
#2436=LINE('',#43048,#4807);
#2437=LINE('',#43052,#4808);
#2438=LINE('',#43060,#4809);
#2439=LINE('',#43064,#4810);
#2440=LINE('',#43072,#4811);
#2441=LINE('',#43076,#4812);
#2442=LINE('',#43084,#4813);
#2443=LINE('',#43088,#4814);
#2444=LINE('',#43096,#4815);
#2445=LINE('',#43100,#4816);
#2446=LINE('',#43108,#4817);
#2447=LINE('',#43112,#4818);
#2448=LINE('',#43120,#4819);
#2449=LINE('',#43124,#4820);
#2450=LINE('',#43132,#4821);
#2451=LINE('',#43136,#4822);
#2452=LINE('',#43144,#4823);
#2453=LINE('',#43148,#4824);
#2454=LINE('',#43156,#4825);
#2455=LINE('',#43160,#4826);
#2456=LINE('',#43168,#4827);
#2457=LINE('',#43172,#4828);
#2458=LINE('',#43180,#4829);
#2459=LINE('',#43184,#4830);
#2460=LINE('',#43192,#4831);
#2461=LINE('',#43196,#4832);
#2462=LINE('',#43204,#4833);
#2463=LINE('',#43208,#4834);
#2464=LINE('',#43216,#4835);
#2465=LINE('',#43220,#4836);
#2466=LINE('',#43228,#4837);
#2467=LINE('',#43232,#4838);
#2468=LINE('',#43240,#4839);
#2469=LINE('',#43244,#4840);
#2470=LINE('',#43252,#4841);
#2471=LINE('',#43256,#4842);
#2472=LINE('',#43264,#4843);
#2473=LINE('',#43268,#4844);
#2474=LINE('',#43276,#4845);
#2475=LINE('',#43280,#4846);
#2476=LINE('',#43288,#4847);
#2477=LINE('',#43292,#4848);
#2478=LINE('',#43300,#4849);
#2479=LINE('',#43304,#4850);
#2480=LINE('',#43306,#4851);
#2481=LINE('',#43307,#4852);
#2482=LINE('',#43310,#4853);
#2483=LINE('',#43312,#4854);
#2484=LINE('',#43313,#4855);
#2485=LINE('',#43315,#4856);
#2486=LINE('',#43316,#4857);
#2487=LINE('',#43319,#4858);
#2488=LINE('',#43320,#4859);
#2489=LINE('',#43323,#4860);
#2490=LINE('',#43324,#4861);
#2491=LINE('',#43326,#4862);
#2492=LINE('',#43329,#4863);
#2493=LINE('',#43331,#4864);
#2494=LINE('',#43332,#4865);
#2495=LINE('',#43335,#4866);
#2496=LINE('',#43337,#4867);
#2497=LINE('',#43338,#4868);
#2498=LINE('',#43340,#4869);
#2499=LINE('',#43341,#4870);
#2500=LINE('',#43344,#4871);
#2501=LINE('',#43345,#4872);
#2502=LINE('',#43348,#4873);
#2503=LINE('',#43349,#4874);
#2504=LINE('',#43351,#4875);
#2505=LINE('',#43354,#4876);
#2506=LINE('',#43356,#4877);
#2507=LINE('',#43357,#4878);
#2508=LINE('',#43360,#4879);
#2509=LINE('',#43362,#4880);
#2510=LINE('',#43363,#4881);
#2511=LINE('',#43365,#4882);
#2512=LINE('',#43366,#4883);
#2513=LINE('',#43369,#4884);
#2514=LINE('',#43370,#4885);
#2515=LINE('',#43373,#4886);
#2516=LINE('',#43374,#4887);
#2517=LINE('',#43376,#4888);
#2518=LINE('',#43379,#4889);
#2519=LINE('',#43381,#4890);
#2520=LINE('',#43382,#4891);
#2521=LINE('',#43385,#4892);
#2522=LINE('',#43387,#4893);
#2523=LINE('',#43388,#4894);
#2524=LINE('',#43391,#4895);
#2525=LINE('',#43392,#4896);
#2526=LINE('',#43395,#4897);
#2527=LINE('',#43396,#4898);
#2528=LINE('',#43398,#4899);
#2529=LINE('',#43399,#4900);
#2530=LINE('',#43402,#4901);
#2531=LINE('',#43403,#4902);
#2532=LINE('',#43405,#4903);
#2533=LINE('',#43407,#4904);
#2534=LINE('',#43408,#4905);
#2535=LINE('',#43410,#4906);
#2536=LINE('',#43412,#4907);
#2537=LINE('',#43413,#4908);
#2538=LINE('',#43415,#4909);
#2539=LINE('',#43417,#4910);
#2540=LINE('',#43418,#4911);
#2541=LINE('',#43420,#4912);
#2542=LINE('',#43422,#4913);
#2543=LINE('',#43423,#4914);
#2544=LINE('',#43425,#4915);
#2545=LINE('',#43427,#4916);
#2546=LINE('',#43428,#4917);
#2547=LINE('',#43430,#4918);
#2548=LINE('',#43432,#4919);
#2549=LINE('',#43433,#4920);
#2550=LINE('',#43435,#4921);
#2551=LINE('',#43437,#4922);
#2552=LINE('',#43438,#4923);
#2553=LINE('',#43440,#4924);
#2554=LINE('',#43442,#4925);
#2555=LINE('',#43443,#4926);
#2556=LINE('',#43445,#4927);
#2557=LINE('',#43447,#4928);
#2558=LINE('',#43448,#4929);
#2559=LINE('',#43450,#4930);
#2560=LINE('',#43452,#4931);
#2561=LINE('',#43453,#4932);
#2562=LINE('',#43455,#4933);
#2563=LINE('',#43457,#4934);
#2564=LINE('',#43458,#4935);
#2565=LINE('',#43460,#4936);
#2566=LINE('',#43462,#4937);
#2567=LINE('',#43463,#4938);
#2568=LINE('',#43465,#4939);
#2569=LINE('',#43467,#4940);
#2570=LINE('',#43468,#4941);
#2571=LINE('',#43470,#4942);
#2572=LINE('',#43472,#4943);
#2573=LINE('',#43473,#4944);
#2574=LINE('',#43475,#4945);
#2575=LINE('',#43477,#4946);
#2576=LINE('',#43478,#4947);
#2577=LINE('',#43480,#4948);
#2578=LINE('',#43482,#4949);
#2579=LINE('',#43483,#4950);
#2580=LINE('',#43485,#4951);
#2581=LINE('',#43487,#4952);
#2582=LINE('',#43488,#4953);
#2583=LINE('',#43490,#4954);
#2584=LINE('',#43492,#4955);
#2585=LINE('',#43493,#4956);
#2586=LINE('',#43495,#4957);
#2587=LINE('',#43497,#4958);
#2588=LINE('',#43498,#4959);
#2589=LINE('',#43500,#4960);
#2590=LINE('',#43502,#4961);
#2591=LINE('',#43503,#4962);
#2592=LINE('',#43505,#4963);
#2593=LINE('',#43507,#4964);
#2594=LINE('',#43508,#4965);
#2595=LINE('',#43510,#4966);
#2596=LINE('',#43512,#4967);
#2597=LINE('',#43513,#4968);
#2598=LINE('',#43515,#4969);
#2599=LINE('',#43517,#4970);
#2600=LINE('',#43518,#4971);
#2601=LINE('',#43520,#4972);
#2602=LINE('',#43522,#4973);
#2603=LINE('',#43523,#4974);
#2604=LINE('',#43525,#4975);
#2605=LINE('',#43527,#4976);
#2606=LINE('',#43528,#4977);
#2607=LINE('',#43531,#4978);
#2608=LINE('',#43535,#4979);
#2609=LINE('',#43537,#4980);
#2610=LINE('',#43539,#4981);
#2611=LINE('',#43543,#4982);
#2612=LINE('',#43544,#4983);
#2613=LINE('',#43547,#4984);
#2614=LINE('',#43548,#4985);
#2615=LINE('',#43551,#4986);
#2616=LINE('',#43552,#4987);
#2617=LINE('',#43554,#4988);
#2618=LINE('',#43557,#4989);
#2619=LINE('',#43558,#4990);
#2620=LINE('',#43561,#4991);
#2621=LINE('',#43562,#4992);
#2622=LINE('',#43564,#4993);
#2623=LINE('',#43567,#4994);
#2624=LINE('',#43568,#4995);
#2625=LINE('',#43571,#4996);
#2626=LINE('',#43572,#4997);
#2627=LINE('',#43574,#4998);
#2628=LINE('',#43577,#4999);
#2629=LINE('',#43578,#5000);
#2630=LINE('',#43581,#5001);
#2631=LINE('',#43582,#5002);
#2632=LINE('',#43584,#5003);
#2633=LINE('',#43587,#5004);
#2634=LINE('',#43588,#5005);
#2635=LINE('',#43591,#5006);
#2636=LINE('',#43592,#5007);
#2637=LINE('',#43594,#5008);
#2638=LINE('',#43597,#5009);
#2639=LINE('',#43598,#5010);
#2640=LINE('',#43601,#5011);
#2641=LINE('',#43602,#5012);
#2642=LINE('',#43604,#5013);
#2643=LINE('',#43607,#5014);
#2644=LINE('',#43608,#5015);
#2645=LINE('',#43611,#5016);
#2646=LINE('',#43612,#5017);
#2647=LINE('',#43614,#5018);
#2648=LINE('',#43617,#5019);
#2649=LINE('',#43618,#5020);
#2650=LINE('',#43621,#5021);
#2651=LINE('',#43622,#5022);
#2652=LINE('',#43624,#5023);
#2653=LINE('',#43627,#5024);
#2654=LINE('',#43628,#5025);
#2655=LINE('',#43631,#5026);
#2656=LINE('',#43632,#5027);
#2657=LINE('',#43634,#5028);
#2658=LINE('',#43637,#5029);
#2659=LINE('',#43638,#5030);
#2660=LINE('',#43641,#5031);
#2661=LINE('',#43642,#5032);
#2662=LINE('',#43644,#5033);
#2663=LINE('',#43647,#5034);
#2664=LINE('',#43648,#5035);
#2665=LINE('',#43651,#5036);
#2666=LINE('',#43652,#5037);
#2667=LINE('',#43654,#5038);
#2668=LINE('',#43657,#5039);
#2669=LINE('',#43658,#5040);
#2670=LINE('',#43661,#5041);
#2671=LINE('',#43662,#5042);
#2672=LINE('',#43664,#5043);
#2673=LINE('',#43667,#5044);
#2674=LINE('',#43668,#5045);
#2675=LINE('',#43671,#5046);
#2676=LINE('',#43672,#5047);
#2677=LINE('',#43674,#5048);
#2678=LINE('',#43677,#5049);
#2679=LINE('',#43678,#5050);
#2680=LINE('',#43681,#5051);
#2681=LINE('',#43682,#5052);
#2682=LINE('',#43684,#5053);
#2683=LINE('',#43687,#5054);
#2684=LINE('',#43688,#5055);
#2685=LINE('',#43691,#5056);
#2686=LINE('',#43692,#5057);
#2687=LINE('',#43694,#5058);
#2688=LINE('',#43697,#5059);
#2689=LINE('',#43698,#5060);
#2690=LINE('',#43701,#5061);
#2691=LINE('',#43702,#5062);
#2692=LINE('',#43704,#5063);
#2693=LINE('',#43707,#5064);
#2694=LINE('',#43708,#5065);
#2695=LINE('',#43711,#5066);
#2696=LINE('',#43712,#5067);
#2697=LINE('',#43714,#5068);
#2698=LINE('',#43717,#5069);
#2699=LINE('',#43718,#5070);
#2700=LINE('',#43721,#5071);
#2701=LINE('',#43722,#5072);
#2702=LINE('',#43724,#5073);
#2703=LINE('',#43727,#5074);
#2704=LINE('',#43728,#5075);
#2705=LINE('',#43731,#5076);
#2706=LINE('',#43732,#5077);
#2707=LINE('',#43734,#5078);
#2708=LINE('',#43737,#5079);
#2709=LINE('',#43738,#5080);
#2710=LINE('',#43741,#5081);
#2711=LINE('',#43742,#5082);
#2712=LINE('',#43745,#5083);
#2713=LINE('',#43746,#5084);
#2714=LINE('',#43748,#5085);
#2715=LINE('',#43751,#5086);
#2716=LINE('',#43752,#5087);
#2717=LINE('',#43754,#5088);
#2718=LINE('',#43757,#5089);
#2719=LINE('',#43758,#5090);
#2720=LINE('',#43761,#5091);
#2721=LINE('',#43762,#5092);
#2722=LINE('',#43764,#5093);
#2723=LINE('',#43767,#5094);
#2724=LINE('',#43768,#5095);
#2725=LINE('',#43771,#5096);
#2726=LINE('',#43772,#5097);
#2727=LINE('',#43774,#5098);
#2728=LINE('',#43777,#5099);
#2729=LINE('',#43778,#5100);
#2730=LINE('',#43781,#5101);
#2731=LINE('',#43782,#5102);
#2732=LINE('',#43784,#5103);
#2733=LINE('',#43787,#5104);
#2734=LINE('',#43788,#5105);
#2735=LINE('',#43791,#5106);
#2736=LINE('',#43792,#5107);
#2737=LINE('',#43794,#5108);
#2738=LINE('',#43797,#5109);
#2739=LINE('',#43798,#5110);
#2740=LINE('',#43801,#5111);
#2741=LINE('',#43802,#5112);
#2742=LINE('',#43804,#5113);
#2743=LINE('',#43807,#5114);
#2744=LINE('',#43808,#5115);
#2745=LINE('',#43811,#5116);
#2746=LINE('',#43812,#5117);
#2747=LINE('',#43814,#5118);
#2748=LINE('',#43817,#5119);
#2749=LINE('',#43818,#5120);
#2750=LINE('',#43821,#5121);
#2751=LINE('',#43822,#5122);
#2752=LINE('',#43824,#5123);
#2753=LINE('',#43827,#5124);
#2754=LINE('',#43828,#5125);
#2755=LINE('',#43831,#5126);
#2756=LINE('',#43832,#5127);
#2757=LINE('',#43834,#5128);
#2758=LINE('',#43837,#5129);
#2759=LINE('',#43838,#5130);
#2760=LINE('',#43841,#5131);
#2761=LINE('',#43842,#5132);
#2762=LINE('',#43844,#5133);
#2763=LINE('',#43847,#5134);
#2764=LINE('',#43848,#5135);
#2765=LINE('',#43851,#5136);
#2766=LINE('',#43852,#5137);
#2767=LINE('',#43854,#5138);
#2768=LINE('',#43857,#5139);
#2769=LINE('',#43858,#5140);
#2770=LINE('',#43861,#5141);
#2771=LINE('',#43862,#5142);
#2772=LINE('',#43864,#5143);
#2773=LINE('',#43867,#5144);
#2774=LINE('',#43868,#5145);
#2775=LINE('',#43871,#5146);
#2776=LINE('',#43872,#5147);
#2777=LINE('',#43874,#5148);
#2778=LINE('',#43877,#5149);
#2779=LINE('',#43878,#5150);
#2780=LINE('',#43881,#5151);
#2781=LINE('',#43882,#5152);
#2782=LINE('',#43884,#5153);
#2783=LINE('',#43887,#5154);
#2784=LINE('',#43888,#5155);
#2785=LINE('',#43891,#5156);
#2786=LINE('',#43892,#5157);
#2787=LINE('',#43894,#5158);
#2788=LINE('',#43897,#5159);
#2789=LINE('',#43898,#5160);
#2790=LINE('',#43901,#5161);
#2791=LINE('',#43902,#5162);
#2792=LINE('',#43904,#5163);
#2793=LINE('',#43907,#5164);
#2794=LINE('',#43908,#5165);
#2795=LINE('',#43911,#5166);
#2796=LINE('',#43912,#5167);
#2797=LINE('',#43914,#5168);
#2798=LINE('',#43917,#5169);
#2799=LINE('',#43918,#5170);
#2800=LINE('',#43921,#5171);
#2801=LINE('',#43922,#5172);
#2802=LINE('',#43924,#5173);
#2803=LINE('',#43927,#5174);
#2804=LINE('',#43928,#5175);
#2805=LINE('',#43931,#5176);
#2806=LINE('',#43932,#5177);
#2807=LINE('',#43934,#5178);
#2808=LINE('',#43937,#5179);
#2809=LINE('',#43938,#5180);
#2810=LINE('',#43941,#5181);
#2811=LINE('',#43942,#5182);
#2812=LINE('',#43944,#5183);
#2813=LINE('',#43947,#5184);
#2814=LINE('',#43948,#5185);
#2815=LINE('',#43951,#5186);
#2816=LINE('',#43952,#5187);
#2817=LINE('',#43954,#5188);
#2818=LINE('',#43957,#5189);
#2819=LINE('',#43958,#5190);
#2820=LINE('',#43961,#5191);
#2821=LINE('',#43962,#5192);
#2822=LINE('',#43964,#5193);
#2823=LINE('',#43967,#5194);
#2824=LINE('',#43968,#5195);
#2825=LINE('',#43971,#5196);
#2826=LINE('',#43972,#5197);
#2827=LINE('',#43974,#5198);
#2828=LINE('',#43977,#5199);
#2829=LINE('',#43978,#5200);
#2830=LINE('',#43981,#5201);
#2831=LINE('',#43982,#5202);
#2832=LINE('',#43984,#5203);
#2833=LINE('',#43987,#5204);
#2834=LINE('',#43988,#5205);
#2835=LINE('',#43991,#5206);
#2836=LINE('',#43992,#5207);
#2837=LINE('',#43994,#5208);
#2838=LINE('',#43998,#5209);
#2839=LINE('',#44000,#5210);
#2840=LINE('',#44002,#5211);
#2841=LINE('',#44003,#5212);
#2842=LINE('',#44005,#5213);
#2843=LINE('',#44006,#5214);
#2844=LINE('',#44008,#5215);
#2845=LINE('',#44010,#5216);
#2846=LINE('',#44012,#5217);
#2847=LINE('',#44013,#5218);
#2848=LINE('',#44015,#5219);
#2849=LINE('',#44017,#5220);
#2850=LINE('',#44018,#5221);
#2851=LINE('',#44020,#5222);
#2852=LINE('',#44022,#5223);
#2853=LINE('',#44023,#5224);
#2854=LINE('',#44025,#5225);
#2855=LINE('',#44027,#5226);
#2856=LINE('',#44028,#5227);
#2857=LINE('',#44030,#5228);
#2858=LINE('',#44032,#5229);
#2859=LINE('',#44033,#5230);
#2860=LINE('',#44035,#5231);
#2861=LINE('',#44037,#5232);
#2862=LINE('',#44038,#5233);
#2863=LINE('',#44040,#5234);
#2864=LINE('',#44042,#5235);
#2865=LINE('',#44043,#5236);
#2866=LINE('',#44045,#5237);
#2867=LINE('',#44047,#5238);
#2868=LINE('',#44048,#5239);
#2869=LINE('',#44050,#5240);
#2870=LINE('',#44052,#5241);
#2871=LINE('',#44053,#5242);
#2872=LINE('',#44055,#5243);
#2873=LINE('',#44057,#5244);
#2874=LINE('',#44058,#5245);
#2875=LINE('',#44060,#5246);
#2876=LINE('',#44062,#5247);
#2877=LINE('',#44063,#5248);
#2878=LINE('',#44065,#5249);
#2879=LINE('',#44067,#5250);
#2880=LINE('',#44068,#5251);
#2881=LINE('',#44070,#5252);
#2882=LINE('',#44072,#5253);
#2883=LINE('',#44073,#5254);
#2884=LINE('',#44075,#5255);
#2885=LINE('',#44077,#5256);
#2886=LINE('',#44078,#5257);
#2887=LINE('',#44080,#5258);
#2888=LINE('',#44082,#5259);
#2889=LINE('',#44083,#5260);
#2890=LINE('',#44085,#5261);
#2891=LINE('',#44087,#5262);
#2892=LINE('',#44088,#5263);
#2893=LINE('',#44090,#5264);
#2894=LINE('',#44092,#5265);
#2895=LINE('',#44093,#5266);
#2896=LINE('',#44095,#5267);
#2897=LINE('',#44097,#5268);
#2898=LINE('',#44098,#5269);
#2899=LINE('',#44100,#5270);
#2900=LINE('',#44102,#5271);
#2901=LINE('',#44103,#5272);
#2902=LINE('',#44105,#5273);
#2903=LINE('',#44107,#5274);
#2904=LINE('',#44108,#5275);
#2905=LINE('',#44110,#5276);
#2906=LINE('',#44112,#5277);
#2907=LINE('',#44113,#5278);
#2908=LINE('',#44115,#5279);
#2909=LINE('',#44117,#5280);
#2910=LINE('',#44118,#5281);
#2911=LINE('',#44120,#5282);
#2912=LINE('',#44122,#5283);
#2913=LINE('',#44123,#5284);
#2914=LINE('',#44125,#5285);
#2915=LINE('',#44127,#5286);
#2916=LINE('',#44128,#5287);
#2917=LINE('',#44130,#5288);
#2918=LINE('',#44132,#5289);
#2919=LINE('',#44133,#5290);
#2920=LINE('',#44135,#5291);
#2921=LINE('',#44137,#5292);
#2922=LINE('',#44138,#5293);
#2923=LINE('',#44140,#5294);
#2924=LINE('',#44142,#5295);
#2925=LINE('',#44143,#5296);
#2926=LINE('',#44145,#5297);
#2927=LINE('',#44147,#5298);
#2928=LINE('',#44148,#5299);
#2929=LINE('',#44150,#5300);
#2930=LINE('',#44152,#5301);
#2931=LINE('',#44153,#5302);
#2932=LINE('',#44156,#5303);
#2933=LINE('',#44158,#5304);
#2934=LINE('',#44160,#5305);
#2935=LINE('',#44164,#5306);
#2936=LINE('',#44166,#5307);
#2937=LINE('',#44168,#5308);
#2938=LINE('',#44171,#5309);
#2939=LINE('',#44174,#5310);
#2940=LINE('',#44176,#5311);
#2941=LINE('',#44177,#5312);
#2942=LINE('',#44179,#5313);
#2943=LINE('',#44181,#5314);
#2944=LINE('',#44184,#5315);
#2945=LINE('',#44186,#5316);
#2946=LINE('',#44187,#5317);
#2947=LINE('',#44189,#5318);
#2948=LINE('',#44191,#5319);
#2949=LINE('',#44194,#5320);
#2950=LINE('',#44195,#5321);
#2951=LINE('',#44198,#5322);
#2952=LINE('',#44199,#5323);
#2953=LINE('',#44202,#5324);
#2954=LINE('',#44204,#5325);
#2955=LINE('',#44205,#5326);
#2956=LINE('',#44207,#5327);
#2957=LINE('',#44209,#5328);
#2958=LINE('',#44212,#5329);
#2959=LINE('',#44214,#5330);
#2960=LINE('',#44215,#5331);
#2961=LINE('',#44217,#5332);
#2962=LINE('',#44219,#5333);
#2963=LINE('',#44222,#5334);
#2964=LINE('',#44223,#5335);
#2965=LINE('',#44226,#5336);
#2966=LINE('',#44227,#5337);
#2967=LINE('',#44230,#5338);
#2968=LINE('',#44232,#5339);
#2969=LINE('',#44233,#5340);
#2970=LINE('',#44235,#5341);
#2971=LINE('',#44237,#5342);
#2972=LINE('',#44240,#5343);
#2973=LINE('',#44242,#5344);
#2974=LINE('',#44243,#5345);
#2975=LINE('',#44245,#5346);
#2976=LINE('',#44247,#5347);
#2977=LINE('',#44250,#5348);
#2978=LINE('',#44251,#5349);
#2979=LINE('',#44254,#5350);
#2980=LINE('',#44255,#5351);
#2981=LINE('',#44258,#5352);
#2982=LINE('',#44259,#5353);
#2983=LINE('',#44262,#5354);
#2984=LINE('',#44263,#5355);
#2985=LINE('',#44265,#5356);
#2986=LINE('',#44268,#5357);
#2987=LINE('',#44270,#5358);
#2988=LINE('',#44271,#5359);
#2989=LINE('',#44273,#5360);
#2990=LINE('',#44275,#5361);
#2991=LINE('',#44278,#5362);
#2992=LINE('',#44280,#5363);
#2993=LINE('',#44281,#5364);
#2994=LINE('',#44283,#5365);
#2995=LINE('',#44285,#5366);
#2996=LINE('',#44288,#5367);
#2997=LINE('',#44289,#5368);
#2998=LINE('',#44292,#5369);
#2999=LINE('',#44293,#5370);
#3000=LINE('',#44296,#5371);
#3001=LINE('',#44298,#5372);
#3002=LINE('',#44299,#5373);
#3003=LINE('',#44301,#5374);
#3004=LINE('',#44303,#5375);
#3005=LINE('',#44306,#5376);
#3006=LINE('',#44308,#5377);
#3007=LINE('',#44309,#5378);
#3008=LINE('',#44311,#5379);
#3009=LINE('',#44313,#5380);
#3010=LINE('',#44316,#5381);
#3011=LINE('',#44317,#5382);
#3012=LINE('',#44320,#5383);
#3013=LINE('',#44321,#5384);
#3014=LINE('',#44324,#5385);
#3015=LINE('',#44326,#5386);
#3016=LINE('',#44327,#5387);
#3017=LINE('',#44329,#5388);
#3018=LINE('',#44331,#5389);
#3019=LINE('',#44334,#5390);
#3020=LINE('',#44336,#5391);
#3021=LINE('',#44337,#5392);
#3022=LINE('',#44339,#5393);
#3023=LINE('',#44341,#5394);
#3024=LINE('',#44344,#5395);
#3025=LINE('',#44345,#5396);
#3026=LINE('',#44348,#5397);
#3027=LINE('',#44349,#5398);
#3028=LINE('',#44352,#5399);
#3029=LINE('',#44354,#5400);
#3030=LINE('',#44355,#5401);
#3031=LINE('',#44357,#5402);
#3032=LINE('',#44359,#5403);
#3033=LINE('',#44362,#5404);
#3034=LINE('',#44364,#5405);
#3035=LINE('',#44365,#5406);
#3036=LINE('',#44367,#5407);
#3037=LINE('',#44369,#5408);
#3038=LINE('',#44372,#5409);
#3039=LINE('',#44373,#5410);
#3040=LINE('',#44376,#5411);
#3041=LINE('',#44377,#5412);
#3042=LINE('',#44380,#5413);
#3043=LINE('',#44382,#5414);
#3044=LINE('',#44383,#5415);
#3045=LINE('',#44385,#5416);
#3046=LINE('',#44387,#5417);
#3047=LINE('',#44390,#5418);
#3048=LINE('',#44392,#5419);
#3049=LINE('',#44393,#5420);
#3050=LINE('',#44395,#5421);
#3051=LINE('',#44397,#5422);
#3052=LINE('',#44400,#5423);
#3053=LINE('',#44401,#5424);
#3054=LINE('',#44404,#5425);
#3055=LINE('',#44405,#5426);
#3056=LINE('',#44408,#5427);
#3057=LINE('',#44410,#5428);
#3058=LINE('',#44411,#5429);
#3059=LINE('',#44413,#5430);
#3060=LINE('',#44415,#5431);
#3061=LINE('',#44418,#5432);
#3062=LINE('',#44420,#5433);
#3063=LINE('',#44421,#5434);
#3064=LINE('',#44423,#5435);
#3065=LINE('',#44425,#5436);
#3066=LINE('',#44428,#5437);
#3067=LINE('',#44429,#5438);
#3068=LINE('',#44432,#5439);
#3069=LINE('',#44433,#5440);
#3070=LINE('',#44436,#5441);
#3071=LINE('',#44438,#5442);
#3072=LINE('',#44439,#5443);
#3073=LINE('',#44441,#5444);
#3074=LINE('',#44443,#5445);
#3075=LINE('',#44446,#5446);
#3076=LINE('',#44448,#5447);
#3077=LINE('',#44449,#5448);
#3078=LINE('',#44451,#5449);
#3079=LINE('',#44453,#5450);
#3080=LINE('',#44456,#5451);
#3081=LINE('',#44458,#5452);
#3082=LINE('',#44459,#5453);
#3083=LINE('',#44461,#5454);
#3084=LINE('',#44463,#5455);
#3085=LINE('',#44466,#5456);
#3086=LINE('',#44467,#5457);
#3087=LINE('',#44470,#5458);
#3088=LINE('',#44471,#5459);
#3089=LINE('',#44474,#5460);
#3090=LINE('',#44476,#5461);
#3091=LINE('',#44477,#5462);
#3092=LINE('',#44479,#5463);
#3093=LINE('',#44481,#5464);
#3094=LINE('',#44484,#5465);
#3095=LINE('',#44486,#5466);
#3096=LINE('',#44487,#5467);
#3097=LINE('',#44489,#5468);
#3098=LINE('',#44491,#5469);
#3099=LINE('',#44494,#5470);
#3100=LINE('',#44495,#5471);
#3101=LINE('',#44498,#5472);
#3102=LINE('',#44499,#5473);
#3103=LINE('',#44502,#5474);
#3104=LINE('',#44504,#5475);
#3105=LINE('',#44505,#5476);
#3106=LINE('',#44507,#5477);
#3107=LINE('',#44509,#5478);
#3108=LINE('',#44512,#5479);
#3109=LINE('',#44514,#5480);
#3110=LINE('',#44515,#5481);
#3111=LINE('',#44517,#5482);
#3112=LINE('',#44519,#5483);
#3113=LINE('',#44522,#5484);
#3114=LINE('',#44523,#5485);
#3115=LINE('',#44526,#5486);
#3116=LINE('',#44527,#5487);
#3117=LINE('',#44530,#5488);
#3118=LINE('',#44531,#5489);
#3119=LINE('',#44534,#5490);
#3120=LINE('',#44535,#5491);
#3121=LINE('',#44537,#5492);
#3122=LINE('',#44540,#5493);
#3123=LINE('',#44542,#5494);
#3124=LINE('',#44543,#5495);
#3125=LINE('',#44545,#5496);
#3126=LINE('',#44547,#5497);
#3127=LINE('',#44550,#5498);
#3128=LINE('',#44552,#5499);
#3129=LINE('',#44553,#5500);
#3130=LINE('',#44555,#5501);
#3131=LINE('',#44557,#5502);
#3132=LINE('',#44560,#5503);
#3133=LINE('',#44561,#5504);
#3134=LINE('',#44564,#5505);
#3135=LINE('',#44565,#5506);
#3136=LINE('',#44568,#5507);
#3137=LINE('',#44570,#5508);
#3138=LINE('',#44571,#5509);
#3139=LINE('',#44575,#5510);
#3140=LINE('',#44578,#5511);
#3141=LINE('',#44582,#5512);
#3142=LINE('',#44584,#5513);
#3143=LINE('',#44585,#5514);
#3144=LINE('',#44588,#5515);
#3145=LINE('',#44589,#5516);
#3146=LINE('',#44592,#5517);
#3147=LINE('',#44593,#5518);
#3148=LINE('',#44598,#5519);
#3149=LINE('',#44602,#5520);
#3150=LINE('',#44603,#5521);
#3151=LINE('',#44610,#5522);
#3152=LINE('',#44612,#5523);
#3153=LINE('',#44615,#5524);
#3154=LINE('',#44616,#5525);
#3155=LINE('',#44618,#5526);
#3156=LINE('',#44621,#5527);
#3157=LINE('',#44623,#5528);
#3158=LINE('',#44624,#5529);
#3159=LINE('',#44627,#5530);
#3160=LINE('',#44628,#5531);
#3161=LINE('',#44630,#5532);
#3162=LINE('',#44633,#5533);
#3163=LINE('',#44635,#5534);
#3164=LINE('',#44639,#5535);
#3165=LINE('',#44644,#5536);
#3166=LINE('',#44646,#5537);
#3167=LINE('',#44647,#5538);
#3168=LINE('',#44649,#5539);
#3169=LINE('',#44651,#5540);
#3170=LINE('',#44656,#5541);
#3171=LINE('',#44658,#5542);
#3172=LINE('',#44659,#5543);
#3173=LINE('',#44661,#5544);
#3174=LINE('',#44663,#5545);
#3175=LINE('',#44667,#5546);
#3176=LINE('',#44672,#5547);
#3177=LINE('',#44674,#5548);
#3178=LINE('',#44675,#5549);
#3179=LINE('',#44677,#5550);
#3180=LINE('',#44679,#5551);
#3181=LINE('',#44683,#5552);
#3182=LINE('',#44688,#5553);
#3183=LINE('',#44690,#5554);
#3184=LINE('',#44691,#5555);
#3185=LINE('',#44693,#5556);
#3186=LINE('',#44695,#5557);
#3187=LINE('',#44699,#5558);
#3188=LINE('',#44704,#5559);
#3189=LINE('',#44706,#5560);
#3190=LINE('',#44707,#5561);
#3191=LINE('',#44709,#5562);
#3192=LINE('',#44711,#5563);
#3193=LINE('',#44716,#5564);
#3194=LINE('',#44718,#5565);
#3195=LINE('',#44719,#5566);
#3196=LINE('',#44721,#5567);
#3197=LINE('',#44723,#5568);
#3198=LINE('',#44727,#5569);
#3199=LINE('',#44732,#5570);
#3200=LINE('',#44734,#5571);
#3201=LINE('',#44735,#5572);
#3202=LINE('',#44737,#5573);
#3203=LINE('',#44739,#5574);
#3204=LINE('',#44743,#5575);
#3205=LINE('',#44748,#5576);
#3206=LINE('',#44750,#5577);
#3207=LINE('',#44751,#5578);
#3208=LINE('',#44753,#5579);
#3209=LINE('',#44755,#5580);
#3210=LINE('',#44759,#5581);
#3211=LINE('',#44764,#5582);
#3212=LINE('',#44766,#5583);
#3213=LINE('',#44767,#5584);
#3214=LINE('',#44769,#5585);
#3215=LINE('',#44771,#5586);
#3216=LINE('',#44775,#5587);
#3217=LINE('',#44780,#5588);
#3218=LINE('',#44782,#5589);
#3219=LINE('',#44783,#5590);
#3220=LINE('',#44785,#5591);
#3221=LINE('',#44787,#5592);
#3222=LINE('',#44791,#5593);
#3223=LINE('',#44794,#5594);
#3224=LINE('',#44798,#5595);
#3225=LINE('',#44800,#5596);
#3226=LINE('',#44801,#5597);
#3227=LINE('',#44803,#5598);
#3228=LINE('',#44805,#5599);
#3229=LINE('',#44809,#5600);
#3230=LINE('',#44814,#5601);
#3231=LINE('',#44816,#5602);
#3232=LINE('',#44817,#5603);
#3233=LINE('',#44819,#5604);
#3234=LINE('',#44821,#5605);
#3235=LINE('',#44826,#5606);
#3236=LINE('',#44828,#5607);
#3237=LINE('',#44829,#5608);
#3238=LINE('',#44831,#5609);
#3239=LINE('',#44833,#5610);
#3240=LINE('',#44836,#5611);
#3241=LINE('',#44839,#5612);
#3242=LINE('',#44843,#5613);
#3243=LINE('',#44844,#5614);
#3244=LINE('',#44847,#5615);
#3245=LINE('',#44848,#5616);
#3246=LINE('',#44850,#5617);
#3247=LINE('',#44854,#5618);
#3248=LINE('',#44856,#5619);
#3249=LINE('',#44857,#5620);
#3250=LINE('',#44859,#5621);
#3251=LINE('',#44861,#5622);
#3252=LINE('',#44865,#5623);
#3253=LINE('',#44866,#5624);
#3254=LINE('',#44869,#5625);
#3255=LINE('',#44870,#5626);
#3256=LINE('',#44872,#5627);
#3257=LINE('',#44875,#5628);
#3258=LINE('',#44879,#5629);
#3259=LINE('',#44880,#5630);
#3260=LINE('',#44883,#5631);
#3261=LINE('',#44884,#5632);
#3262=LINE('',#44886,#5633);
#3263=LINE('',#44890,#5634);
#3264=LINE('',#44892,#5635);
#3265=LINE('',#44893,#5636);
#3266=LINE('',#44895,#5637);
#3267=LINE('',#44897,#5638);
#3268=LINE('',#44901,#5639);
#3269=LINE('',#44902,#5640);
#3270=LINE('',#44905,#5641);
#3271=LINE('',#44906,#5642);
#3272=LINE('',#44908,#5643);
#3273=LINE('',#44911,#5644);
#3274=LINE('',#44915,#5645);
#3275=LINE('',#44916,#5646);
#3276=LINE('',#44919,#5647);
#3277=LINE('',#44920,#5648);
#3278=LINE('',#44922,#5649);
#3279=LINE('',#44926,#5650);
#3280=LINE('',#44928,#5651);
#3281=LINE('',#44929,#5652);
#3282=LINE('',#44931,#5653);
#3283=LINE('',#44933,#5654);
#3284=LINE('',#44937,#5655);
#3285=LINE('',#44938,#5656);
#3286=LINE('',#44941,#5657);
#3287=LINE('',#44942,#5658);
#3288=LINE('',#44944,#5659);
#3289=LINE('',#44948,#5660);
#3290=LINE('',#44950,#5661);
#3291=LINE('',#44951,#5662);
#3292=LINE('',#44953,#5663);
#3293=LINE('',#44955,#5664);
#3294=LINE('',#44964,#5665);
#3295=LINE('',#44966,#5666);
#3296=LINE('',#44967,#5667);
#3297=LINE('',#44970,#5668);
#3298=LINE('',#44972,#5669);
#3299=LINE('',#44973,#5670);
#3300=LINE('',#44976,#5671);
#3301=LINE('',#44978,#5672);
#3302=LINE('',#44979,#5673);
#3303=LINE('',#44982,#5674);
#3304=LINE('',#45009,#5675);
#3305=LINE('',#45071,#5676);
#3306=LINE('',#45075,#5677);
#3307=LINE('',#45076,#5678);
#3308=LINE('',#45080,#5679);
#3309=LINE('',#45084,#5680);
#3310=LINE('',#45091,#5681);
#3311=LINE('',#45098,#5682);
#3312=LINE('',#45105,#5683);
#3313=LINE('',#45112,#5684);
#3314=LINE('',#45119,#5685);
#3315=LINE('',#45123,#5686);
#3316=LINE('',#45130,#5687);
#3317=LINE('',#45137,#5688);
#3318=LINE('',#45145,#5689);
#3319=LINE('',#45149,#5690);
#3320=LINE('',#45153,#5691);
#3321=LINE('',#45159,#5692);
#3322=LINE('',#45167,#5693);
#3323=LINE('',#45173,#5694);
#3324=LINE('',#45177,#5695);
#3325=LINE('',#45181,#5696);
#3326=LINE('',#45189,#5697);
#3327=LINE('',#45195,#5698);
#3328=LINE('',#45204,#5699);
#3329=LINE('',#45210,#5700);
#3330=LINE('',#45214,#5701);
#3331=LINE('',#45220,#5702);
#3332=LINE('',#45228,#5703);
#3333=LINE('',#45236,#5704);
#3334=LINE('',#45240,#5705);
#3335=LINE('',#45249,#5706);
#3336=LINE('',#45253,#5707);
#3337=LINE('',#45257,#5708);
#3338=LINE('',#45264,#5709);
#3339=LINE('',#45272,#5710);
#3340=LINE('',#45283,#5711);
#3341=LINE('',#45287,#5712);
#3342=LINE('',#45303,#5713);
#3343=LINE('',#45306,#5714);
#3344=LINE('',#45312,#5715);
#3345=LINE('',#45316,#5716);
#3346=LINE('',#45324,#5717);
#3347=LINE('',#45328,#5718);
#3348=LINE('',#45339,#5719);
#3349=LINE('',#45340,#5720);
#3350=LINE('',#45342,#5721);
#3351=LINE('',#45344,#5722);
#3352=LINE('',#45350,#5723);
#3353=LINE('',#45352,#5724);
#3354=LINE('',#45359,#5725);
#3355=LINE('',#45361,#5726);
#3356=LINE('',#45369,#5727);
#3357=LINE('',#45370,#5728);
#3358=LINE('',#45378,#5729);
#3359=LINE('',#45379,#5730);
#3360=LINE('',#45383,#5731);
#3361=LINE('',#45388,#5732);
#3362=LINE('',#45396,#5733);
#3363=LINE('',#45397,#5734);
#3364=LINE('',#45399,#5735);
#3365=LINE('',#45400,#5736);
#3366=LINE('',#45405,#5737);
#3367=LINE('',#45406,#5738);
#3368=LINE('',#45411,#5739);
#3369=LINE('',#45412,#5740);
#3370=LINE('',#45417,#5741);
#3371=LINE('',#45418,#5742);
#3372=LINE('',#45422,#5743);
#3373=LINE('',#45426,#5744);
#3374=LINE('',#45434,#5745);
#3375=LINE('',#45472,#5746);
#3376=LINE('',#45489,#5747);
#3377=LINE('',#45517,#5748);
#3378=LINE('',#45521,#5749);
#3379=LINE('',#45549,#5750);
#3380=LINE('',#45553,#5751);
#3381=LINE('',#45581,#5752);
#3382=LINE('',#45615,#5753);
#3383=LINE('',#45616,#5754);
#3384=LINE('',#45617,#5755);
#3385=LINE('',#45681,#5756);
#3386=LINE('',#45682,#5757);
#3387=LINE('',#45683,#5758);
#3388=LINE('',#45687,#5759);
#3389=LINE('',#45688,#5760);
#3390=LINE('',#45689,#5761);
#3391=LINE('',#45753,#5762);
#3392=LINE('',#45754,#5763);
#3393=LINE('',#45755,#5764);
#3394=LINE('',#45759,#5765);
#3395=LINE('',#45760,#5766);
#3396=LINE('',#45761,#5767);
#3397=LINE('',#45795,#5768);
#3398=LINE('',#45796,#5769);
#3399=LINE('',#45797,#5770);
#3400=LINE('',#45800,#5771);
#3401=LINE('',#45803,#5772);
#3402=LINE('',#45806,#5773);
#3403=LINE('',#45807,#5774);
#3404=LINE('',#45810,#5775);
#3405=LINE('',#45814,#5776);
#3406=LINE('',#45815,#5777);
#3407=LINE('',#45818,#5778);
#3408=LINE('',#45822,#5779);
#3409=LINE('',#45823,#5780);
#3410=LINE('',#45826,#5781);
#3411=LINE('',#45828,#5782);
#3412=LINE('',#45829,#5783);
#3413=LINE('',#45832,#5784);
#3414=LINE('',#45834,#5785);
#3415=LINE('',#45835,#5786);
#3416=LINE('',#45838,#5787);
#3417=LINE('',#45845,#5788);
#3418=LINE('',#45866,#5789);
#3419=LINE('',#45868,#5790);
#3420=LINE('',#45873,#5791);
#3421=LINE('',#45875,#5792);
#3422=LINE('',#45877,#5793);
#3423=LINE('',#45878,#5794);
#3424=LINE('',#45882,#5795);
#3425=LINE('',#45888,#5796);
#3426=LINE('',#45889,#5797);
#3427=LINE('',#45890,#5798);
#3428=LINE('',#45894,#5799);
#3429=LINE('',#45900,#5800);
#3430=LINE('',#45901,#5801);
#3431=LINE('',#45902,#5802);
#3432=LINE('',#45906,#5803);
#3433=LINE('',#45912,#5804);
#3434=LINE('',#45913,#5805);
#3435=LINE('',#45914,#5806);
#3436=LINE('',#45920,#5807);
#3437=LINE('',#45923,#5808);
#3438=LINE('',#45926,#5809);
#3439=LINE('',#45927,#5810);
#3440=LINE('',#45930,#5811);
#3441=LINE('',#45934,#5812);
#3442=LINE('',#45935,#5813);
#3443=LINE('',#45947,#5814);
#3444=LINE('',#45951,#5815);
#3445=LINE('',#45955,#5816);
#3446=LINE('',#45959,#5817);
#3447=LINE('',#45963,#5818);
#3448=LINE('',#45965,#5819);
#3449=LINE('',#45966,#5820);
#3450=LINE('',#45970,#5821);
#3451=LINE('',#45976,#5822);
#3452=LINE('',#45977,#5823);
#3453=LINE('',#45978,#5824);
#3454=LINE('',#45982,#5825);
#3455=LINE('',#45987,#5826);
#3456=LINE('',#45988,#5827);
#3457=LINE('',#45989,#5828);
#3458=LINE('',#45992,#5829);
#3459=LINE('',#45996,#5830);
#3460=LINE('',#45997,#5831);
#3461=LINE('',#46001,#5832);
#3462=LINE('',#46002,#5833);
#3463=LINE('',#46004,#5834);
#3464=LINE('',#46018,#5835);
#3465=LINE('',#46020,#5836);
#3466=LINE('',#46022,#5837);
#3467=LINE('',#46023,#5838);
#3468=LINE('',#46027,#5839);
#3469=LINE('',#46033,#5840);
#3470=LINE('',#46034,#5841);
#3471=LINE('',#46035,#5842);
#3472=LINE('',#46039,#5843);
#3473=LINE('',#46045,#5844);
#3474=LINE('',#46046,#5845);
#3475=LINE('',#46047,#5846);
#3476=LINE('',#46051,#5847);
#3477=LINE('',#46057,#5848);
#3478=LINE('',#46058,#5849);
#3479=LINE('',#46059,#5850);
#3480=LINE('',#46064,#5851);
#3481=LINE('',#46065,#5852);
#3482=LINE('',#46067,#5853);
#3483=LINE('',#46069,#5854);
#3484=LINE('',#46071,#5855);
#3485=LINE('',#46074,#5856);
#3486=LINE('',#46076,#5857);
#3487=LINE('',#46078,#5858);
#3488=LINE('',#46081,#5859);
#3489=LINE('',#46083,#5860);
#3490=LINE('',#46085,#5861);
#3491=LINE('',#46087,#5862);
#3492=LINE('',#46111,#5863);
#3493=LINE('',#46190,#5864);
#3494=LINE('',#46197,#5865);
#3495=LINE('',#46224,#5866);
#3496=LINE('',#46226,#5867);
#3497=LINE('',#46227,#5868);
#3498=LINE('',#46231,#5869);
#3499=LINE('',#46232,#5870);
#3500=LINE('',#46233,#5871);
#3501=LINE('',#46237,#5872);
#3502=LINE('',#46239,#5873);
#3503=LINE('',#46240,#5874);
#3504=LINE('',#46244,#5875);
#3505=LINE('',#46246,#5876);
#3506=LINE('',#46247,#5877);
#3507=LINE('',#46251,#5878);
#3508=LINE('',#46252,#5879);
#3509=LINE('',#46253,#5880);
#3510=LINE('',#46255,#5881);
#3511=LINE('',#46256,#5882);
#3512=LINE('',#46260,#5883);
#3513=LINE('',#46262,#5884);
#3514=LINE('',#46263,#5885);
#3515=LINE('',#46265,#5886);
#3516=LINE('',#46266,#5887);
#3517=LINE('',#46270,#5888);
#3518=LINE('',#46272,#5889);
#3519=LINE('',#46273,#5890);
#3520=LINE('',#46277,#5891);
#3521=LINE('',#46279,#5892);
#3522=LINE('',#46280,#5893);
#3523=LINE('',#46282,#5894);
#3524=LINE('',#46283,#5895);
#3525=LINE('',#46285,#5896);
#3526=LINE('',#46286,#5897);
#3527=LINE('',#46288,#5898);
#3528=LINE('',#46289,#5899);
#3529=LINE('',#46291,#5900);
#3530=LINE('',#46292,#5901);
#3531=LINE('',#46294,#5902);
#3532=LINE('',#46295,#5903);
#3533=LINE('',#46297,#5904);
#3534=LINE('',#46298,#5905);
#3535=LINE('',#46300,#5906);
#3536=LINE('',#46301,#5907);
#3537=LINE('',#46303,#5908);
#3538=LINE('',#46305,#5909);
#3539=LINE('',#46313,#5910);
#3540=LINE('',#46319,#5911);
#3541=LINE('',#46352,#5912);
#3542=LINE('',#46356,#5913);
#3543=LINE('',#46358,#5914);
#3544=LINE('',#46359,#5915);
#3545=LINE('',#46363,#5916);
#3546=LINE('',#46364,#5917);
#3547=LINE('',#46365,#5918);
#3548=LINE('',#46369,#5919);
#3549=LINE('',#46370,#5920);
#3550=LINE('',#46372,#5921);
#3551=LINE('',#46373,#5922);
#3552=LINE('',#46377,#5923);
#3553=LINE('',#46378,#5924);
#3554=LINE('',#46380,#5925);
#3555=LINE('',#46381,#5926);
#3556=LINE('',#46383,#5927);
#3557=LINE('',#46385,#5928);
#3558=LINE('',#46387,#5929);
#3559=LINE('',#46388,#5930);
#3560=LINE('',#46391,#5931);
#3561=LINE('',#46392,#5932);
#3562=LINE('',#46395,#5933);
#3563=LINE('',#46397,#5934);
#3564=LINE('',#46398,#5935);
#3565=LINE('',#46402,#5936);
#3566=LINE('',#46404,#5937);
#3567=LINE('',#46405,#5938);
#3568=LINE('',#46409,#5939);
#3569=LINE('',#46411,#5940);
#3570=LINE('',#46412,#5941);
#3571=LINE('',#46414,#5942);
#3572=LINE('',#46416,#5943);
#3573=LINE('',#46417,#5944);
#3574=LINE('',#46419,#5945);
#3575=LINE('',#46420,#5946);
#3576=LINE('',#46422,#5947);
#3577=LINE('',#46423,#5948);
#3578=LINE('',#46425,#5949);
#3579=LINE('',#46426,#5950);
#3580=LINE('',#46429,#5951);
#3581=LINE('',#46430,#5952);
#3582=LINE('',#46431,#5953);
#3583=LINE('',#46433,#5954);
#3584=LINE('',#46435,#5955);
#3585=LINE('',#46441,#5956);
#3586=LINE('',#46443,#5957);
#3587=LINE('',#46444,#5958);
#3588=LINE('',#46448,#5959);
#3589=LINE('',#46449,#5960);
#3590=LINE('',#46450,#5961);
#3591=LINE('',#46454,#5962);
#3592=LINE('',#46456,#5963);
#3593=LINE('',#46457,#5964);
#3594=LINE('',#46461,#5965);
#3595=LINE('',#46463,#5966);
#3596=LINE('',#46464,#5967);
#3597=LINE('',#46468,#5968);
#3598=LINE('',#46469,#5969);
#3599=LINE('',#46470,#5970);
#3600=LINE('',#46472,#5971);
#3601=LINE('',#46473,#5972);
#3602=LINE('',#46477,#5973);
#3603=LINE('',#46479,#5974);
#3604=LINE('',#46480,#5975);
#3605=LINE('',#46482,#5976);
#3606=LINE('',#46483,#5977);
#3607=LINE('',#46487,#5978);
#3608=LINE('',#46489,#5979);
#3609=LINE('',#46490,#5980);
#3610=LINE('',#46494,#5981);
#3611=LINE('',#46496,#5982);
#3612=LINE('',#46497,#5983);
#3613=LINE('',#46499,#5984);
#3614=LINE('',#46500,#5985);
#3615=LINE('',#46502,#5986);
#3616=LINE('',#46503,#5987);
#3617=LINE('',#46505,#5988);
#3618=LINE('',#46506,#5989);
#3619=LINE('',#46508,#5990);
#3620=LINE('',#46509,#5991);
#3621=LINE('',#46511,#5992);
#3622=LINE('',#46512,#5993);
#3623=LINE('',#46514,#5994);
#3624=LINE('',#46515,#5995);
#3625=LINE('',#46517,#5996);
#3626=LINE('',#46518,#5997);
#3627=LINE('',#46520,#5998);
#3628=LINE('',#46522,#5999);
#3629=LINE('',#46646,#6000);
#3630=LINE('',#46679,#6001);
#3631=LINE('',#46684,#6002);
#3632=LINE('',#46686,#6003);
#3633=LINE('',#46688,#6004);
#3634=LINE('',#46692,#6005);
#3635=LINE('',#46697,#6006);
#3636=LINE('',#46698,#6007);
#3637=LINE('',#46704,#6008);
#3638=LINE('',#46731,#6009);
#3639=LINE('',#46779,#6010);
#3640=LINE('',#46827,#6011);
#3641=LINE('',#46875,#6012);
#3642=LINE('',#46929,#6013);
#3643=LINE('',#46977,#6014);
#3644=LINE('',#47025,#6015);
#3645=LINE('',#47079,#6016);
#3646=LINE('',#47127,#6017);
#3647=LINE('',#47175,#6018);
#3648=LINE('',#47223,#6019);
#3649=LINE('',#47277,#6020);
#3650=LINE('',#47325,#6021);
#3651=LINE('',#47373,#6022);
#3652=LINE('',#47427,#6023);
#3653=LINE('',#47475,#6024);
#3654=LINE('',#47523,#6025);
#3655=LINE('',#47571,#6026);
#3656=LINE('',#47625,#6027);
#3657=LINE('',#47673,#6028);
#3658=LINE('',#47683,#6029);
#3659=LINE('',#47709,#6030);
#3660=LINE('',#47734,#6031);
#3661=LINE('',#47759,#6032);
#3662=LINE('',#47783,#6033);
#3663=LINE('',#47807,#6034);
#3664=LINE('',#47832,#6035);
#3665=LINE('',#47857,#6036);
#3666=LINE('',#47881,#6037);
#3667=LINE('',#47906,#6038);
#3668=LINE('',#47931,#6039);
#3669=LINE('',#47955,#6040);
#3670=LINE('',#47979,#6041);
#3671=LINE('',#48004,#6042);
#3672=LINE('',#48029,#6043);
#3673=LINE('',#48053,#6044);
#3674=LINE('',#48078,#6045);
#3675=LINE('',#48103,#6046);
#3676=LINE('',#48127,#6047);
#3677=LINE('',#49685,#6048);
#3678=LINE('',#49696,#6049);
#3679=LINE('',#49698,#6050);
#3680=LINE('',#49699,#6051);
#3681=LINE('',#49702,#6052);
#3682=LINE('',#49703,#6053);
#3683=LINE('',#49706,#6054);
#3684=LINE('',#49707,#6055);
#3685=LINE('',#49710,#6056);
#3686=LINE('',#49712,#6057);
#3687=LINE('',#49713,#6058);
#3688=LINE('',#49716,#6059);
#3689=LINE('',#49718,#6060);
#3690=LINE('',#49725,#6061);
#3691=LINE('',#49731,#6062);
#3692=LINE('',#49758,#6063);
#3693=LINE('',#49806,#6064);
#3694=LINE('',#49854,#6065);
#3695=LINE('',#49902,#6066);
#3696=LINE('',#49956,#6067);
#3697=LINE('',#50004,#6068);
#3698=LINE('',#50052,#6069);
#3699=LINE('',#50106,#6070);
#3700=LINE('',#50154,#6071);
#3701=LINE('',#50202,#6072);
#3702=LINE('',#50250,#6073);
#3703=LINE('',#50304,#6074);
#3704=LINE('',#50352,#6075);
#3705=LINE('',#50400,#6076);
#3706=LINE('',#50454,#6077);
#3707=LINE('',#50502,#6078);
#3708=LINE('',#50550,#6079);
#3709=LINE('',#50598,#6080);
#3710=LINE('',#50652,#6081);
#3711=LINE('',#50700,#6082);
#3712=LINE('',#50710,#6083);
#3713=LINE('',#50736,#6084);
#3714=LINE('',#50761,#6085);
#3715=LINE('',#50786,#6086);
#3716=LINE('',#50810,#6087);
#3717=LINE('',#50834,#6088);
#3718=LINE('',#50859,#6089);
#3719=LINE('',#50884,#6090);
#3720=LINE('',#50908,#6091);
#3721=LINE('',#50933,#6092);
#3722=LINE('',#50958,#6093);
#3723=LINE('',#50982,#6094);
#3724=LINE('',#51006,#6095);
#3725=LINE('',#51031,#6096);
#3726=LINE('',#51056,#6097);
#3727=LINE('',#51080,#6098);
#3728=LINE('',#51105,#6099);
#3729=LINE('',#51130,#6100);
#3730=LINE('',#51154,#6101);
#3731=LINE('',#52692,#6102);
#3732=LINE('',#52694,#6103);
#3733=LINE('',#52696,#6104);
#3734=LINE('',#52697,#6105);
#3735=LINE('',#52701,#6106);
#3736=LINE('',#52704,#6107);
#3737=LINE('',#52705,#6108);
#3738=LINE('',#52711,#6109);
#3739=LINE('',#52713,#6110);
#3740=LINE('',#52715,#6111);
#3741=LINE('',#52716,#6112);
#3742=LINE('',#52720,#6113);
#3743=LINE('',#52723,#6114);
#3744=LINE('',#52724,#6115);
#3745=LINE('',#52730,#6116);
#3746=LINE('',#52732,#6117);
#3747=LINE('',#52734,#6118);
#3748=LINE('',#52735,#6119);
#3749=LINE('',#52739,#6120);
#3750=LINE('',#52742,#6121);
#3751=LINE('',#52743,#6122);
#3752=LINE('',#52749,#6123);
#3753=LINE('',#52751,#6124);
#3754=LINE('',#52753,#6125);
#3755=LINE('',#52754,#6126);
#3756=LINE('',#52758,#6127);
#3757=LINE('',#52761,#6128);
#3758=LINE('',#52762,#6129);
#3759=LINE('',#52768,#6130);
#3760=LINE('',#52770,#6131);
#3761=LINE('',#52772,#6132);
#3762=LINE('',#52773,#6133);
#3763=LINE('',#52777,#6134);
#3764=LINE('',#52780,#6135);
#3765=LINE('',#52781,#6136);
#3766=LINE('',#52787,#6137);
#3767=LINE('',#52789,#6138);
#3768=LINE('',#52791,#6139);
#3769=LINE('',#52792,#6140);
#3770=LINE('',#52796,#6141);
#3771=LINE('',#52799,#6142);
#3772=LINE('',#52800,#6143);
#3773=LINE('',#52806,#6144);
#3774=LINE('',#52808,#6145);
#3775=LINE('',#52810,#6146);
#3776=LINE('',#52811,#6147);
#3777=LINE('',#52815,#6148);
#3778=LINE('',#52818,#6149);
#3779=LINE('',#52819,#6150);
#3780=LINE('',#52825,#6151);
#3781=LINE('',#52827,#6152);
#3782=LINE('',#52829,#6153);
#3783=LINE('',#52830,#6154);
#3784=LINE('',#52834,#6155);
#3785=LINE('',#52837,#6156);
#3786=LINE('',#52838,#6157);
#3787=LINE('',#52844,#6158);
#3788=LINE('',#52846,#6159);
#3789=LINE('',#52848,#6160);
#3790=LINE('',#52849,#6161);
#3791=LINE('',#52853,#6162);
#3792=LINE('',#52856,#6163);
#3793=LINE('',#52857,#6164);
#3794=LINE('',#52863,#6165);
#3795=LINE('',#52865,#6166);
#3796=LINE('',#52867,#6167);
#3797=LINE('',#52868,#6168);
#3798=LINE('',#52872,#6169);
#3799=LINE('',#52875,#6170);
#3800=LINE('',#52876,#6171);
#3801=LINE('',#52882,#6172);
#3802=LINE('',#52884,#6173);
#3803=LINE('',#52886,#6174);
#3804=LINE('',#52887,#6175);
#3805=LINE('',#52891,#6176);
#3806=LINE('',#52894,#6177);
#3807=LINE('',#52895,#6178);
#3808=LINE('',#52901,#6179);
#3809=LINE('',#52903,#6180);
#3810=LINE('',#52905,#6181);
#3811=LINE('',#52906,#6182);
#3812=LINE('',#52910,#6183);
#3813=LINE('',#52913,#6184);
#3814=LINE('',#52914,#6185);
#3815=LINE('',#52920,#6186);
#3816=LINE('',#52922,#6187);
#3817=LINE('',#52924,#6188);
#3818=LINE('',#52925,#6189);
#3819=LINE('',#52929,#6190);
#3820=LINE('',#52932,#6191);
#3821=LINE('',#52933,#6192);
#3822=LINE('',#52939,#6193);
#3823=LINE('',#52941,#6194);
#3824=LINE('',#52943,#6195);
#3825=LINE('',#52944,#6196);
#3826=LINE('',#52948,#6197);
#3827=LINE('',#52951,#6198);
#3828=LINE('',#52952,#6199);
#3829=LINE('',#52958,#6200);
#3830=LINE('',#52960,#6201);
#3831=LINE('',#52962,#6202);
#3832=LINE('',#52963,#6203);
#3833=LINE('',#52967,#6204);
#3834=LINE('',#52970,#6205);
#3835=LINE('',#52971,#6206);
#3836=LINE('',#52977,#6207);
#3837=LINE('',#52979,#6208);
#3838=LINE('',#52981,#6209);
#3839=LINE('',#52982,#6210);
#3840=LINE('',#52986,#6211);
#3841=LINE('',#52989,#6212);
#3842=LINE('',#52990,#6213);
#3843=LINE('',#52996,#6214);
#3844=LINE('',#52998,#6215);
#3845=LINE('',#53000,#6216);
#3846=LINE('',#53001,#6217);
#3847=LINE('',#53005,#6218);
#3848=LINE('',#53008,#6219);
#3849=LINE('',#53009,#6220);
#3850=LINE('',#53015,#6221);
#3851=LINE('',#53017,#6222);
#3852=LINE('',#53019,#6223);
#3853=LINE('',#53020,#6224);
#3854=LINE('',#53025,#6225);
#3855=LINE('',#53029,#6226);
#3856=LINE('',#53030,#6227);
#3857=LINE('',#53038,#6228);
#3858=LINE('',#53040,#6229);
#3859=LINE('',#53042,#6230);
#3860=LINE('',#53043,#6231);
#3861=LINE('',#53047,#6232);
#3862=LINE('',#53050,#6233);
#3863=LINE('',#53051,#6234);
#3864=LINE('',#53057,#6235);
#3865=LINE('',#53059,#6236);
#3866=LINE('',#53061,#6237);
#3867=LINE('',#53062,#6238);
#3868=LINE('',#53066,#6239);
#3869=LINE('',#53069,#6240);
#3870=LINE('',#53070,#6241);
#3871=LINE('',#53076,#6242);
#3872=LINE('',#53078,#6243);
#3873=LINE('',#53080,#6244);
#3874=LINE('',#53081,#6245);
#3875=LINE('',#53085,#6246);
#3876=LINE('',#53088,#6247);
#3877=LINE('',#53089,#6248);
#3878=LINE('',#53095,#6249);
#3879=LINE('',#53097,#6250);
#3880=LINE('',#53099,#6251);
#3881=LINE('',#53100,#6252);
#3882=LINE('',#53104,#6253);
#3883=LINE('',#53107,#6254);
#3884=LINE('',#53108,#6255);
#3885=LINE('',#53114,#6256);
#3886=LINE('',#53116,#6257);
#3887=LINE('',#53118,#6258);
#3888=LINE('',#53119,#6259);
#3889=LINE('',#53123,#6260);
#3890=LINE('',#53126,#6261);
#3891=LINE('',#53127,#6262);
#3892=LINE('',#53133,#6263);
#3893=LINE('',#53135,#6264);
#3894=LINE('',#53137,#6265);
#3895=LINE('',#53138,#6266);
#3896=LINE('',#53142,#6267);
#3897=LINE('',#53145,#6268);
#3898=LINE('',#53146,#6269);
#3899=LINE('',#53152,#6270);
#3900=LINE('',#53154,#6271);
#3901=LINE('',#53156,#6272);
#3902=LINE('',#53157,#6273);
#3903=LINE('',#53161,#6274);
#3904=LINE('',#53164,#6275);
#3905=LINE('',#53165,#6276);
#3906=LINE('',#53171,#6277);
#3907=LINE('',#53173,#6278);
#3908=LINE('',#53175,#6279);
#3909=LINE('',#53176,#6280);
#3910=LINE('',#53180,#6281);
#3911=LINE('',#53183,#6282);
#3912=LINE('',#53184,#6283);
#3913=LINE('',#53190,#6284);
#3914=LINE('',#53192,#6285);
#3915=LINE('',#53194,#6286);
#3916=LINE('',#53195,#6287);
#3917=LINE('',#53199,#6288);
#3918=LINE('',#53202,#6289);
#3919=LINE('',#53203,#6290);
#3920=LINE('',#53209,#6291);
#3921=LINE('',#53211,#6292);
#3922=LINE('',#53213,#6293);
#3923=LINE('',#53214,#6294);
#3924=LINE('',#53218,#6295);
#3925=LINE('',#53221,#6296);
#3926=LINE('',#53222,#6297);
#3927=LINE('',#53228,#6298);
#3928=LINE('',#53230,#6299);
#3929=LINE('',#53232,#6300);
#3930=LINE('',#53233,#6301);
#3931=LINE('',#53237,#6302);
#3932=LINE('',#53240,#6303);
#3933=LINE('',#53241,#6304);
#3934=LINE('',#53247,#6305);
#3935=LINE('',#53249,#6306);
#3936=LINE('',#53251,#6307);
#3937=LINE('',#53252,#6308);
#3938=LINE('',#53256,#6309);
#3939=LINE('',#53259,#6310);
#3940=LINE('',#53260,#6311);
#3941=LINE('',#53266,#6312);
#3942=LINE('',#53268,#6313);
#3943=LINE('',#53270,#6314);
#3944=LINE('',#53271,#6315);
#3945=LINE('',#53275,#6316);
#3946=LINE('',#53278,#6317);
#3947=LINE('',#53279,#6318);
#3948=LINE('',#53285,#6319);
#3949=LINE('',#53287,#6320);
#3950=LINE('',#53289,#6321);
#3951=LINE('',#53290,#6322);
#3952=LINE('',#53294,#6323);
#3953=LINE('',#53297,#6324);
#3954=LINE('',#53298,#6325);
#3955=LINE('',#53304,#6326);
#3956=LINE('',#53306,#6327);
#3957=LINE('',#53308,#6328);
#3958=LINE('',#53309,#6329);
#3959=LINE('',#53313,#6330);
#3960=LINE('',#53316,#6331);
#3961=LINE('',#53317,#6332);
#3962=LINE('',#53323,#6333);
#3963=LINE('',#53325,#6334);
#3964=LINE('',#53327,#6335);
#3965=LINE('',#53328,#6336);
#3966=LINE('',#53332,#6337);
#3967=LINE('',#53335,#6338);
#3968=LINE('',#53336,#6339);
#3969=LINE('',#53342,#6340);
#3970=LINE('',#53344,#6341);
#3971=LINE('',#53346,#6342);
#3972=LINE('',#53347,#6343);
#3973=LINE('',#53351,#6344);
#3974=LINE('',#53354,#6345);
#3975=LINE('',#53355,#6346);
#3976=LINE('',#53361,#6347);
#3977=LINE('',#53363,#6348);
#3978=LINE('',#53365,#6349);
#3979=LINE('',#53366,#6350);
#3980=LINE('',#53370,#6351);
#3981=LINE('',#53373,#6352);
#3982=LINE('',#53374,#6353);
#3983=LINE('',#53380,#6354);
#3984=LINE('',#53382,#6355);
#3985=LINE('',#53384,#6356);
#3986=LINE('',#53385,#6357);
#3987=LINE('',#53388,#6358);
#3988=LINE('',#53390,#6359);
#3989=LINE('',#53391,#6360);
#3990=LINE('',#53394,#6361);
#3991=LINE('',#53396,#6362);
#3992=LINE('',#53397,#6363);
#3993=LINE('',#53400,#6364);
#3994=LINE('',#53402,#6365);
#3995=LINE('',#53403,#6366);
#3996=LINE('',#53406,#6367);
#3997=LINE('',#53408,#6368);
#3998=LINE('',#53409,#6369);
#3999=LINE('',#53411,#6370);
#4000=LINE('',#53412,#6371);
#4001=LINE('',#53418,#6372);
#4002=LINE('',#53427,#6373);
#4003=LINE('',#53428,#6374);
#4004=LINE('',#53432,#6375);
#4005=LINE('',#53438,#6376);
#4006=LINE('',#53440,#6377);
#4007=LINE('',#53441,#6378);
#4008=LINE('',#53445,#6379);
#4009=LINE('',#53446,#6380);
#4010=LINE('',#53447,#6381);
#4011=LINE('',#53451,#6382);
#4012=LINE('',#53453,#6383);
#4013=LINE('',#53454,#6384);
#4014=LINE('',#53458,#6385);
#4015=LINE('',#53459,#6386);
#4016=LINE('',#53460,#6387);
#4017=LINE('',#53462,#6388);
#4018=LINE('',#53463,#6389);
#4019=LINE('',#53467,#6390);
#4020=LINE('',#53469,#6391);
#4021=LINE('',#53470,#6392);
#4022=LINE('',#53474,#6393);
#4023=LINE('',#53475,#6394);
#4024=LINE('',#53476,#6395);
#4025=LINE('',#53480,#6396);
#4026=LINE('',#53482,#6397);
#4027=LINE('',#53483,#6398);
#4028=LINE('',#53487,#6399);
#4029=LINE('',#53488,#6400);
#4030=LINE('',#53489,#6401);
#4031=LINE('',#53491,#6402);
#4032=LINE('',#53492,#6403);
#4033=LINE('',#53496,#6404);
#4034=LINE('',#53498,#6405);
#4035=LINE('',#53499,#6406);
#4036=LINE('',#53503,#6407);
#4037=LINE('',#53504,#6408);
#4038=LINE('',#53505,#6409);
#4039=LINE('',#53509,#6410);
#4040=LINE('',#53511,#6411);
#4041=LINE('',#53512,#6412);
#4042=LINE('',#53516,#6413);
#4043=LINE('',#53517,#6414);
#4044=LINE('',#53518,#6415);
#4045=LINE('',#53520,#6416);
#4046=LINE('',#53521,#6417);
#4047=LINE('',#53523,#6418);
#4048=LINE('',#53524,#6419);
#4049=LINE('',#53526,#6420);
#4050=LINE('',#53527,#6421);
#4051=LINE('',#53529,#6422);
#4052=LINE('',#53530,#6423);
#4053=LINE('',#53532,#6424);
#4054=LINE('',#53534,#6425);
#4055=LINE('',#53536,#6426);
#4056=LINE('',#53540,#6427);
#4057=LINE('',#53542,#6428);
#4058=LINE('',#53544,#6429);
#4059=LINE('',#53546,#6430);
#4060=LINE('',#53548,#6431);
#4061=LINE('',#53549,#6432);
#4062=LINE('',#53552,#6433);
#4063=LINE('',#53554,#6434);
#4064=LINE('',#53555,#6435);
#4065=LINE('',#53558,#6436);
#4066=LINE('',#53559,#6437);
#4067=LINE('',#53562,#6438);
#4068=LINE('',#53564,#6439);
#4069=LINE('',#53565,#6440);
#4070=LINE('',#53568,#6441);
#4071=LINE('',#53569,#6442);
#4072=LINE('',#53571,#6443);
#4073=LINE('',#53573,#6444);
#4074=LINE('',#53576,#6445);
#4075=LINE('',#53578,#6446);
#4076=LINE('',#53579,#6447);
#4077=LINE('',#53582,#6448);
#4078=LINE('',#53583,#6449);
#4079=LINE('',#53586,#6450);
#4080=LINE('',#53587,#6451);
#4081=LINE('',#53590,#6452);
#4082=LINE('',#53591,#6453);
#4083=LINE('',#53594,#6454);
#4084=LINE('',#53595,#6455);
#4085=LINE('',#53597,#6456);
#4086=LINE('',#53600,#6457);
#4087=LINE('',#53601,#6458);
#4088=LINE('',#53602,#6459);
#4089=LINE('',#53614,#6460);
#4090=LINE('',#53616,#6461);
#4091=LINE('',#53621,#6462);
#4092=LINE('',#53645,#6463);
#4093=LINE('',#53693,#6464);
#4094=LINE('',#53741,#6465);
#4095=LINE('',#53795,#6466);
#4096=LINE('',#53843,#6467);
#4097=LINE('',#53891,#6468);
#4098=LINE('',#53939,#6469);
#4099=LINE('',#53993,#6470);
#4100=LINE('',#54041,#6471);
#4101=LINE('',#54089,#6472);
#4102=LINE('',#54143,#6473);
#4103=LINE('',#54191,#6474);
#4104=LINE('',#54238,#6475);
#4105=LINE('',#54258,#6476);
#4106=LINE('',#54282,#6477);
#4107=LINE('',#54307,#6478);
#4108=LINE('',#54332,#6479);
#4109=LINE('',#54356,#6480);
#4110=LINE('',#54381,#6481);
#4111=LINE('',#54406,#6482);
#4112=LINE('',#54430,#6483);
#4113=LINE('',#54454,#6484);
#4114=LINE('',#54479,#6485);
#4115=LINE('',#54504,#6486);
#4116=LINE('',#55561,#6487);
#4117=LINE('',#55563,#6488);
#4118=LINE('',#55564,#6489);
#4119=LINE('',#55574,#6490);
#4120=LINE('',#55575,#6491);
#4121=LINE('',#55585,#6492);
#4122=LINE('',#55586,#6493);
#4123=LINE('',#55596,#6494);
#4124=LINE('',#55597,#6495);
#4125=LINE('',#55607,#6496);
#4126=LINE('',#55608,#6497);
#4127=LINE('',#55616,#6498);
#4128=LINE('',#55622,#6499);
#4129=VECTOR('',#29994,10.);
#4130=VECTOR('',#29999,10.);
#4131=VECTOR('',#30002,10.);
#4132=VECTOR('',#30005,10.);
#4133=VECTOR('',#30052,10.);
#4134=VECTOR('',#30055,10.);
#4135=VECTOR('',#30066,10.);
#4136=VECTOR('',#30067,10.);
#4137=VECTOR('',#30078,10.);
#4138=VECTOR('',#30079,10.);
#4139=VECTOR('',#30090,10.);
#4140=VECTOR('',#30091,10.);
#4141=VECTOR('',#30098,10.);
#4142=VECTOR('',#30101,10.);
#4143=VECTOR('',#30104,10.);
#4144=VECTOR('',#30105,10.);
#4145=VECTOR('',#30108,10.);
#4146=VECTOR('',#30113,10.);
#4147=VECTOR('',#30114,10.);
#4148=VECTOR('',#30125,10.);
#4149=VECTOR('',#30128,10.);
#4150=VECTOR('',#30139,10.);
#4151=VECTOR('',#30140,10.);
#4152=VECTOR('',#30149,10.);
#4153=VECTOR('',#30158,10.);
#4154=VECTOR('',#30165,10.);
#4155=VECTOR('',#30168,10.);
#4156=VECTOR('',#30171,10.);
#4157=VECTOR('',#30176,10.);
#4158=VECTOR('',#30179,10.);
#4159=VECTOR('',#30182,10.);
#4160=VECTOR('',#30185,10.);
#4161=VECTOR('',#30194,10.);
#4162=VECTOR('',#30197,10.);
#4163=VECTOR('',#30208,10.);
#4164=VECTOR('',#30209,10.);
#4165=VECTOR('',#30220,10.);
#4166=VECTOR('',#30221,10.);
#4167=VECTOR('',#30232,10.);
#4168=VECTOR('',#30233,10.);
#4169=VECTOR('',#30240,10.);
#4170=VECTOR('',#30243,10.);
#4171=VECTOR('',#30246,10.);
#4172=VECTOR('',#30247,10.);
#4173=VECTOR('',#30250,10.);
#4174=VECTOR('',#30255,10.);
#4175=VECTOR('',#30256,10.);
#4176=VECTOR('',#30265,10.);
#4177=VECTOR('',#30268,10.);
#4178=VECTOR('',#30279,10.);
#4179=VECTOR('',#30280,10.);
#4180=VECTOR('',#30291,10.);
#4181=VECTOR('',#30292,10.);
#4182=VECTOR('',#30303,10.);
#4183=VECTOR('',#30304,10.);
#4184=VECTOR('',#30311,10.);
#4185=VECTOR('',#30314,10.);
#4186=VECTOR('',#30317,10.);
#4187=VECTOR('',#30318,10.);
#4188=VECTOR('',#30321,10.);
#4189=VECTOR('',#30326,10.);
#4190=VECTOR('',#30327,10.);
#4191=VECTOR('',#30340,70.2);
#4192=VECTOR('',#30343,10.);
#4193=VECTOR('',#30346,10.);
#4194=VECTOR('',#30359,10.);
#4195=VECTOR('',#30360,10.);
#4196=VECTOR('',#30365,20.05);
#4197=VECTOR('',#30370,10.);
#4198=VECTOR('',#30377,10.);
#4199=VECTOR('',#30380,10.);
#4200=VECTOR('',#30381,10.);
#4201=VECTOR('',#30384,10.);
#4202=VECTOR('',#30389,10.);
#4203=VECTOR('',#30414,10.);
#4204=VECTOR('',#30417,10.);
#4205=VECTOR('',#30420,10.);
#4206=VECTOR('',#30423,10.);
#4207=VECTOR('',#30424,10.);
#4208=VECTOR('',#30427,16.75);
#4209=VECTOR('',#30432,10.);
#4210=VECTOR('',#30435,10.);
#4211=VECTOR('',#30440,10.);
#4212=VECTOR('',#30443,10.);
#4213=VECTOR('',#30454,10.);
#4214=VECTOR('',#30455,10.);
#4215=VECTOR('',#30464,10.);
#4216=VECTOR('',#30467,10.);
#4217=VECTOR('',#30468,10.);
#4218=VECTOR('',#30471,10.);
#4219=VECTOR('',#30472,10.);
#4220=VECTOR('',#30479,10.);
#4221=VECTOR('',#30482,10.);
#4222=VECTOR('',#30493,10.);
#4223=VECTOR('',#30504,10.);
#4224=VECTOR('',#30517,10.);
#4225=VECTOR('',#30518,10.);
#4226=VECTOR('',#30527,10.);
#4227=VECTOR('',#30534,10.);
#4228=VECTOR('',#30537,10.);
#4229=VECTOR('',#30540,10.);
#4230=VECTOR('',#30543,10.);
#4231=VECTOR('',#30568,10.);
#4232=VECTOR('',#30569,10.);
#4233=VECTOR('',#30572,16.75);
#4234=VECTOR('',#30577,7.);
#4235=VECTOR('',#30580,7.);
#4236=VECTOR('',#30583,6.9);
#4237=VECTOR('',#30590,6.9);
#4238=VECTOR('',#30597,16.75);
#4239=VECTOR('',#30610,10.);
#4240=VECTOR('',#30611,10.);
#4241=VECTOR('',#30614,5.05);
#4242=VECTOR('',#30621,5.05);
#4243=VECTOR('',#30628,5.05);
#4244=VECTOR('',#30635,5.05);
#4245=VECTOR('',#30642,5.05);
#4246=VECTOR('',#30649,5.05);
#4247=VECTOR('',#30656,5.05);
#4248=VECTOR('',#30663,5.05);
#4249=VECTOR('',#30670,5.05);
#4250=VECTOR('',#30677,5.05);
#4251=VECTOR('',#30684,5.05);
#4252=VECTOR('',#30691,5.05);
#4253=VECTOR('',#30704,13.);
#4254=VECTOR('',#30707,10.);
#4255=VECTOR('',#30710,10.);
#4256=VECTOR('',#30713,10.);
#4257=VECTOR('',#30718,10.);
#4258=VECTOR('',#30721,10.);
#4259=VECTOR('',#30724,10.);
#4260=VECTOR('',#30731,10.);
#4261=VECTOR('',#30732,10.);
#4262=VECTOR('',#30735,10.);
#4263=VECTOR('',#30738,10.);
#4264=VECTOR('',#30741,10.);
#4265=VECTOR('',#30744,10.);
#4266=VECTOR('',#30747,10.);
#4267=VECTOR('',#30750,10.);
#4268=VECTOR('',#30755,10.);
#4269=VECTOR('',#30760,10.);
#4270=VECTOR('',#30765,10.);
#4271=VECTOR('',#30766,10.);
#4272=VECTOR('',#30769,10.);
#4273=VECTOR('',#30770,10.);
#4274=VECTOR('',#30771,10.);
#4275=VECTOR('',#30774,10.);
#4276=VECTOR('',#30775,10.);
#4277=VECTOR('',#30776,10.);
#4278=VECTOR('',#30781,10.);
#4279=VECTOR('',#30784,10.);
#4280=VECTOR('',#30787,10.);
#4281=VECTOR('',#30788,10.);
#4282=VECTOR('',#30789,10.);
#4283=VECTOR('',#30792,10.);
#4284=VECTOR('',#30793,10.);
#4285=VECTOR('',#30796,10.);
#4286=VECTOR('',#30799,10.);
#4287=VECTOR('',#30800,10.);
#4288=VECTOR('',#30801,10.);
#4289=VECTOR('',#30802,10.);
#4290=VECTOR('',#30805,10.);
#4291=VECTOR('',#30806,10.);
#4292=VECTOR('',#30807,10.);
#4293=VECTOR('',#30810,10.);
#4294=VECTOR('',#30811,10.);
#4295=VECTOR('',#30814,10.);
#4296=VECTOR('',#30817,10.);
#4297=VECTOR('',#30822,10.);
#4298=VECTOR('',#30823,10.);
#4299=VECTOR('',#30824,10.);
#4300=VECTOR('',#30825,10.);
#4301=VECTOR('',#30828,10.);
#4302=VECTOR('',#30829,10.);
#4303=VECTOR('',#30830,10.);
#4304=VECTOR('',#30833,10.);
#4305=VECTOR('',#30834,10.);
#4306=VECTOR('',#30835,10.);
#4307=VECTOR('',#30838,10.);
#4308=VECTOR('',#30841,10.);
#4309=VECTOR('',#30844,10.);
#4310=VECTOR('',#30845,10.);
#4311=VECTOR('',#30846,10.);
#4312=VECTOR('',#30849,10.);
#4313=VECTOR('',#30850,10.);
#4314=VECTOR('',#30853,10.);
#4315=VECTOR('',#30856,10.);
#4316=VECTOR('',#30857,10.);
#4317=VECTOR('',#30858,10.);
#4318=VECTOR('',#30859,10.);
#4319=VECTOR('',#30862,10.);
#4320=VECTOR('',#30863,10.);
#4321=VECTOR('',#30864,10.);
#4322=VECTOR('',#30867,10.);
#4323=VECTOR('',#30868,10.);
#4324=VECTOR('',#30869,10.);
#4325=VECTOR('',#30872,10.);
#4326=VECTOR('',#30875,10.);
#4327=VECTOR('',#30878,10.);
#4328=VECTOR('',#30879,10.);
#4329=VECTOR('',#30880,10.);
#4330=VECTOR('',#30883,10.);
#4331=VECTOR('',#30884,10.);
#4332=VECTOR('',#30887,10.);
#4333=VECTOR('',#30890,10.);
#4334=VECTOR('',#30891,10.);
#4335=VECTOR('',#30902,91.5);
#4336=VECTOR('',#30909,92.);
#4337=VECTOR('',#30934,10.);
#4338=VECTOR('',#30937,10.);
#4339=VECTOR('',#30940,10.);
#4340=VECTOR('',#30943,10.);
#4341=VECTOR('',#30946,10.);
#4342=VECTOR('',#30951,10.);
#4343=VECTOR('',#30954,10.);
#4344=VECTOR('',#30957,10.);
#4345=VECTOR('',#30960,10.);
#4346=VECTOR('',#31031,56.);
#4347=VECTOR('',#31034,10.);
#4348=VECTOR('',#31035,10.);
#4349=VECTOR('',#31036,10.);
#4350=VECTOR('',#31037,10.);
#4351=VECTOR('',#31038,10.);
#4352=VECTOR('',#31039,10.);
#4353=VECTOR('',#31040,10.);
#4354=VECTOR('',#31041,10.);
#4355=VECTOR('',#31042,10.);
#4356=VECTOR('',#31043,10.);
#4357=VECTOR('',#31044,10.);
#4358=VECTOR('',#31045,10.);
#4359=VECTOR('',#31046,10.);
#4360=VECTOR('',#31047,10.);
#4361=VECTOR('',#31048,10.);
#4362=VECTOR('',#31049,10.);
#4363=VECTOR('',#31050,10.);
#4364=VECTOR('',#31051,10.);
#4365=VECTOR('',#31052,10.);
#4366=VECTOR('',#31053,10.);
#4367=VECTOR('',#31054,10.);
#4368=VECTOR('',#31055,10.);
#4369=VECTOR('',#31056,1.5);
#4370=VECTOR('',#31057,10.);
#4371=VECTOR('',#31058,10.);
#4372=VECTOR('',#31059,1.5);
#4373=VECTOR('',#31060,10.);
#4374=VECTOR('',#31061,10.);
#4375=VECTOR('',#31062,1.5);
#4376=VECTOR('',#31063,10.);
#4377=VECTOR('',#31064,1.5);
#4378=VECTOR('',#31065,10.);
#4379=VECTOR('',#31066,10.);
#4380=VECTOR('',#31067,10.);
#4381=VECTOR('',#31068,10.);
#4382=VECTOR('',#31069,10.);
#4383=VECTOR('',#31070,10.);
#4384=VECTOR('',#31071,10.);
#4385=VECTOR('',#31072,10.);
#4386=VECTOR('',#31073,10.);
#4387=VECTOR('',#31074,1.5);
#4388=VECTOR('',#31077,10.);
#4389=VECTOR('',#31082,10.);
#4390=VECTOR('',#31089,10.);
#4391=VECTOR('',#31092,10.);
#4392=VECTOR('',#31101,10.);
#4393=VECTOR('',#31102,56.5);
#4394=VECTOR('',#31103,10.);
#4395=VECTOR('',#31106,10.);
#4396=VECTOR('',#31117,10.);
#4397=VECTOR('',#31118,10.);
#4398=VECTOR('',#31121,10.);
#4399=VECTOR('',#31122,10.);
#4400=VECTOR('',#31139,10.);
#4401=VECTOR('',#31142,70.2);
#4402=VECTOR('',#31145,10.);
#4403=VECTOR('',#31156,5.5);
#4404=VECTOR('',#31159,5.5);
#4405=VECTOR('',#31162,5.5);
#4406=VECTOR('',#31165,5.5);
#4407=VECTOR('',#31170,75.05);
#4408=VECTOR('',#31177,10.);
#4409=VECTOR('',#31184,10.);
#4410=VECTOR('',#31191,10.);
#4411=VECTOR('',#31200,10.);
#4412=VECTOR('',#31207,10.);
#4413=VECTOR('',#31210,10.);
#4414=VECTOR('',#31211,10.);
#4415=VECTOR('',#31212,10.);
#4416=VECTOR('',#31215,10.);
#4417=VECTOR('',#31216,10.);
#4418=VECTOR('',#31219,10.);
#4419=VECTOR('',#31222,10.);
#4420=VECTOR('',#31225,10.);
#4421=VECTOR('',#31226,10.);
#4422=VECTOR('',#31227,10.);
#4423=VECTOR('',#31228,10.);
#4424=VECTOR('',#31229,10.);
#4425=VECTOR('',#31232,10.);
#4426=VECTOR('',#31237,10.);
#4427=VECTOR('',#31238,10.);
#4428=VECTOR('',#31239,10.);
#4429=VECTOR('',#31242,10.);
#4430=VECTOR('',#31243,10.);
#4431=VECTOR('',#31246,10.);
#4432=VECTOR('',#31247,10.);
#4433=VECTOR('',#31250,10.);
#4434=VECTOR('',#31251,10.);
#4435=VECTOR('',#31254,10.);
#4436=VECTOR('',#31255,10.);
#4437=VECTOR('',#31258,10.);
#4438=VECTOR('',#31259,10.);
#4439=VECTOR('',#31262,10.);
#4440=VECTOR('',#31263,10.);
#4441=VECTOR('',#31266,10.);
#4442=VECTOR('',#31267,10.);
#4443=VECTOR('',#31270,10.);
#4444=VECTOR('',#31273,10.);
#4445=VECTOR('',#31274,10.);
#4446=VECTOR('',#31277,10.);
#4447=VECTOR('',#31280,10.);
#4448=VECTOR('',#31281,10.);
#4449=VECTOR('',#31282,10.);
#4450=VECTOR('',#31283,10.);
#4451=VECTOR('',#31284,10.);
#4452=VECTOR('',#31285,10.);
#4453=VECTOR('',#31286,10.);
#4454=VECTOR('',#31287,10.);
#4455=VECTOR('',#31288,10.);
#4456=VECTOR('',#31289,10.);
#4457=VECTOR('',#31290,10.);
#4458=VECTOR('',#31293,10.);
#4459=VECTOR('',#31296,10.);
#4460=VECTOR('',#31297,10.);
#4461=VECTOR('',#31300,10.);
#4462=VECTOR('',#31301,10.);
#4463=VECTOR('',#31302,10.);
#4464=VECTOR('',#31303,10.);
#4465=VECTOR('',#31304,10.);
#4466=VECTOR('',#31305,10.);
#4467=VECTOR('',#31306,10.);
#4468=VECTOR('',#31307,10.);
#4469=VECTOR('',#31308,10.);
#4470=VECTOR('',#31309,10.);
#4471=VECTOR('',#31310,10.);
#4472=VECTOR('',#31311,10.);
#4473=VECTOR('',#31312,10.);
#4474=VECTOR('',#31313,10.);
#4475=VECTOR('',#31316,10.);
#4476=VECTOR('',#31317,10.);
#4477=VECTOR('',#31318,10.);
#4478=VECTOR('',#31319,10.);
#4479=VECTOR('',#31320,10.);
#4480=VECTOR('',#31321,10.);
#4481=VECTOR('',#31322,10.);
#4482=VECTOR('',#31323,10.);
#4483=VECTOR('',#31324,10.);
#4484=VECTOR('',#31325,10.);
#4485=VECTOR('',#31326,10.);
#4486=VECTOR('',#31327,10.);
#4487=VECTOR('',#31328,10.);
#4488=VECTOR('',#31329,10.);
#4489=VECTOR('',#31330,10.);
#4490=VECTOR('',#31331,10.);
#4491=VECTOR('',#31332,10.);
#4492=VECTOR('',#31333,10.);
#4493=VECTOR('',#31334,10.);
#4494=VECTOR('',#31335,10.);
#4495=VECTOR('',#31338,10.);
#4496=VECTOR('',#31339,10.);
#4497=VECTOR('',#31340,10.);
#4498=VECTOR('',#31345,10.);
#4499=VECTOR('',#31346,10.);
#4500=VECTOR('',#31347,10.);
#4501=VECTOR('',#31348,10.);
#4502=VECTOR('',#31349,10.);
#4503=VECTOR('',#31350,10.);
#4504=VECTOR('',#31351,10.);
#4505=VECTOR('',#31354,10.);
#4506=VECTOR('',#31357,10.);
#4507=VECTOR('',#31358,10.);
#4508=VECTOR('',#31359,10.);
#4509=VECTOR('',#31360,10.);
#4510=VECTOR('',#31361,10.);
#4511=VECTOR('',#31362,10.);
#4512=VECTOR('',#31363,10.);
#4513=VECTOR('',#31364,10.);
#4514=VECTOR('',#31365,10.);
#4515=VECTOR('',#31368,10.);
#4516=VECTOR('',#31371,10.);
#4517=VECTOR('',#31372,10.);
#4518=VECTOR('',#31375,10.);
#4519=VECTOR('',#31380,10.);
#4520=VECTOR('',#31381,10.);
#4521=VECTOR('',#31382,10.);
#4522=VECTOR('',#31385,10.);
#4523=VECTOR('',#31386,10.);
#4524=VECTOR('',#31389,10.);
#4525=VECTOR('',#31390,10.);
#4526=VECTOR('',#31391,10.);
#4527=VECTOR('',#31392,10.);
#4528=VECTOR('',#31395,10.);
#4529=VECTOR('',#31396,10.);
#4530=VECTOR('',#31399,10.);
#4531=VECTOR('',#31400,10.);
#4532=VECTOR('',#31403,10.);
#4533=VECTOR('',#31404,10.);
#4534=VECTOR('',#31407,10.);
#4535=VECTOR('',#31408,10.);
#4536=VECTOR('',#31411,10.);
#4537=VECTOR('',#31412,10.);
#4538=VECTOR('',#31415,10.);
#4539=VECTOR('',#31420,5.5);
#4540=VECTOR('',#31423,5.5);
#4541=VECTOR('',#31426,5.5);
#4542=VECTOR('',#31429,5.5);
#4543=VECTOR('',#31434,10.);
#4544=VECTOR('',#31437,10.);
#4545=VECTOR('',#31440,10.);
#4546=VECTOR('',#31443,10.);
#4547=VECTOR('',#31454,26.26);
#4548=VECTOR('',#31461,26.01);
#4549=VECTOR('',#31466,10.);
#4550=VECTOR('',#31469,10.);
#4551=VECTOR('',#31472,10.);
#4552=VECTOR('',#31475,10.);
#4553=VECTOR('',#31478,26.26);
#4554=VECTOR('',#31489,7.25);
#4555=VECTOR('',#31496,10.);
#4556=VECTOR('',#31499,10.);
#4557=VECTOR('',#31502,10.);
#4558=VECTOR('',#31503,10.);
#4559=VECTOR('',#31504,10.);
#4560=VECTOR('',#31507,10.);
#4561=VECTOR('',#31510,10.);
#4562=VECTOR('',#31513,10.);
#4563=VECTOR('',#31516,10.);
#4564=VECTOR('',#31519,10.);
#4565=VECTOR('',#31524,7.);
#4566=VECTOR('',#31529,7.25);
#4567=VECTOR('',#31534,7.);
#4568=VECTOR('',#31539,10.);
#4569=VECTOR('',#31542,10.);
#4570=VECTOR('',#31547,10.);
#4571=VECTOR('',#31550,10.);
#4572=VECTOR('',#31551,10.);
#4573=VECTOR('',#31554,10.);
#4574=VECTOR('',#31557,10.);
#4575=VECTOR('',#31558,10.);
#4576=VECTOR('',#31559,10.);
#4577=VECTOR('',#31560,10.);
#4578=VECTOR('',#31561,10.);
#4579=VECTOR('',#31564,10.);
#4580=VECTOR('',#31567,10.);
#4581=VECTOR('',#31570,10.);
#4582=VECTOR('',#31577,2.55);
#4583=VECTOR('',#31580,10.);
#4584=VECTOR('',#31585,10.);
#4585=VECTOR('',#31588,10.);
#4586=VECTOR('',#31595,2.55);
#4587=VECTOR('',#31598,10.);
#4588=VECTOR('',#31601,10.);
#4589=VECTOR('',#31606,2.55);
#4590=VECTOR('',#31609,10.);
#4591=VECTOR('',#31614,10.);
#4592=VECTOR('',#31619,2.55);
#4593=VECTOR('',#31624,2.8);
#4594=VECTOR('',#31627,10.);
#4595=VECTOR('',#31628,10.);
#4596=VECTOR('',#31629,10.);
#4597=VECTOR('',#31630,10.);
#4598=VECTOR('',#31635,10.);
#4599=VECTOR('',#31638,10.);
#4600=VECTOR('',#31641,10.);
#4601=VECTOR('',#31644,10.);
#4602=VECTOR('',#31651,2.8);
#4603=VECTOR('',#31654,2.8);
#4604=VECTOR('',#31657,2.8);
#4605=VECTOR('',#31662,7.25);
#4606=VECTOR('',#31681,7.);
#4607=VECTOR('',#31684,7.25);
#4608=VECTOR('',#31691,7.);
#4609=VECTOR('',#31694,7.25000000000001);
#4610=VECTOR('',#31701,7.);
#4611=VECTOR('',#31704,7.25);
#4612=VECTOR('',#31711,6.99999999999999);
#4613=VECTOR('',#31716,7.25);
#4614=VECTOR('',#31719,10.);
#4615=VECTOR('',#31722,10.);
#4616=VECTOR('',#31725,10.);
#4617=VECTOR('',#31728,10.);
#4618=VECTOR('',#31735,7.25);
#4619=VECTOR('',#31746,70.);
#4620=VECTOR('',#31789,121.5);
#4621=VECTOR('',#31796,124.5);
#4622=VECTOR('',#31805,91.5);
#4623=VECTOR('',#31822,10.);
#4624=VECTOR('',#31829,10.);
#4625=VECTOR('',#31842,10.);
#4626=VECTOR('',#31851,10.);
#4627=VECTOR('',#31860,10.);
#4628=VECTOR('',#31869,10.);
#4629=VECTOR('',#31874,10.);
#4630=VECTOR('',#31875,10.);
#4631=VECTOR('',#31878,10.);
#4632=VECTOR('',#31881,10.);
#4633=VECTOR('',#31884,10.);
#4634=VECTOR('',#31893,125.);
#4635=VECTOR('',#31894,10.);
#4636=VECTOR('',#31911,10.);
#4637=VECTOR('',#31914,10.);
#4638=VECTOR('',#31917,10.);
#4639=VECTOR('',#31920,10.);
#4640=VECTOR('',#31923,10.);
#4641=VECTOR('',#31926,10.);
#4642=VECTOR('',#31933,45.);
#4643=VECTOR('',#31946,90.1);
#4644=VECTOR('',#31959,10.);
#4645=VECTOR('',#31962,10.);
#4646=VECTOR('',#31975,10.);
#4647=VECTOR('',#31976,10.);
#4648=VECTOR('',#31989,10.);
#4649=VECTOR('',#31990,10.);
#4650=VECTOR('',#32003,10.);
#4651=VECTOR('',#32004,10.);
#4652=VECTOR('',#32013,10.);
#4653=VECTOR('',#32016,10.);
#4654=VECTOR('',#32019,10.);
#4655=VECTOR('',#32020,10.);
#4656=VECTOR('',#32023,10.);
#4657=VECTOR('',#32028,10.);
#4658=VECTOR('',#32029,10.);
#4659=VECTOR('',#32032,10.);
#4660=VECTOR('',#32033,10.);
#4661=VECTOR('',#32034,10.);
#4662=VECTOR('',#32041,10.);
#4663=VECTOR('',#32054,10.);
#4664=VECTOR('',#32055,10.);
#4665=VECTOR('',#32068,10.);
#4666=VECTOR('',#32069,10.);
#4667=VECTOR('',#32080,10.);
#4668=VECTOR('',#32087,10.);
#4669=VECTOR('',#32088,10.);
#4670=VECTOR('',#32091,10.);
#4671=VECTOR('',#32096,10.);
#4672=VECTOR('',#32097,10.);
#4673=VECTOR('',#32104,10.);
#4674=VECTOR('',#32117,10.);
#4675=VECTOR('',#32118,10.);
#4676=VECTOR('',#32131,10.);
#4677=VECTOR('',#32144,10.);
#4678=VECTOR('',#32145,10.);
#4679=VECTOR('',#32154,10.);
#4680=VECTOR('',#32157,10.);
#4681=VECTOR('',#32160,10.);
#4682=VECTOR('',#32163,10.);
#4683=VECTOR('',#32166,10.);
#4684=VECTOR('',#32179,10.);
#4685=VECTOR('',#32192,10.);
#4686=VECTOR('',#32203,10.);
#4687=VECTOR('',#32214,10.);
#4688=VECTOR('',#32221,10.);
#4689=VECTOR('',#32224,10.);
#4690=VECTOR('',#32227,10.);
#4691=VECTOR('',#32228,10.);
#4692=VECTOR('',#32231,10.);
#4693=VECTOR('',#32236,10.);
#4694=VECTOR('',#32237,10.);
#4695=VECTOR('',#32254,10.);
#4696=VECTOR('',#32265,10.);
#4697=VECTOR('',#32278,10.);
#4698=VECTOR('',#32279,10.);
#4699=VECTOR('',#32282,10.);
#4700=VECTOR('',#32295,5.5);
#4701=VECTOR('',#32298,5.5);
#4702=VECTOR('',#32301,5.5);
#4703=VECTOR('',#32304,5.5);
#4704=VECTOR('',#32317,27.5);
#4705=VECTOR('',#32326,26.01);
#4706=VECTOR('',#32329,10.);
#4707=VECTOR('',#32332,10.);
#4708=VECTOR('',#32337,10.);
#4709=VECTOR('',#32342,10.);
#4710=VECTOR('',#32345,10.);
#4711=VECTOR('',#32348,10.);
#4712=VECTOR('',#32353,10.);
#4713=VECTOR('',#32354,10.);
#4714=VECTOR('',#32357,10.);
#4715=VECTOR('',#32360,10.);
#4716=VECTOR('',#32363,10.);
#4717=VECTOR('',#32366,10.);
#4718=VECTOR('',#32369,10.);
#4719=VECTOR('',#32372,10.);
#4720=VECTOR('',#32377,10.);
#4721=VECTOR('',#32378,10.);
#4722=VECTOR('',#32385,22.5);
#4723=VECTOR('',#32388,42.5);
#4724=VECTOR('',#32395,10.);
#4725=VECTOR('',#32396,10.);
#4726=VECTOR('',#32397,10.);
#4727=VECTOR('',#32400,10.);
#4728=VECTOR('',#32401,10.);
#4729=VECTOR('',#32402,10.);
#4730=VECTOR('',#32409,10.);
#4731=VECTOR('',#32412,10.);
#4732=VECTOR('',#32419,10.);
#4733=VECTOR('',#32422,10.);
#4734=VECTOR('',#32427,70.);
#4735=VECTOR('',#32432,10.);
#4736=VECTOR('',#32435,10.);
#4737=VECTOR('',#32442,10.);
#4738=VECTOR('',#32445,10.);
#4739=VECTOR('',#32452,10.);
#4740=VECTOR('',#32455,10.);
#4741=VECTOR('',#32462,10.);
#4742=VECTOR('',#32465,10.);
#4743=VECTOR('',#32472,10.);
#4744=VECTOR('',#32475,10.);
#4745=VECTOR('',#32482,10.);
#4746=VECTOR('',#32485,10.);
#4747=VECTOR('',#32492,10.);
#4748=VECTOR('',#32495,10.);
#4749=VECTOR('',#32502,10.);
#4750=VECTOR('',#32505,10.);
#4751=VECTOR('',#32512,10.);
#4752=VECTOR('',#32515,10.);
#4753=VECTOR('',#32522,10.);
#4754=VECTOR('',#32525,10.);
#4755=VECTOR('',#32532,10.);
#4756=VECTOR('',#32535,10.);
#4757=VECTOR('',#32542,10.);
#4758=VECTOR('',#32545,10.);
#4759=VECTOR('',#32552,10.);
#4760=VECTOR('',#32555,10.);
#4761=VECTOR('',#32562,10.);
#4762=VECTOR('',#32565,10.);
#4763=VECTOR('',#32572,10.);
#4764=VECTOR('',#32575,10.);
#4765=VECTOR('',#32582,10.);
#4766=VECTOR('',#32585,10.);
#4767=VECTOR('',#32592,10.);
#4768=VECTOR('',#32595,10.);
#4769=VECTOR('',#32602,10.);
#4770=VECTOR('',#32605,10.);
#4771=VECTOR('',#32612,10.);
#4772=VECTOR('',#32615,10.);
#4773=VECTOR('',#32622,10.);
#4774=VECTOR('',#32625,10.);
#4775=VECTOR('',#32632,10.);
#4776=VECTOR('',#32635,10.);
#4777=VECTOR('',#32642,10.);
#4778=VECTOR('',#32645,10.);
#4779=VECTOR('',#32652,10.);
#4780=VECTOR('',#32655,10.);
#4781=VECTOR('',#32662,10.);
#4782=VECTOR('',#32665,10.);
#4783=VECTOR('',#32672,10.);
#4784=VECTOR('',#32675,10.);
#4785=VECTOR('',#32682,10.);
#4786=VECTOR('',#32685,10.);
#4787=VECTOR('',#32692,10.);
#4788=VECTOR('',#32695,10.);
#4789=VECTOR('',#32702,10.);
#4790=VECTOR('',#32705,10.);
#4791=VECTOR('',#32712,10.);
#4792=VECTOR('',#32715,10.);
#4793=VECTOR('',#32722,10.);
#4794=VECTOR('',#32725,10.);
#4795=VECTOR('',#32734,10.);
#4796=VECTOR('',#32737,10.);
#4797=VECTOR('',#32744,10.);
#4798=VECTOR('',#32747,10.);
#4799=VECTOR('',#32754,10.);
#4800=VECTOR('',#32757,10.);
#4801=VECTOR('',#32764,10.);
#4802=VECTOR('',#32767,10.);
#4803=VECTOR('',#32774,10.);
#4804=VECTOR('',#32777,10.);
#4805=VECTOR('',#32784,10.);
#4806=VECTOR('',#32787,10.);
#4807=VECTOR('',#32794,10.);
#4808=VECTOR('',#32797,10.);
#4809=VECTOR('',#32804,10.);
#4810=VECTOR('',#32807,10.);
#4811=VECTOR('',#32814,10.);
#4812=VECTOR('',#32817,10.);
#4813=VECTOR('',#32824,10.);
#4814=VECTOR('',#32827,10.);
#4815=VECTOR('',#32834,10.);
#4816=VECTOR('',#32837,10.);
#4817=VECTOR('',#32844,10.);
#4818=VECTOR('',#32847,10.);
#4819=VECTOR('',#32854,10.);
#4820=VECTOR('',#32857,10.);
#4821=VECTOR('',#32864,10.);
#4822=VECTOR('',#32867,10.);
#4823=VECTOR('',#32874,10.);
#4824=VECTOR('',#32877,10.);
#4825=VECTOR('',#32884,10.);
#4826=VECTOR('',#32887,10.);
#4827=VECTOR('',#32894,10.);
#4828=VECTOR('',#32897,10.);
#4829=VECTOR('',#32904,10.);
#4830=VECTOR('',#32907,10.);
#4831=VECTOR('',#32914,10.);
#4832=VECTOR('',#32917,10.);
#4833=VECTOR('',#32924,10.);
#4834=VECTOR('',#32927,10.);
#4835=VECTOR('',#32934,10.);
#4836=VECTOR('',#32937,10.);
#4837=VECTOR('',#32944,10.);
#4838=VECTOR('',#32947,10.);
#4839=VECTOR('',#32954,10.);
#4840=VECTOR('',#32957,10.);
#4841=VECTOR('',#32964,10.);
#4842=VECTOR('',#32967,10.);
#4843=VECTOR('',#32974,10.);
#4844=VECTOR('',#32977,10.);
#4845=VECTOR('',#32984,10.);
#4846=VECTOR('',#32987,10.);
#4847=VECTOR('',#32994,10.);
#4848=VECTOR('',#32997,10.);
#4849=VECTOR('',#33004,10.);
#4850=VECTOR('',#33009,10.);
#4851=VECTOR('',#33010,10.);
#4852=VECTOR('',#33011,10.);
#4853=VECTOR('',#33014,10.);
#4854=VECTOR('',#33015,10.);
#4855=VECTOR('',#33016,10.);
#4856=VECTOR('',#33019,10.);
#4857=VECTOR('',#33020,10.);
#4858=VECTOR('',#33023,10.);
#4859=VECTOR('',#33024,10.);
#4860=VECTOR('',#33027,10.);
#4861=VECTOR('',#33028,10.);
#4862=VECTOR('',#33031,10.);
#4863=VECTOR('',#33034,10.);
#4864=VECTOR('',#33035,10.);
#4865=VECTOR('',#33036,10.);
#4866=VECTOR('',#33039,10.);
#4867=VECTOR('',#33040,10.);
#4868=VECTOR('',#33041,10.);
#4869=VECTOR('',#33044,10.);
#4870=VECTOR('',#33045,10.);
#4871=VECTOR('',#33048,10.);
#4872=VECTOR('',#33049,10.);
#4873=VECTOR('',#33052,10.);
#4874=VECTOR('',#33053,10.);
#4875=VECTOR('',#33056,10.);
#4876=VECTOR('',#33059,10.);
#4877=VECTOR('',#33060,10.);
#4878=VECTOR('',#33061,10.);
#4879=VECTOR('',#33064,10.);
#4880=VECTOR('',#33065,10.);
#4881=VECTOR('',#33066,10.);
#4882=VECTOR('',#33069,10.);
#4883=VECTOR('',#33070,10.);
#4884=VECTOR('',#33073,10.);
#4885=VECTOR('',#33074,10.);
#4886=VECTOR('',#33077,10.);
#4887=VECTOR('',#33078,10.);
#4888=VECTOR('',#33081,10.);
#4889=VECTOR('',#33084,10.);
#4890=VECTOR('',#33085,10.);
#4891=VECTOR('',#33086,10.);
#4892=VECTOR('',#33089,10.);
#4893=VECTOR('',#33090,10.);
#4894=VECTOR('',#33091,10.);
#4895=VECTOR('',#33094,10.);
#4896=VECTOR('',#33095,10.);
#4897=VECTOR('',#33098,10.);
#4898=VECTOR('',#33099,10.);
#4899=VECTOR('',#33102,10.);
#4900=VECTOR('',#33103,10.);
#4901=VECTOR('',#33106,10.);
#4902=VECTOR('',#33107,10.);
#4903=VECTOR('',#33108,10.);
#4904=VECTOR('',#33109,10.);
#4905=VECTOR('',#33110,10.);
#4906=VECTOR('',#33111,10.);
#4907=VECTOR('',#33112,10.);
#4908=VECTOR('',#33113,10.);
#4909=VECTOR('',#33114,10.);
#4910=VECTOR('',#33115,10.);
#4911=VECTOR('',#33116,10.);
#4912=VECTOR('',#33117,10.);
#4913=VECTOR('',#33118,10.);
#4914=VECTOR('',#33119,10.);
#4915=VECTOR('',#33120,10.);
#4916=VECTOR('',#33121,10.);
#4917=VECTOR('',#33122,10.);
#4918=VECTOR('',#33123,10.);
#4919=VECTOR('',#33124,10.);
#4920=VECTOR('',#33125,10.);
#4921=VECTOR('',#33126,10.);
#4922=VECTOR('',#33127,10.);
#4923=VECTOR('',#33128,10.);
#4924=VECTOR('',#33129,10.);
#4925=VECTOR('',#33130,10.);
#4926=VECTOR('',#33131,10.);
#4927=VECTOR('',#33132,10.);
#4928=VECTOR('',#33133,10.);
#4929=VECTOR('',#33134,10.);
#4930=VECTOR('',#33135,10.);
#4931=VECTOR('',#33136,10.);
#4932=VECTOR('',#33137,10.);
#4933=VECTOR('',#33138,10.);
#4934=VECTOR('',#33139,10.);
#4935=VECTOR('',#33140,10.);
#4936=VECTOR('',#33141,10.);
#4937=VECTOR('',#33142,10.);
#4938=VECTOR('',#33143,10.);
#4939=VECTOR('',#33144,10.);
#4940=VECTOR('',#33145,10.);
#4941=VECTOR('',#33146,10.);
#4942=VECTOR('',#33147,10.);
#4943=VECTOR('',#33148,10.);
#4944=VECTOR('',#33149,10.);
#4945=VECTOR('',#33150,10.);
#4946=VECTOR('',#33151,10.);
#4947=VECTOR('',#33152,10.);
#4948=VECTOR('',#33153,10.);
#4949=VECTOR('',#33154,10.);
#4950=VECTOR('',#33155,10.);
#4951=VECTOR('',#33156,10.);
#4952=VECTOR('',#33157,10.);
#4953=VECTOR('',#33158,10.);
#4954=VECTOR('',#33159,10.);
#4955=VECTOR('',#33160,10.);
#4956=VECTOR('',#33161,10.);
#4957=VECTOR('',#33162,10.);
#4958=VECTOR('',#33163,10.);
#4959=VECTOR('',#33164,10.);
#4960=VECTOR('',#33165,10.);
#4961=VECTOR('',#33166,10.);
#4962=VECTOR('',#33167,10.);
#4963=VECTOR('',#33168,10.);
#4964=VECTOR('',#33169,10.);
#4965=VECTOR('',#33170,10.);
#4966=VECTOR('',#33171,10.);
#4967=VECTOR('',#33172,10.);
#4968=VECTOR('',#33173,10.);
#4969=VECTOR('',#33174,10.);
#4970=VECTOR('',#33175,10.);
#4971=VECTOR('',#33176,10.);
#4972=VECTOR('',#33177,10.);
#4973=VECTOR('',#33178,10.);
#4974=VECTOR('',#33179,10.);
#4975=VECTOR('',#33180,10.);
#4976=VECTOR('',#33181,10.);
#4977=VECTOR('',#33182,10.);
#4978=VECTOR('',#33183,10.);
#4979=VECTOR('',#33186,10.);
#4980=VECTOR('',#33187,10.);
#4981=VECTOR('',#33188,10.);
#4982=VECTOR('',#33191,10.);
#4983=VECTOR('',#33192,10.);
#4984=VECTOR('',#33195,10.);
#4985=VECTOR('',#33196,10.);
#4986=VECTOR('',#33199,10.);
#4987=VECTOR('',#33200,10.);
#4988=VECTOR('',#33203,10.);
#4989=VECTOR('',#33206,10.);
#4990=VECTOR('',#33207,10.);
#4991=VECTOR('',#33210,10.);
#4992=VECTOR('',#33211,10.);
#4993=VECTOR('',#33214,10.);
#4994=VECTOR('',#33217,10.);
#4995=VECTOR('',#33218,10.);
#4996=VECTOR('',#33221,10.);
#4997=VECTOR('',#33222,10.);
#4998=VECTOR('',#33225,10.);
#4999=VECTOR('',#33228,10.);
#5000=VECTOR('',#33229,10.);
#5001=VECTOR('',#33232,10.);
#5002=VECTOR('',#33233,10.);
#5003=VECTOR('',#33236,10.);
#5004=VECTOR('',#33239,10.);
#5005=VECTOR('',#33240,10.);
#5006=VECTOR('',#33243,10.);
#5007=VECTOR('',#33244,10.);
#5008=VECTOR('',#33247,10.);
#5009=VECTOR('',#33250,10.);
#5010=VECTOR('',#33251,10.);
#5011=VECTOR('',#33254,10.);
#5012=VECTOR('',#33255,10.);
#5013=VECTOR('',#33258,10.);
#5014=VECTOR('',#33261,10.);
#5015=VECTOR('',#33262,10.);
#5016=VECTOR('',#33265,10.);
#5017=VECTOR('',#33266,10.);
#5018=VECTOR('',#33269,10.);
#5019=VECTOR('',#33272,10.);
#5020=VECTOR('',#33273,10.);
#5021=VECTOR('',#33276,10.);
#5022=VECTOR('',#33277,10.);
#5023=VECTOR('',#33280,10.);
#5024=VECTOR('',#33283,10.);
#5025=VECTOR('',#33284,10.);
#5026=VECTOR('',#33287,10.);
#5027=VECTOR('',#33288,10.);
#5028=VECTOR('',#33291,10.);
#5029=VECTOR('',#33294,10.);
#5030=VECTOR('',#33295,10.);
#5031=VECTOR('',#33298,10.);
#5032=VECTOR('',#33299,10.);
#5033=VECTOR('',#33302,10.);
#5034=VECTOR('',#33305,10.);
#5035=VECTOR('',#33306,10.);
#5036=VECTOR('',#33309,10.);
#5037=VECTOR('',#33310,10.);
#5038=VECTOR('',#33313,10.);
#5039=VECTOR('',#33316,10.);
#5040=VECTOR('',#33317,10.);
#5041=VECTOR('',#33320,10.);
#5042=VECTOR('',#33321,10.);
#5043=VECTOR('',#33324,10.);
#5044=VECTOR('',#33327,10.);
#5045=VECTOR('',#33328,10.);
#5046=VECTOR('',#33331,10.);
#5047=VECTOR('',#33332,10.);
#5048=VECTOR('',#33335,10.);
#5049=VECTOR('',#33338,10.);
#5050=VECTOR('',#33339,10.);
#5051=VECTOR('',#33342,10.);
#5052=VECTOR('',#33343,10.);
#5053=VECTOR('',#33346,10.);
#5054=VECTOR('',#33349,10.);
#5055=VECTOR('',#33350,10.);
#5056=VECTOR('',#33353,10.);
#5057=VECTOR('',#33354,10.);
#5058=VECTOR('',#33357,10.);
#5059=VECTOR('',#33360,10.);
#5060=VECTOR('',#33361,10.);
#5061=VECTOR('',#33364,10.);
#5062=VECTOR('',#33365,10.);
#5063=VECTOR('',#33368,10.);
#5064=VECTOR('',#33371,10.);
#5065=VECTOR('',#33372,10.);
#5066=VECTOR('',#33375,10.);
#5067=VECTOR('',#33376,10.);
#5068=VECTOR('',#33379,10.);
#5069=VECTOR('',#33382,10.);
#5070=VECTOR('',#33383,10.);
#5071=VECTOR('',#33386,10.);
#5072=VECTOR('',#33387,10.);
#5073=VECTOR('',#33390,10.);
#5074=VECTOR('',#33393,10.);
#5075=VECTOR('',#33394,10.);
#5076=VECTOR('',#33397,10.);
#5077=VECTOR('',#33398,10.);
#5078=VECTOR('',#33401,10.);
#5079=VECTOR('',#33404,10.);
#5080=VECTOR('',#33405,10.);
#5081=VECTOR('',#33408,10.);
#5082=VECTOR('',#33409,10.);
#5083=VECTOR('',#33412,10.);
#5084=VECTOR('',#33413,10.);
#5085=VECTOR('',#33416,10.);
#5086=VECTOR('',#33419,10.);
#5087=VECTOR('',#33420,10.);
#5088=VECTOR('',#33423,10.);
#5089=VECTOR('',#33426,10.);
#5090=VECTOR('',#33427,10.);
#5091=VECTOR('',#33430,10.);
#5092=VECTOR('',#33431,10.);
#5093=VECTOR('',#33434,10.);
#5094=VECTOR('',#33437,10.);
#5095=VECTOR('',#33438,10.);
#5096=VECTOR('',#33441,10.);
#5097=VECTOR('',#33442,10.);
#5098=VECTOR('',#33445,10.);
#5099=VECTOR('',#33448,10.);
#5100=VECTOR('',#33449,10.);
#5101=VECTOR('',#33452,10.);
#5102=VECTOR('',#33453,10.);
#5103=VECTOR('',#33456,10.);
#5104=VECTOR('',#33459,10.);
#5105=VECTOR('',#33460,10.);
#5106=VECTOR('',#33463,10.);
#5107=VECTOR('',#33464,10.);
#5108=VECTOR('',#33467,10.);
#5109=VECTOR('',#33470,10.);
#5110=VECTOR('',#33471,10.);
#5111=VECTOR('',#33474,10.);
#5112=VECTOR('',#33475,10.);
#5113=VECTOR('',#33478,10.);
#5114=VECTOR('',#33481,10.);
#5115=VECTOR('',#33482,10.);
#5116=VECTOR('',#33485,10.);
#5117=VECTOR('',#33486,10.);
#5118=VECTOR('',#33489,10.);
#5119=VECTOR('',#33492,10.);
#5120=VECTOR('',#33493,10.);
#5121=VECTOR('',#33496,10.);
#5122=VECTOR('',#33497,10.);
#5123=VECTOR('',#33500,10.);
#5124=VECTOR('',#33503,10.);
#5125=VECTOR('',#33504,10.);
#5126=VECTOR('',#33507,10.);
#5127=VECTOR('',#33508,10.);
#5128=VECTOR('',#33511,10.);
#5129=VECTOR('',#33514,10.);
#5130=VECTOR('',#33515,10.);
#5131=VECTOR('',#33518,10.);
#5132=VECTOR('',#33519,10.);
#5133=VECTOR('',#33522,10.);
#5134=VECTOR('',#33525,10.);
#5135=VECTOR('',#33526,10.);
#5136=VECTOR('',#33529,10.);
#5137=VECTOR('',#33530,10.);
#5138=VECTOR('',#33533,10.);
#5139=VECTOR('',#33536,10.);
#5140=VECTOR('',#33537,10.);
#5141=VECTOR('',#33540,10.);
#5142=VECTOR('',#33541,10.);
#5143=VECTOR('',#33544,10.);
#5144=VECTOR('',#33547,10.);
#5145=VECTOR('',#33548,10.);
#5146=VECTOR('',#33551,10.);
#5147=VECTOR('',#33552,10.);
#5148=VECTOR('',#33555,10.);
#5149=VECTOR('',#33558,10.);
#5150=VECTOR('',#33559,10.);
#5151=VECTOR('',#33562,10.);
#5152=VECTOR('',#33563,10.);
#5153=VECTOR('',#33566,10.);
#5154=VECTOR('',#33569,10.);
#5155=VECTOR('',#33570,10.);
#5156=VECTOR('',#33573,10.);
#5157=VECTOR('',#33574,10.);
#5158=VECTOR('',#33577,10.);
#5159=VECTOR('',#33580,10.);
#5160=VECTOR('',#33581,10.);
#5161=VECTOR('',#33584,10.);
#5162=VECTOR('',#33585,10.);
#5163=VECTOR('',#33588,10.);
#5164=VECTOR('',#33591,10.);
#5165=VECTOR('',#33592,10.);
#5166=VECTOR('',#33595,10.);
#5167=VECTOR('',#33596,10.);
#5168=VECTOR('',#33599,10.);
#5169=VECTOR('',#33602,10.);
#5170=VECTOR('',#33603,10.);
#5171=VECTOR('',#33606,10.);
#5172=VECTOR('',#33607,10.);
#5173=VECTOR('',#33610,10.);
#5174=VECTOR('',#33613,10.);
#5175=VECTOR('',#33614,10.);
#5176=VECTOR('',#33617,10.);
#5177=VECTOR('',#33618,10.);
#5178=VECTOR('',#33621,10.);
#5179=VECTOR('',#33624,10.);
#5180=VECTOR('',#33625,10.);
#5181=VECTOR('',#33628,10.);
#5182=VECTOR('',#33629,10.);
#5183=VECTOR('',#33632,10.);
#5184=VECTOR('',#33635,10.);
#5185=VECTOR('',#33636,10.);
#5186=VECTOR('',#33639,10.);
#5187=VECTOR('',#33640,10.);
#5188=VECTOR('',#33643,10.);
#5189=VECTOR('',#33646,10.);
#5190=VECTOR('',#33647,10.);
#5191=VECTOR('',#33650,10.);
#5192=VECTOR('',#33651,10.);
#5193=VECTOR('',#33654,10.);
#5194=VECTOR('',#33657,10.);
#5195=VECTOR('',#33658,10.);
#5196=VECTOR('',#33661,10.);
#5197=VECTOR('',#33662,10.);
#5198=VECTOR('',#33665,10.);
#5199=VECTOR('',#33668,10.);
#5200=VECTOR('',#33669,10.);
#5201=VECTOR('',#33672,10.);
#5202=VECTOR('',#33673,10.);
#5203=VECTOR('',#33676,10.);
#5204=VECTOR('',#33679,10.);
#5205=VECTOR('',#33680,10.);
#5206=VECTOR('',#33683,10.);
#5207=VECTOR('',#33684,10.);
#5208=VECTOR('',#33687,10.);
#5209=VECTOR('',#33690,10.);
#5210=VECTOR('',#33691,10.);
#5211=VECTOR('',#33692,10.);
#5212=VECTOR('',#33693,10.);
#5213=VECTOR('',#33696,10.);
#5214=VECTOR('',#33697,10.);
#5215=VECTOR('',#33700,10.);
#5216=VECTOR('',#33701,10.);
#5217=VECTOR('',#33702,10.);
#5218=VECTOR('',#33703,10.);
#5219=VECTOR('',#33704,10.);
#5220=VECTOR('',#33705,10.);
#5221=VECTOR('',#33706,10.);
#5222=VECTOR('',#33707,10.);
#5223=VECTOR('',#33708,10.);
#5224=VECTOR('',#33709,10.);
#5225=VECTOR('',#33710,10.);
#5226=VECTOR('',#33711,10.);
#5227=VECTOR('',#33712,10.);
#5228=VECTOR('',#33713,10.);
#5229=VECTOR('',#33714,10.);
#5230=VECTOR('',#33715,10.);
#5231=VECTOR('',#33716,10.);
#5232=VECTOR('',#33717,10.);
#5233=VECTOR('',#33718,10.);
#5234=VECTOR('',#33719,10.);
#5235=VECTOR('',#33720,10.);
#5236=VECTOR('',#33721,10.);
#5237=VECTOR('',#33722,10.);
#5238=VECTOR('',#33723,10.);
#5239=VECTOR('',#33724,10.);
#5240=VECTOR('',#33725,10.);
#5241=VECTOR('',#33726,10.);
#5242=VECTOR('',#33727,10.);
#5243=VECTOR('',#33728,10.);
#5244=VECTOR('',#33729,10.);
#5245=VECTOR('',#33730,10.);
#5246=VECTOR('',#33731,10.);
#5247=VECTOR('',#33732,10.);
#5248=VECTOR('',#33733,10.);
#5249=VECTOR('',#33734,10.);
#5250=VECTOR('',#33735,10.);
#5251=VECTOR('',#33736,10.);
#5252=VECTOR('',#33737,10.);
#5253=VECTOR('',#33738,10.);
#5254=VECTOR('',#33739,10.);
#5255=VECTOR('',#33740,10.);
#5256=VECTOR('',#33741,10.);
#5257=VECTOR('',#33742,10.);
#5258=VECTOR('',#33743,10.);
#5259=VECTOR('',#33744,10.);
#5260=VECTOR('',#33745,10.);
#5261=VECTOR('',#33746,10.);
#5262=VECTOR('',#33747,10.);
#5263=VECTOR('',#33748,10.);
#5264=VECTOR('',#33749,10.);
#5265=VECTOR('',#33750,10.);
#5266=VECTOR('',#33751,10.);
#5267=VECTOR('',#33752,10.);
#5268=VECTOR('',#33753,10.);
#5269=VECTOR('',#33754,10.);
#5270=VECTOR('',#33755,10.);
#5271=VECTOR('',#33756,10.);
#5272=VECTOR('',#33757,10.);
#5273=VECTOR('',#33758,10.);
#5274=VECTOR('',#33759,10.);
#5275=VECTOR('',#33760,10.);
#5276=VECTOR('',#33761,10.);
#5277=VECTOR('',#33762,10.);
#5278=VECTOR('',#33763,10.);
#5279=VECTOR('',#33764,10.);
#5280=VECTOR('',#33765,10.);
#5281=VECTOR('',#33766,10.);
#5282=VECTOR('',#33767,10.);
#5283=VECTOR('',#33768,10.);
#5284=VECTOR('',#33769,10.);
#5285=VECTOR('',#33770,10.);
#5286=VECTOR('',#33771,10.);
#5287=VECTOR('',#33772,10.);
#5288=VECTOR('',#33773,10.);
#5289=VECTOR('',#33774,10.);
#5290=VECTOR('',#33775,10.);
#5291=VECTOR('',#33776,10.);
#5292=VECTOR('',#33777,10.);
#5293=VECTOR('',#33778,10.);
#5294=VECTOR('',#33779,10.);
#5295=VECTOR('',#33780,10.);
#5296=VECTOR('',#33781,10.);
#5297=VECTOR('',#33782,10.);
#5298=VECTOR('',#33783,10.);
#5299=VECTOR('',#33784,10.);
#5300=VECTOR('',#33785,10.);
#5301=VECTOR('',#33786,10.);
#5302=VECTOR('',#33787,10.);
#5303=VECTOR('',#33788,10.);
#5304=VECTOR('',#33789,10.);
#5305=VECTOR('',#33790,10.);
#5306=VECTOR('',#33793,10.);
#5307=VECTOR('',#33794,10.);
#5308=VECTOR('',#33795,10.);
#5309=VECTOR('',#33800,10.);
#5310=VECTOR('',#33803,10.);
#5311=VECTOR('',#33804,10.);
#5312=VECTOR('',#33805,10.);
#5313=VECTOR('',#33808,10.);
#5314=VECTOR('',#33811,10.);
#5315=VECTOR('',#33814,10.);
#5316=VECTOR('',#33815,10.);
#5317=VECTOR('',#33816,10.);
#5318=VECTOR('',#33819,10.);
#5319=VECTOR('',#33822,10.);
#5320=VECTOR('',#33825,10.);
#5321=VECTOR('',#33826,10.);
#5322=VECTOR('',#33829,10.);
#5323=VECTOR('',#33830,10.);
#5324=VECTOR('',#33833,10.);
#5325=VECTOR('',#33834,10.);
#5326=VECTOR('',#33835,10.);
#5327=VECTOR('',#33838,10.);
#5328=VECTOR('',#33841,10.);
#5329=VECTOR('',#33844,10.);
#5330=VECTOR('',#33845,10.);
#5331=VECTOR('',#33846,10.);
#5332=VECTOR('',#33849,10.);
#5333=VECTOR('',#33852,10.);
#5334=VECTOR('',#33855,10.);
#5335=VECTOR('',#33856,10.);
#5336=VECTOR('',#33859,10.);
#5337=VECTOR('',#33860,10.);
#5338=VECTOR('',#33863,10.);
#5339=VECTOR('',#33864,10.);
#5340=VECTOR('',#33865,10.);
#5341=VECTOR('',#33868,10.);
#5342=VECTOR('',#33871,10.);
#5343=VECTOR('',#33874,10.);
#5344=VECTOR('',#33875,10.);
#5345=VECTOR('',#33876,10.);
#5346=VECTOR('',#33879,10.);
#5347=VECTOR('',#33882,10.);
#5348=VECTOR('',#33885,10.);
#5349=VECTOR('',#33886,10.);
#5350=VECTOR('',#33889,10.);
#5351=VECTOR('',#33890,10.);
#5352=VECTOR('',#33893,10.);
#5353=VECTOR('',#33894,10.);
#5354=VECTOR('',#33897,10.);
#5355=VECTOR('',#33898,10.);
#5356=VECTOR('',#33901,10.);
#5357=VECTOR('',#33904,10.);
#5358=VECTOR('',#33905,10.);
#5359=VECTOR('',#33906,10.);
#5360=VECTOR('',#33909,10.);
#5361=VECTOR('',#33912,10.);
#5362=VECTOR('',#33915,10.);
#5363=VECTOR('',#33916,10.);
#5364=VECTOR('',#33917,10.);
#5365=VECTOR('',#33920,10.);
#5366=VECTOR('',#33923,10.);
#5367=VECTOR('',#33926,10.);
#5368=VECTOR('',#33927,10.);
#5369=VECTOR('',#33930,10.);
#5370=VECTOR('',#33931,10.);
#5371=VECTOR('',#33934,10.);
#5372=VECTOR('',#33935,10.);
#5373=VECTOR('',#33936,10.);
#5374=VECTOR('',#33939,10.);
#5375=VECTOR('',#33942,10.);
#5376=VECTOR('',#33945,10.);
#5377=VECTOR('',#33946,10.);
#5378=VECTOR('',#33947,10.);
#5379=VECTOR('',#33950,10.);
#5380=VECTOR('',#33953,10.);
#5381=VECTOR('',#33956,10.);
#5382=VECTOR('',#33957,10.);
#5383=VECTOR('',#33960,10.);
#5384=VECTOR('',#33961,10.);
#5385=VECTOR('',#33964,10.);
#5386=VECTOR('',#33965,10.);
#5387=VECTOR('',#33966,10.);
#5388=VECTOR('',#33969,10.);
#5389=VECTOR('',#33972,10.);
#5390=VECTOR('',#33975,10.);
#5391=VECTOR('',#33976,10.);
#5392=VECTOR('',#33977,10.);
#5393=VECTOR('',#33980,10.);
#5394=VECTOR('',#33983,10.);
#5395=VECTOR('',#33986,10.);
#5396=VECTOR('',#33987,10.);
#5397=VECTOR('',#33990,10.);
#5398=VECTOR('',#33991,10.);
#5399=VECTOR('',#33994,10.);
#5400=VECTOR('',#33995,10.);
#5401=VECTOR('',#33996,10.);
#5402=VECTOR('',#33999,10.);
#5403=VECTOR('',#34002,10.);
#5404=VECTOR('',#34005,10.);
#5405=VECTOR('',#34006,10.);
#5406=VECTOR('',#34007,10.);
#5407=VECTOR('',#34010,10.);
#5408=VECTOR('',#34013,10.);
#5409=VECTOR('',#34016,10.);
#5410=VECTOR('',#34017,10.);
#5411=VECTOR('',#34020,10.);
#5412=VECTOR('',#34021,10.);
#5413=VECTOR('',#34024,10.);
#5414=VECTOR('',#34025,10.);
#5415=VECTOR('',#34026,10.);
#5416=VECTOR('',#34029,10.);
#5417=VECTOR('',#34032,10.);
#5418=VECTOR('',#34035,10.);
#5419=VECTOR('',#34036,10.);
#5420=VECTOR('',#34037,10.);
#5421=VECTOR('',#34040,10.);
#5422=VECTOR('',#34043,10.);
#5423=VECTOR('',#34046,10.);
#5424=VECTOR('',#34047,10.);
#5425=VECTOR('',#34050,10.);
#5426=VECTOR('',#34051,10.);
#5427=VECTOR('',#34054,10.);
#5428=VECTOR('',#34055,10.);
#5429=VECTOR('',#34056,10.);
#5430=VECTOR('',#34059,10.);
#5431=VECTOR('',#34062,10.);
#5432=VECTOR('',#34065,10.);
#5433=VECTOR('',#34066,10.);
#5434=VECTOR('',#34067,10.);
#5435=VECTOR('',#34070,10.);
#5436=VECTOR('',#34073,10.);
#5437=VECTOR('',#34076,10.);
#5438=VECTOR('',#34077,10.);
#5439=VECTOR('',#34080,10.);
#5440=VECTOR('',#34081,10.);
#5441=VECTOR('',#34084,10.);
#5442=VECTOR('',#34085,10.);
#5443=VECTOR('',#34086,10.);
#5444=VECTOR('',#34089,10.);
#5445=VECTOR('',#34092,10.);
#5446=VECTOR('',#34095,10.);
#5447=VECTOR('',#34096,10.);
#5448=VECTOR('',#34097,10.);
#5449=VECTOR('',#34100,10.);
#5450=VECTOR('',#34103,10.);
#5451=VECTOR('',#34106,10.);
#5452=VECTOR('',#34107,10.);
#5453=VECTOR('',#34108,10.);
#5454=VECTOR('',#34111,10.);
#5455=VECTOR('',#34114,10.);
#5456=VECTOR('',#34117,10.);
#5457=VECTOR('',#34118,10.);
#5458=VECTOR('',#34121,10.);
#5459=VECTOR('',#34122,10.);
#5460=VECTOR('',#34125,10.);
#5461=VECTOR('',#34126,10.);
#5462=VECTOR('',#34127,10.);
#5463=VECTOR('',#34130,10.);
#5464=VECTOR('',#34133,10.);
#5465=VECTOR('',#34136,10.);
#5466=VECTOR('',#34137,10.);
#5467=VECTOR('',#34138,10.);
#5468=VECTOR('',#34141,10.);
#5469=VECTOR('',#34144,10.);
#5470=VECTOR('',#34147,10.);
#5471=VECTOR('',#34148,10.);
#5472=VECTOR('',#34151,10.);
#5473=VECTOR('',#34152,10.);
#5474=VECTOR('',#34155,10.);
#5475=VECTOR('',#34156,10.);
#5476=VECTOR('',#34157,10.);
#5477=VECTOR('',#34160,10.);
#5478=VECTOR('',#34163,10.);
#5479=VECTOR('',#34166,10.);
#5480=VECTOR('',#34167,10.);
#5481=VECTOR('',#34168,10.);
#5482=VECTOR('',#34171,10.);
#5483=VECTOR('',#34174,10.);
#5484=VECTOR('',#34177,10.);
#5485=VECTOR('',#34178,10.);
#5486=VECTOR('',#34181,10.);
#5487=VECTOR('',#34182,10.);
#5488=VECTOR('',#34185,10.);
#5489=VECTOR('',#34186,10.);
#5490=VECTOR('',#34189,10.);
#5491=VECTOR('',#34190,10.);
#5492=VECTOR('',#34193,10.);
#5493=VECTOR('',#34196,10.);
#5494=VECTOR('',#34197,10.);
#5495=VECTOR('',#34198,10.);
#5496=VECTOR('',#34201,10.);
#5497=VECTOR('',#34204,10.);
#5498=VECTOR('',#34207,10.);
#5499=VECTOR('',#34208,10.);
#5500=VECTOR('',#34209,10.);
#5501=VECTOR('',#34212,10.);
#5502=VECTOR('',#34215,10.);
#5503=VECTOR('',#34218,10.);
#5504=VECTOR('',#34219,10.);
#5505=VECTOR('',#34222,10.);
#5506=VECTOR('',#34223,10.);
#5507=VECTOR('',#34226,10.);
#5508=VECTOR('',#34227,10.);
#5509=VECTOR('',#34228,10.);
#5510=VECTOR('',#34233,10.);
#5511=VECTOR('',#34236,10.);
#5512=VECTOR('',#34241,10.);
#5513=VECTOR('',#34242,10.);
#5514=VECTOR('',#34243,10.);
#5515=VECTOR('',#34246,10.);
#5516=VECTOR('',#34247,10.);
#5517=VECTOR('',#34250,10.);
#5518=VECTOR('',#34251,10.);
#5519=VECTOR('',#34256,10.);
#5520=VECTOR('',#34263,10.);
#5521=VECTOR('',#34264,10.);
#5522=VECTOR('',#34273,10.);
#5523=VECTOR('',#34276,10.);
#5524=VECTOR('',#34279,10.);
#5525=VECTOR('',#34280,10.);
#5526=VECTOR('',#34283,10.);
#5527=VECTOR('',#34286,10.);
#5528=VECTOR('',#34287,10.);
#5529=VECTOR('',#34288,10.);
#5530=VECTOR('',#34291,10.);
#5531=VECTOR('',#34292,10.);
#5532=VECTOR('',#34295,10.);
#5533=VECTOR('',#34300,10.);
#5534=VECTOR('',#34303,10.);
#5535=VECTOR('',#34310,10.);
#5536=VECTOR('',#34317,10.);
#5537=VECTOR('',#34318,10.);
#5538=VECTOR('',#34319,10.);
#5539=VECTOR('',#34322,10.);
#5540=VECTOR('',#34325,10.);
#5541=VECTOR('',#34332,10.);
#5542=VECTOR('',#34333,10.);
#5543=VECTOR('',#34334,10.);
#5544=VECTOR('',#34337,10.);
#5545=VECTOR('',#34340,10.);
#5546=VECTOR('',#34347,10.);
#5547=VECTOR('',#34354,10.);
#5548=VECTOR('',#34355,10.);
#5549=VECTOR('',#34356,10.);
#5550=VECTOR('',#34359,10.);
#5551=VECTOR('',#34362,10.);
#5552=VECTOR('',#34369,10.);
#5553=VECTOR('',#34376,10.);
#5554=VECTOR('',#34377,10.);
#5555=VECTOR('',#34378,10.);
#5556=VECTOR('',#34381,10.);
#5557=VECTOR('',#34384,10.);
#5558=VECTOR('',#34391,10.);
#5559=VECTOR('',#34398,10.);
#5560=VECTOR('',#34399,10.);
#5561=VECTOR('',#34400,10.);
#5562=VECTOR('',#34403,10.);
#5563=VECTOR('',#34406,10.);
#5564=VECTOR('',#34413,10.);
#5565=VECTOR('',#34414,10.);
#5566=VECTOR('',#34415,10.);
#5567=VECTOR('',#34418,10.);
#5568=VECTOR('',#34421,10.);
#5569=VECTOR('',#34428,10.);
#5570=VECTOR('',#34435,10.);
#5571=VECTOR('',#34436,10.);
#5572=VECTOR('',#34437,10.);
#5573=VECTOR('',#34440,10.);
#5574=VECTOR('',#34443,10.);
#5575=VECTOR('',#34450,10.);
#5576=VECTOR('',#34457,10.);
#5577=VECTOR('',#34458,10.);
#5578=VECTOR('',#34459,10.);
#5579=VECTOR('',#34462,10.);
#5580=VECTOR('',#34465,10.);
#5581=VECTOR('',#34472,10.);
#5582=VECTOR('',#34479,10.);
#5583=VECTOR('',#34480,10.);
#5584=VECTOR('',#34481,10.);
#5585=VECTOR('',#34484,10.);
#5586=VECTOR('',#34487,10.);
#5587=VECTOR('',#34494,10.);
#5588=VECTOR('',#34501,10.);
#5589=VECTOR('',#34502,10.);
#5590=VECTOR('',#34503,10.);
#5591=VECTOR('',#34506,10.);
#5592=VECTOR('',#34509,10.);
#5593=VECTOR('',#34516,10.);
#5594=VECTOR('',#34521,10.);
#5595=VECTOR('',#34526,10.);
#5596=VECTOR('',#34527,10.);
#5597=VECTOR('',#34528,10.);
#5598=VECTOR('',#34531,10.);
#5599=VECTOR('',#34534,10.);
#5600=VECTOR('',#34541,10.);
#5601=VECTOR('',#34548,10.);
#5602=VECTOR('',#34549,10.);
#5603=VECTOR('',#34550,10.);
#5604=VECTOR('',#34553,10.);
#5605=VECTOR('',#34556,10.);
#5606=VECTOR('',#34563,10.);
#5607=VECTOR('',#34564,10.);
#5608=VECTOR('',#34565,10.);
#5609=VECTOR('',#34568,10.);
#5610=VECTOR('',#34571,10.);
#5611=VECTOR('',#34576,10.);
#5612=VECTOR('',#34581,10.);
#5613=VECTOR('',#34586,10.);
#5614=VECTOR('',#34587,10.);
#5615=VECTOR('',#34590,10.);
#5616=VECTOR('',#34591,10.);
#5617=VECTOR('',#34594,10.);
#5618=VECTOR('',#34599,10.);
#5619=VECTOR('',#34600,10.);
#5620=VECTOR('',#34601,10.);
#5621=VECTOR('',#34604,10.);
#5622=VECTOR('',#34607,10.);
#5623=VECTOR('',#34612,10.);
#5624=VECTOR('',#34613,10.);
#5625=VECTOR('',#34616,10.);
#5626=VECTOR('',#34617,10.);
#5627=VECTOR('',#34620,10.);
#5628=VECTOR('',#34625,10.);
#5629=VECTOR('',#34630,10.);
#5630=VECTOR('',#34631,10.);
#5631=VECTOR('',#34634,10.);
#5632=VECTOR('',#34635,10.);
#5633=VECTOR('',#34638,10.);
#5634=VECTOR('',#34643,10.);
#5635=VECTOR('',#34644,10.);
#5636=VECTOR('',#34645,10.);
#5637=VECTOR('',#34648,10.);
#5638=VECTOR('',#34651,10.);
#5639=VECTOR('',#34656,10.);
#5640=VECTOR('',#34657,10.);
#5641=VECTOR('',#34660,10.);
#5642=VECTOR('',#34661,10.);
#5643=VECTOR('',#34664,10.);
#5644=VECTOR('',#34669,10.);
#5645=VECTOR('',#34674,10.);
#5646=VECTOR('',#34675,10.);
#5647=VECTOR('',#34678,10.);
#5648=VECTOR('',#34679,10.);
#5649=VECTOR('',#34682,10.);
#5650=VECTOR('',#34687,10.);
#5651=VECTOR('',#34688,10.);
#5652=VECTOR('',#34689,10.);
#5653=VECTOR('',#34692,10.);
#5654=VECTOR('',#34695,10.);
#5655=VECTOR('',#34700,10.);
#5656=VECTOR('',#34701,10.);
#5657=VECTOR('',#34704,10.);
#5658=VECTOR('',#34705,10.);
#5659=VECTOR('',#34708,10.);
#5660=VECTOR('',#34713,10.);
#5661=VECTOR('',#34714,10.);
#5662=VECTOR('',#34715,10.);
#5663=VECTOR('',#34718,10.);
#5664=VECTOR('',#34721,10.);
#5665=VECTOR('',#34732,10.);
#5666=VECTOR('',#34733,10.);
#5667=VECTOR('',#34734,10.);
#5668=VECTOR('',#34737,10.);
#5669=VECTOR('',#34738,10.);
#5670=VECTOR('',#34739,10.);
#5671=VECTOR('',#34742,10.);
#5672=VECTOR('',#34743,10.);
#5673=VECTOR('',#34744,10.);
#5674=VECTOR('',#34749,10.);
#5675=VECTOR('',#34754,2.51);
#5676=VECTOR('',#34763,9.8);
#5677=VECTOR('',#34768,10.);
#5678=VECTOR('',#34769,10.);
#5679=VECTOR('',#34774,11.25);
#5680=VECTOR('',#34779,12.5);
#5681=VECTOR('',#34788,15.);
#5682=VECTOR('',#34797,12.5);
#5683=VECTOR('',#34806,11.95);
#5684=VECTOR('',#34815,12.5);
#5685=VECTOR('',#34824,10.);
#5686=VECTOR('',#34829,9.75);
#5687=VECTOR('',#34838,15.9);
#5688=VECTOR('',#34847,22.7);
#5689=VECTOR('',#34858,25.775);
#5690=VECTOR('',#34863,26.);
#5691=VECTOR('',#34868,25.775);
#5692=VECTOR('',#34875,22.7);
#5693=VECTOR('',#34886,15.9);
#5694=VECTOR('',#34893,12.725);
#5695=VECTOR('',#34898,12.5);
#5696=VECTOR('',#34903,12.725);
#5697=VECTOR('',#34914,17.75);
#5698=VECTOR('',#34921,18.);
#5699=VECTOR('',#34932,10.);
#5700=VECTOR('',#34941,17.5);
#5701=VECTOR('',#34946,16.);
#5702=VECTOR('',#34953,13.);
#5703=VECTOR('',#34964,13.);
#5704=VECTOR('',#34975,19.75);
#5705=VECTOR('',#34980,20.);
#5706=VECTOR('',#34993,2.35);
#5707=VECTOR('',#34998,2.5);
#5708=VECTOR('',#35003,2.35);
#5709=VECTOR('',#35012,12.55);
#5710=VECTOR('',#35023,16.);
#5711=VECTOR('',#35038,10.);
#5712=VECTOR('',#35041,10.);
#5713=VECTOR('',#35050,10.);
#5714=VECTOR('',#35053,10.);
#5715=VECTOR('',#35060,10.);
#5716=VECTOR('',#35063,10.);
#5717=VECTOR('',#35066,10.);
#5718=VECTOR('',#35069,10.);
#5719=VECTOR('',#35082,10.);
#5720=VECTOR('',#35083,10.);
#5721=VECTOR('',#35086,10.);
#5722=VECTOR('',#35089,10.);
#5723=VECTOR('',#35096,10.);
#5724=VECTOR('',#35097,10.);
#5725=VECTOR('',#35100,10.);
#5726=VECTOR('',#35101,10.);
#5727=VECTOR('',#35106,10.);
#5728=VECTOR('',#35107,10.);
#5729=VECTOR('',#35110,10.);
#5730=VECTOR('',#35111,10.);
#5731=VECTOR('',#35114,10.);
#5732=VECTOR('',#35115,10.);
#5733=VECTOR('',#35126,10.);
#5734=VECTOR('',#35127,10.);
#5735=VECTOR('',#35130,10.);
#5736=VECTOR('',#35131,10.);
#5737=VECTOR('',#35136,10.);
#5738=VECTOR('',#35137,10.);
#5739=VECTOR('',#35146,10.);
#5740=VECTOR('',#35147,10.);
#5741=VECTOR('',#35152,10.);
#5742=VECTOR('',#35153,10.);
#5743=VECTOR('',#35160,10.);
#5744=VECTOR('',#35167,10.);
#5745=VECTOR('',#35178,13.9397047631572);
#5746=VECTOR('',#35183,16.15);
#5747=VECTOR('',#35188,10.);
#5748=VECTOR('',#35191,10.);
#5749=VECTOR('',#35194,10.);
#5750=VECTOR('',#35197,10.);
#5751=VECTOR('',#35200,10.);
#5752=VECTOR('',#35203,10.);
#5753=VECTOR('',#35206,10.);
#5754=VECTOR('',#35207,10.);
#5755=VECTOR('',#35208,10.);
#5756=VECTOR('',#35211,10.);
#5757=VECTOR('',#35212,10.);
#5758=VECTOR('',#35213,10.);
#5759=VECTOR('',#35216,10.);
#5760=VECTOR('',#35217,10.);
#5761=VECTOR('',#35218,10.);
#5762=VECTOR('',#35221,10.);
#5763=VECTOR('',#35222,10.);
#5764=VECTOR('',#35223,10.);
#5765=VECTOR('',#35226,10.);
#5766=VECTOR('',#35227,10.);
#5767=VECTOR('',#35228,10.);
#5768=VECTOR('',#35231,10.);
#5769=VECTOR('',#35232,10.);
#5770=VECTOR('',#35233,10.);
#5771=VECTOR('',#35236,10.);
#5772=VECTOR('',#35239,10.);
#5773=VECTOR('',#35242,10.);
#5774=VECTOR('',#35243,10.);
#5775=VECTOR('',#35246,10.);
#5776=VECTOR('',#35251,10.);
#5777=VECTOR('',#35252,10.);
#5778=VECTOR('',#35255,10.);
#5779=VECTOR('',#35260,10.);
#5780=VECTOR('',#35261,10.);
#5781=VECTOR('',#35264,10.);
#5782=VECTOR('',#35265,10.);
#5783=VECTOR('',#35266,10.);
#5784=VECTOR('',#35269,10.);
#5785=VECTOR('',#35270,10.);
#5786=VECTOR('',#35271,10.);
#5787=VECTOR('',#35274,10.);
#5788=VECTOR('',#35287,10.);
#5789=VECTOR('',#35322,16.45);
#5790=VECTOR('',#35325,16.7);
#5791=VECTOR('',#35330,10.);
#5792=VECTOR('',#35331,10.);
#5793=VECTOR('',#35332,10.);
#5794=VECTOR('',#35333,10.);
#5795=VECTOR('',#35336,10.);
#5796=VECTOR('',#35343,10.);
#5797=VECTOR('',#35344,10.);
#5798=VECTOR('',#35345,10.);
#5799=VECTOR('',#35348,10.);
#5800=VECTOR('',#35355,10.);
#5801=VECTOR('',#35356,10.);
#5802=VECTOR('',#35357,10.);
#5803=VECTOR('',#35360,10.);
#5804=VECTOR('',#35367,10.);
#5805=VECTOR('',#35368,10.);
#5806=VECTOR('',#35369,10.);
#5807=VECTOR('',#35378,10.);
#5808=VECTOR('',#35381,10.);
#5809=VECTOR('',#35384,10.);
#5810=VECTOR('',#35385,10.);
#5811=VECTOR('',#35388,10.);
#5812=VECTOR('',#35393,10.);
#5813=VECTOR('',#35394,10.);
#5814=VECTOR('',#35405,10.);
#5815=VECTOR('',#35408,10.);
#5816=VECTOR('',#35411,10.);
#5817=VECTOR('',#35414,10.);
#5818=VECTOR('',#35419,10.);
#5819=VECTOR('',#35420,10.);
#5820=VECTOR('',#35421,10.);
#5821=VECTOR('',#35424,10.);
#5822=VECTOR('',#35431,10.);
#5823=VECTOR('',#35432,10.);
#5824=VECTOR('',#35433,10.);
#5825=VECTOR('',#35436,10.);
#5826=VECTOR('',#35443,10.);
#5827=VECTOR('',#35444,10.);
#5828=VECTOR('',#35445,10.);
#5829=VECTOR('',#35448,10.);
#5830=VECTOR('',#35453,10.);
#5831=VECTOR('',#35454,10.);
#5832=VECTOR('',#35461,10.);
#5833=VECTOR('',#35462,10.);
#5834=VECTOR('',#35465,10.);
#5835=VECTOR('',#35480,10.);
#5836=VECTOR('',#35481,10.);
#5837=VECTOR('',#35482,10.);
#5838=VECTOR('',#35483,10.);
#5839=VECTOR('',#35486,10.);
#5840=VECTOR('',#35493,10.);
#5841=VECTOR('',#35494,10.);
#5842=VECTOR('',#35495,10.);
#5843=VECTOR('',#35498,10.);
#5844=VECTOR('',#35505,10.);
#5845=VECTOR('',#35506,10.);
#5846=VECTOR('',#35507,10.);
#5847=VECTOR('',#35510,10.);
#5848=VECTOR('',#35517,10.);
#5849=VECTOR('',#35518,10.);
#5850=VECTOR('',#35519,10.);
#5851=VECTOR('',#35528,10.);
#5852=VECTOR('',#35529,10.);
#5853=VECTOR('',#35532,10.);
#5854=VECTOR('',#35535,10.);
#5855=VECTOR('',#35538,10.);
#5856=VECTOR('',#35543,10.);
#5857=VECTOR('',#35546,10.);
#5858=VECTOR('',#35549,10.);
#5859=VECTOR('',#35554,2.75);
#5860=VECTOR('',#35557,2.75);
#5861=VECTOR('',#35560,2.75);
#5862=VECTOR('',#35563,2.75);
#5863=VECTOR('',#35578,24.5);
#5864=VECTOR('',#35599,23.9267766952966);
#5865=VECTOR('',#35608,24.5);
#5866=VECTOR('',#35623,10.);
#5867=VECTOR('',#35624,10.);
#5868=VECTOR('',#35625,10.);
#5869=VECTOR('',#35628,10.);
#5870=VECTOR('',#35629,10.);
#5871=VECTOR('',#35630,10.);
#5872=VECTOR('',#35633,10.);
#5873=VECTOR('',#35634,10.);
#5874=VECTOR('',#35635,10.);
#5875=VECTOR('',#35638,10.);
#5876=VECTOR('',#35639,10.);
#5877=VECTOR('',#35640,10.);
#5878=VECTOR('',#35643,10.);
#5879=VECTOR('',#35644,10.);
#5880=VECTOR('',#35645,10.);
#5881=VECTOR('',#35648,10.);
#5882=VECTOR('',#35649,10.);
#5883=VECTOR('',#35652,10.);
#5884=VECTOR('',#35653,10.);
#5885=VECTOR('',#35654,10.);
#5886=VECTOR('',#35657,10.);
#5887=VECTOR('',#35658,10.);
#5888=VECTOR('',#35661,10.);
#5889=VECTOR('',#35662,10.);
#5890=VECTOR('',#35663,10.);
#5891=VECTOR('',#35666,10.);
#5892=VECTOR('',#35667,10.);
#5893=VECTOR('',#35668,10.);
#5894=VECTOR('',#35671,10.);
#5895=VECTOR('',#35672,10.);
#5896=VECTOR('',#35675,10.);
#5897=VECTOR('',#35676,10.);
#5898=VECTOR('',#35679,10.);
#5899=VECTOR('',#35680,10.);
#5900=VECTOR('',#35683,10.);
#5901=VECTOR('',#35684,10.);
#5902=VECTOR('',#35687,10.);
#5903=VECTOR('',#35688,10.);
#5904=VECTOR('',#35691,10.);
#5905=VECTOR('',#35692,10.);
#5906=VECTOR('',#35695,10.);
#5907=VECTOR('',#35696,10.);
#5908=VECTOR('',#35699,10.);
#5909=VECTOR('',#35702,10.);
#5910=VECTOR('',#35713,24.8232233047034);
#5911=VECTOR('',#35720,25.);
#5912=VECTOR('',#35723,24.8232233047034);
#5913=VECTOR('',#35726,10.);
#5914=VECTOR('',#35727,10.);
#5915=VECTOR('',#35728,10.);
#5916=VECTOR('',#35731,10.);
#5917=VECTOR('',#35732,10.);
#5918=VECTOR('',#35733,10.);
#5919=VECTOR('',#35736,10.);
#5920=VECTOR('',#35737,10.);
#5921=VECTOR('',#35738,10.);
#5922=VECTOR('',#35739,10.);
#5923=VECTOR('',#35742,10.);
#5924=VECTOR('',#35743,10.);
#5925=VECTOR('',#35744,10.);
#5926=VECTOR('',#35745,10.);
#5927=VECTOR('',#35748,10.);
#5928=VECTOR('',#35749,10.);
#5929=VECTOR('',#35750,10.);
#5930=VECTOR('',#35751,10.);
#5931=VECTOR('',#35754,10.);
#5932=VECTOR('',#35755,10.);
#5933=VECTOR('',#35758,10.);
#5934=VECTOR('',#35759,10.);
#5935=VECTOR('',#35760,10.);
#5936=VECTOR('',#35763,10.);
#5937=VECTOR('',#35764,10.);
#5938=VECTOR('',#35765,10.);
#5939=VECTOR('',#35768,10.);
#5940=VECTOR('',#35769,10.);
#5941=VECTOR('',#35770,10.);
#5942=VECTOR('',#35773,10.);
#5943=VECTOR('',#35774,10.);
#5944=VECTOR('',#35775,10.);
#5945=VECTOR('',#35778,10.);
#5946=VECTOR('',#35779,10.);
#5947=VECTOR('',#35782,10.);
#5948=VECTOR('',#35783,10.);
#5949=VECTOR('',#35786,10.);
#5950=VECTOR('',#35787,10.);
#5951=VECTOR('',#35790,10.);
#5952=VECTOR('',#35791,10.);
#5953=VECTOR('',#35792,10.);
#5954=VECTOR('',#35795,10.);
#5955=VECTOR('',#35798,10.);
#5956=VECTOR('',#35805,10.);
#5957=VECTOR('',#35806,10.);
#5958=VECTOR('',#35807,10.);
#5959=VECTOR('',#35810,10.);
#5960=VECTOR('',#35811,10.);
#5961=VECTOR('',#35812,10.);
#5962=VECTOR('',#35815,10.);
#5963=VECTOR('',#35816,10.);
#5964=VECTOR('',#35817,10.);
#5965=VECTOR('',#35820,10.);
#5966=VECTOR('',#35821,10.);
#5967=VECTOR('',#35822,10.);
#5968=VECTOR('',#35825,10.);
#5969=VECTOR('',#35826,10.);
#5970=VECTOR('',#35827,10.);
#5971=VECTOR('',#35830,10.);
#5972=VECTOR('',#35831,10.);
#5973=VECTOR('',#35834,10.);
#5974=VECTOR('',#35835,10.);
#5975=VECTOR('',#35836,10.);
#5976=VECTOR('',#35839,10.);
#5977=VECTOR('',#35840,10.);
#5978=VECTOR('',#35843,10.);
#5979=VECTOR('',#35844,10.);
#5980=VECTOR('',#35845,10.);
#5981=VECTOR('',#35848,10.);
#5982=VECTOR('',#35849,10.);
#5983=VECTOR('',#35850,10.);
#5984=VECTOR('',#35853,10.);
#5985=VECTOR('',#35854,10.);
#5986=VECTOR('',#35857,10.);
#5987=VECTOR('',#35858,10.);
#5988=VECTOR('',#35861,10.);
#5989=VECTOR('',#35862,10.);
#5990=VECTOR('',#35865,10.);
#5991=VECTOR('',#35866,10.);
#5992=VECTOR('',#35869,10.);
#5993=VECTOR('',#35870,10.);
#5994=VECTOR('',#35873,10.);
#5995=VECTOR('',#35874,10.);
#5996=VECTOR('',#35877,10.);
#5997=VECTOR('',#35878,10.);
#5998=VECTOR('',#35881,10.);
#5999=VECTOR('',#35884,10.);
#6000=VECTOR('',#35889,10.);
#6001=VECTOR('',#35892,3.4);
#6002=VECTOR('',#35899,10.);
#6003=VECTOR('',#35902,10.);
#6004=VECTOR('',#35905,10.);
#6005=VECTOR('',#35912,10.);
#6006=VECTOR('',#35919,10.);
#6007=VECTOR('',#35920,10.);
#6008=VECTOR('',#35927,5.);
#6009=VECTOR('',#35932,5.);
#6010=VECTOR('',#35935,5.);
#6011=VECTOR('',#35938,5.);
#6012=VECTOR('',#35941,5.);
#6013=VECTOR('',#35944,5.);
#6014=VECTOR('',#35947,5.);
#6015=VECTOR('',#35950,5.);
#6016=VECTOR('',#35953,5.);
#6017=VECTOR('',#35956,5.);
#6018=VECTOR('',#35959,5.);
#6019=VECTOR('',#35962,5.);
#6020=VECTOR('',#35965,5.);
#6021=VECTOR('',#35968,5.);
#6022=VECTOR('',#35971,5.);
#6023=VECTOR('',#35974,5.);
#6024=VECTOR('',#35977,5.);
#6025=VECTOR('',#35980,5.);
#6026=VECTOR('',#35983,5.);
#6027=VECTOR('',#35986,5.);
#6028=VECTOR('',#35989,4.0705);
#6029=VECTOR('',#35994,4.0705);
#6030=VECTOR('',#35999,4.0705);
#6031=VECTOR('',#36002,4.0705);
#6032=VECTOR('',#36005,4.0705);
#6033=VECTOR('',#36008,4.0705);
#6034=VECTOR('',#36011,4.0705);
#6035=VECTOR('',#36014,4.0705);
#6036=VECTOR('',#36017,4.0705);
#6037=VECTOR('',#36020,4.0705);
#6038=VECTOR('',#36023,4.0705);
#6039=VECTOR('',#36026,4.0705);
#6040=VECTOR('',#36029,4.0705);
#6041=VECTOR('',#36032,4.0705);
#6042=VECTOR('',#36035,4.0705);
#6043=VECTOR('',#36038,4.0705);
#6044=VECTOR('',#36041,4.0705);
#6045=VECTOR('',#36044,4.0705);
#6046=VECTOR('',#36047,4.0705);
#6047=VECTOR('',#36050,4.0705);
#6048=VECTOR('',#36063,8.83380215351701);
#6049=VECTOR('',#36068,10.);
#6050=VECTOR('',#36069,10.);
#6051=VECTOR('',#36070,10.);
#6052=VECTOR('',#36073,10.);
#6053=VECTOR('',#36074,10.);
#6054=VECTOR('',#36077,10.);
#6055=VECTOR('',#36078,10.);
#6056=VECTOR('',#36081,10.);
#6057=VECTOR('',#36082,10.);
#6058=VECTOR('',#36083,10.);
#6059=VECTOR('',#36088,10.);
#6060=VECTOR('',#36091,10.);
#6061=VECTOR('',#36102,4.75);
#6062=VECTOR('',#36109,5.);
#6063=VECTOR('',#36114,5.);
#6064=VECTOR('',#36117,5.);
#6065=VECTOR('',#36120,5.);
#6066=VECTOR('',#36123,5.);
#6067=VECTOR('',#36126,5.);
#6068=VECTOR('',#36129,5.);
#6069=VECTOR('',#36132,5.);
#6070=VECTOR('',#36135,5.);
#6071=VECTOR('',#36138,5.);
#6072=VECTOR('',#36141,5.);
#6073=VECTOR('',#36144,5.);
#6074=VECTOR('',#36147,5.);
#6075=VECTOR('',#36150,5.);
#6076=VECTOR('',#36153,5.);
#6077=VECTOR('',#36156,5.);
#6078=VECTOR('',#36159,5.);
#6079=VECTOR('',#36162,5.);
#6080=VECTOR('',#36165,5.);
#6081=VECTOR('',#36168,5.);
#6082=VECTOR('',#36171,4.0705);
#6083=VECTOR('',#36176,4.0705);
#6084=VECTOR('',#36181,4.0705);
#6085=VECTOR('',#36184,4.0705);
#6086=VECTOR('',#36187,4.0705);
#6087=VECTOR('',#36190,4.0705);
#6088=VECTOR('',#36193,4.0705);
#6089=VECTOR('',#36196,4.0705);
#6090=VECTOR('',#36199,4.0705);
#6091=VECTOR('',#36202,4.0705);
#6092=VECTOR('',#36205,4.0705);
#6093=VECTOR('',#36208,4.0705);
#6094=VECTOR('',#36211,4.0705);
#6095=VECTOR('',#36214,4.0705);
#6096=VECTOR('',#36217,4.0705);
#6097=VECTOR('',#36220,4.0705);
#6098=VECTOR('',#36223,4.0705);
#6099=VECTOR('',#36226,4.0705);
#6100=VECTOR('',#36229,4.0705);
#6101=VECTOR('',#36232,4.0705);
#6102=VECTOR('',#36245,10.);
#6103=VECTOR('',#36246,10.);
#6104=VECTOR('',#36247,10.);
#6105=VECTOR('',#36248,10.);
#6106=VECTOR('',#36253,10.);
#6107=VECTOR('',#36256,10.);
#6108=VECTOR('',#36257,10.);
#6109=VECTOR('',#36264,10.);
#6110=VECTOR('',#36265,10.);
#6111=VECTOR('',#36266,10.);
#6112=VECTOR('',#36267,10.);
#6113=VECTOR('',#36272,10.);
#6114=VECTOR('',#36275,10.);
#6115=VECTOR('',#36276,10.);
#6116=VECTOR('',#36283,10.);
#6117=VECTOR('',#36284,10.);
#6118=VECTOR('',#36285,10.);
#6119=VECTOR('',#36286,10.);
#6120=VECTOR('',#36291,10.);
#6121=VECTOR('',#36294,10.);
#6122=VECTOR('',#36295,10.);
#6123=VECTOR('',#36302,10.);
#6124=VECTOR('',#36303,10.);
#6125=VECTOR('',#36304,10.);
#6126=VECTOR('',#36305,10.);
#6127=VECTOR('',#36310,10.);
#6128=VECTOR('',#36313,10.);
#6129=VECTOR('',#36314,10.);
#6130=VECTOR('',#36321,10.);
#6131=VECTOR('',#36322,10.);
#6132=VECTOR('',#36323,10.);
#6133=VECTOR('',#36324,10.);
#6134=VECTOR('',#36329,10.);
#6135=VECTOR('',#36332,10.);
#6136=VECTOR('',#36333,10.);
#6137=VECTOR('',#36340,10.);
#6138=VECTOR('',#36341,10.);
#6139=VECTOR('',#36342,10.);
#6140=VECTOR('',#36343,10.);
#6141=VECTOR('',#36348,10.);
#6142=VECTOR('',#36351,10.);
#6143=VECTOR('',#36352,10.);
#6144=VECTOR('',#36359,10.);
#6145=VECTOR('',#36360,10.);
#6146=VECTOR('',#36361,10.);
#6147=VECTOR('',#36362,10.);
#6148=VECTOR('',#36367,10.);
#6149=VECTOR('',#36370,10.);
#6150=VECTOR('',#36371,10.);
#6151=VECTOR('',#36378,10.);
#6152=VECTOR('',#36379,10.);
#6153=VECTOR('',#36380,10.);
#6154=VECTOR('',#36381,10.);
#6155=VECTOR('',#36386,10.);
#6156=VECTOR('',#36389,10.);
#6157=VECTOR('',#36390,10.);
#6158=VECTOR('',#36397,10.);
#6159=VECTOR('',#36398,10.);
#6160=VECTOR('',#36399,10.);
#6161=VECTOR('',#36400,10.);
#6162=VECTOR('',#36405,10.);
#6163=VECTOR('',#36408,10.);
#6164=VECTOR('',#36409,10.);
#6165=VECTOR('',#36416,10.);
#6166=VECTOR('',#36417,10.);
#6167=VECTOR('',#36418,10.);
#6168=VECTOR('',#36419,10.);
#6169=VECTOR('',#36424,10.);
#6170=VECTOR('',#36427,10.);
#6171=VECTOR('',#36428,10.);
#6172=VECTOR('',#36435,10.);
#6173=VECTOR('',#36436,10.);
#6174=VECTOR('',#36437,10.);
#6175=VECTOR('',#36438,10.);
#6176=VECTOR('',#36443,10.);
#6177=VECTOR('',#36446,10.);
#6178=VECTOR('',#36447,10.);
#6179=VECTOR('',#36454,10.);
#6180=VECTOR('',#36455,10.);
#6181=VECTOR('',#36456,10.);
#6182=VECTOR('',#36457,10.);
#6183=VECTOR('',#36462,10.);
#6184=VECTOR('',#36465,10.);
#6185=VECTOR('',#36466,10.);
#6186=VECTOR('',#36473,10.);
#6187=VECTOR('',#36474,10.);
#6188=VECTOR('',#36475,10.);
#6189=VECTOR('',#36476,10.);
#6190=VECTOR('',#36481,10.);
#6191=VECTOR('',#36484,10.);
#6192=VECTOR('',#36485,10.);
#6193=VECTOR('',#36492,10.);
#6194=VECTOR('',#36493,10.);
#6195=VECTOR('',#36494,10.);
#6196=VECTOR('',#36495,10.);
#6197=VECTOR('',#36500,10.);
#6198=VECTOR('',#36503,10.);
#6199=VECTOR('',#36504,10.);
#6200=VECTOR('',#36511,10.);
#6201=VECTOR('',#36512,10.);
#6202=VECTOR('',#36513,10.);
#6203=VECTOR('',#36514,10.);
#6204=VECTOR('',#36519,10.);
#6205=VECTOR('',#36522,10.);
#6206=VECTOR('',#36523,10.);
#6207=VECTOR('',#36530,10.);
#6208=VECTOR('',#36531,10.);
#6209=VECTOR('',#36532,10.);
#6210=VECTOR('',#36533,10.);
#6211=VECTOR('',#36538,10.);
#6212=VECTOR('',#36541,10.);
#6213=VECTOR('',#36542,10.);
#6214=VECTOR('',#36549,10.);
#6215=VECTOR('',#36550,10.);
#6216=VECTOR('',#36551,10.);
#6217=VECTOR('',#36552,10.);
#6218=VECTOR('',#36557,10.);
#6219=VECTOR('',#36560,10.);
#6220=VECTOR('',#36561,10.);
#6221=VECTOR('',#36568,10.);
#6222=VECTOR('',#36569,10.);
#6223=VECTOR('',#36570,10.);
#6224=VECTOR('',#36571,10.);
#6225=VECTOR('',#36576,10.);
#6226=VECTOR('',#36581,10.);
#6227=VECTOR('',#36582,10.);
#6228=VECTOR('',#36591,10.);
#6229=VECTOR('',#36592,10.);
#6230=VECTOR('',#36593,10.);
#6231=VECTOR('',#36594,10.);
#6232=VECTOR('',#36599,10.);
#6233=VECTOR('',#36602,10.);
#6234=VECTOR('',#36603,10.);
#6235=VECTOR('',#36610,10.);
#6236=VECTOR('',#36611,10.);
#6237=VECTOR('',#36612,10.);
#6238=VECTOR('',#36613,10.);
#6239=VECTOR('',#36618,10.);
#6240=VECTOR('',#36621,10.);
#6241=VECTOR('',#36622,10.);
#6242=VECTOR('',#36629,10.);
#6243=VECTOR('',#36630,10.);
#6244=VECTOR('',#36631,10.);
#6245=VECTOR('',#36632,10.);
#6246=VECTOR('',#36637,10.);
#6247=VECTOR('',#36640,10.);
#6248=VECTOR('',#36641,10.);
#6249=VECTOR('',#36648,10.);
#6250=VECTOR('',#36649,10.);
#6251=VECTOR('',#36650,10.);
#6252=VECTOR('',#36651,10.);
#6253=VECTOR('',#36656,10.);
#6254=VECTOR('',#36659,10.);
#6255=VECTOR('',#36660,10.);
#6256=VECTOR('',#36667,10.);
#6257=VECTOR('',#36668,10.);
#6258=VECTOR('',#36669,10.);
#6259=VECTOR('',#36670,10.);
#6260=VECTOR('',#36675,10.);
#6261=VECTOR('',#36678,10.);
#6262=VECTOR('',#36679,10.);
#6263=VECTOR('',#36686,10.);
#6264=VECTOR('',#36687,10.);
#6265=VECTOR('',#36688,10.);
#6266=VECTOR('',#36689,10.);
#6267=VECTOR('',#36694,10.);
#6268=VECTOR('',#36697,10.);
#6269=VECTOR('',#36698,10.);
#6270=VECTOR('',#36705,10.);
#6271=VECTOR('',#36706,10.);
#6272=VECTOR('',#36707,10.);
#6273=VECTOR('',#36708,10.);
#6274=VECTOR('',#36713,10.);
#6275=VECTOR('',#36716,10.);
#6276=VECTOR('',#36717,10.);
#6277=VECTOR('',#36724,10.);
#6278=VECTOR('',#36725,10.);
#6279=VECTOR('',#36726,10.);
#6280=VECTOR('',#36727,10.);
#6281=VECTOR('',#36732,10.);
#6282=VECTOR('',#36735,10.);
#6283=VECTOR('',#36736,10.);
#6284=VECTOR('',#36743,10.);
#6285=VECTOR('',#36744,10.);
#6286=VECTOR('',#36745,10.);
#6287=VECTOR('',#36746,10.);
#6288=VECTOR('',#36751,10.);
#6289=VECTOR('',#36754,10.);
#6290=VECTOR('',#36755,10.);
#6291=VECTOR('',#36762,10.);
#6292=VECTOR('',#36763,10.);
#6293=VECTOR('',#36764,10.);
#6294=VECTOR('',#36765,10.);
#6295=VECTOR('',#36770,10.);
#6296=VECTOR('',#36773,10.);
#6297=VECTOR('',#36774,10.);
#6298=VECTOR('',#36781,10.);
#6299=VECTOR('',#36782,10.);
#6300=VECTOR('',#36783,10.);
#6301=VECTOR('',#36784,10.);
#6302=VECTOR('',#36789,10.);
#6303=VECTOR('',#36792,10.);
#6304=VECTOR('',#36793,10.);
#6305=VECTOR('',#36800,10.);
#6306=VECTOR('',#36801,10.);
#6307=VECTOR('',#36802,10.);
#6308=VECTOR('',#36803,10.);
#6309=VECTOR('',#36808,10.);
#6310=VECTOR('',#36811,10.);
#6311=VECTOR('',#36812,10.);
#6312=VECTOR('',#36819,10.);
#6313=VECTOR('',#36820,10.);
#6314=VECTOR('',#36821,10.);
#6315=VECTOR('',#36822,10.);
#6316=VECTOR('',#36827,10.);
#6317=VECTOR('',#36830,10.);
#6318=VECTOR('',#36831,10.);
#6319=VECTOR('',#36838,10.);
#6320=VECTOR('',#36839,10.);
#6321=VECTOR('',#36840,10.);
#6322=VECTOR('',#36841,10.);
#6323=VECTOR('',#36846,10.);
#6324=VECTOR('',#36849,10.);
#6325=VECTOR('',#36850,10.);
#6326=VECTOR('',#36857,10.);
#6327=VECTOR('',#36858,10.);
#6328=VECTOR('',#36859,10.);
#6329=VECTOR('',#36860,10.);
#6330=VECTOR('',#36865,10.);
#6331=VECTOR('',#36868,10.);
#6332=VECTOR('',#36869,10.);
#6333=VECTOR('',#36876,10.);
#6334=VECTOR('',#36877,10.);
#6335=VECTOR('',#36878,10.);
#6336=VECTOR('',#36879,10.);
#6337=VECTOR('',#36884,10.);
#6338=VECTOR('',#36887,10.);
#6339=VECTOR('',#36888,10.);
#6340=VECTOR('',#36895,10.);
#6341=VECTOR('',#36896,10.);
#6342=VECTOR('',#36897,10.);
#6343=VECTOR('',#36898,10.);
#6344=VECTOR('',#36903,10.);
#6345=VECTOR('',#36906,10.);
#6346=VECTOR('',#36907,10.);
#6347=VECTOR('',#36914,10.);
#6348=VECTOR('',#36915,10.);
#6349=VECTOR('',#36916,10.);
#6350=VECTOR('',#36917,10.);
#6351=VECTOR('',#36922,10.);
#6352=VECTOR('',#36925,10.);
#6353=VECTOR('',#36926,10.);
#6354=VECTOR('',#36933,10.);
#6355=VECTOR('',#36934,10.);
#6356=VECTOR('',#36935,10.);
#6357=VECTOR('',#36936,10.);
#6358=VECTOR('',#36939,10.);
#6359=VECTOR('',#36940,10.);
#6360=VECTOR('',#36941,10.);
#6361=VECTOR('',#36944,10.);
#6362=VECTOR('',#36945,10.);
#6363=VECTOR('',#36946,10.);
#6364=VECTOR('',#36949,10.);
#6365=VECTOR('',#36950,10.);
#6366=VECTOR('',#36951,10.);
#6367=VECTOR('',#36954,10.);
#6368=VECTOR('',#36955,10.);
#6369=VECTOR('',#36956,10.);
#6370=VECTOR('',#36959,10.);
#6371=VECTOR('',#36960,10.);
#6372=VECTOR('',#36969,4.75);
#6373=VECTOR('',#36982,8.);
#6374=VECTOR('',#36983,8.);
#6375=VECTOR('',#36988,7.75);
#6376=VECTOR('',#36995,10.);
#6377=VECTOR('',#36996,10.);
#6378=VECTOR('',#36997,10.);
#6379=VECTOR('',#37000,10.);
#6380=VECTOR('',#37001,10.);
#6381=VECTOR('',#37002,10.);
#6382=VECTOR('',#37005,10.);
#6383=VECTOR('',#37006,10.);
#6384=VECTOR('',#37007,10.);
#6385=VECTOR('',#37010,10.);
#6386=VECTOR('',#37011,10.);
#6387=VECTOR('',#37012,10.);
#6388=VECTOR('',#37015,10.);
#6389=VECTOR('',#37016,10.);
#6390=VECTOR('',#37019,10.);
#6391=VECTOR('',#37020,10.);
#6392=VECTOR('',#37021,10.);
#6393=VECTOR('',#37024,10.);
#6394=VECTOR('',#37025,10.);
#6395=VECTOR('',#37026,10.);
#6396=VECTOR('',#37029,10.);
#6397=VECTOR('',#37030,10.);
#6398=VECTOR('',#37031,10.);
#6399=VECTOR('',#37034,10.);
#6400=VECTOR('',#37035,10.);
#6401=VECTOR('',#37036,10.);
#6402=VECTOR('',#37039,10.);
#6403=VECTOR('',#37040,10.);
#6404=VECTOR('',#37043,10.);
#6405=VECTOR('',#37044,10.);
#6406=VECTOR('',#37045,10.);
#6407=VECTOR('',#37048,10.);
#6408=VECTOR('',#37049,10.);
#6409=VECTOR('',#37050,10.);
#6410=VECTOR('',#37053,10.);
#6411=VECTOR('',#37054,10.);
#6412=VECTOR('',#37055,10.);
#6413=VECTOR('',#37058,10.);
#6414=VECTOR('',#37059,10.);
#6415=VECTOR('',#37060,10.);
#6416=VECTOR('',#37063,10.);
#6417=VECTOR('',#37064,10.);
#6418=VECTOR('',#37067,10.);
#6419=VECTOR('',#37068,10.);
#6420=VECTOR('',#37071,10.);
#6421=VECTOR('',#37072,10.);
#6422=VECTOR('',#37075,10.);
#6423=VECTOR('',#37076,10.);
#6424=VECTOR('',#37079,10.);
#6425=VECTOR('',#37082,10.);
#6426=VECTOR('',#37085,10.);
#6427=VECTOR('',#37088,10.);
#6428=VECTOR('',#37089,10.);
#6429=VECTOR('',#37090,10.);
#6430=VECTOR('',#37091,10.);
#6431=VECTOR('',#37092,10.);
#6432=VECTOR('',#37093,10.);
#6433=VECTOR('',#37096,10.);
#6434=VECTOR('',#37097,10.);
#6435=VECTOR('',#37098,10.);
#6436=VECTOR('',#37101,10.);
#6437=VECTOR('',#37102,10.);
#6438=VECTOR('',#37105,10.);
#6439=VECTOR('',#37106,10.);
#6440=VECTOR('',#37107,10.);
#6441=VECTOR('',#37110,10.);
#6442=VECTOR('',#37111,10.);
#6443=VECTOR('',#37114,10.);
#6444=VECTOR('',#37117,10.);
#6445=VECTOR('',#37120,10.);
#6446=VECTOR('',#37121,10.);
#6447=VECTOR('',#37122,10.);
#6448=VECTOR('',#37125,10.);
#6449=VECTOR('',#37126,10.);
#6450=VECTOR('',#37129,10.);
#6451=VECTOR('',#37130,10.);
#6452=VECTOR('',#37133,10.);
#6453=VECTOR('',#37134,10.);
#6454=VECTOR('',#37137,10.);
#6455=VECTOR('',#37138,10.);
#6456=VECTOR('',#37141,10.);
#6457=VECTOR('',#37146,10.);
#6458=VECTOR('',#37147,10.);
#6459=VECTOR('',#37148,10.);
#6460=VECTOR('',#37165,6.6);
#6461=VECTOR('',#37168,6.85);
#6462=VECTOR('',#37173,2.5);
#6463=VECTOR('',#37178,2.5);
#6464=VECTOR('',#37181,2.5);
#6465=VECTOR('',#37184,2.5);
#6466=VECTOR('',#37187,2.5);
#6467=VECTOR('',#37190,2.5);
#6468=VECTOR('',#37193,2.5);
#6469=VECTOR('',#37196,2.5);
#6470=VECTOR('',#37199,2.5);
#6471=VECTOR('',#37202,2.5);
#6472=VECTOR('',#37205,2.5);
#6473=VECTOR('',#37208,2.5);
#6474=VECTOR('',#37211,2.5);
#6475=VECTOR('',#37216,1.99475);
#6476=VECTOR('',#37221,1.99475);
#6477=VECTOR('',#37224,1.99475);
#6478=VECTOR('',#37227,1.99475);
#6479=VECTOR('',#37230,1.99475);
#6480=VECTOR('',#37233,1.99475);
#6481=VECTOR('',#37236,1.99475);
#6482=VECTOR('',#37239,1.99475);
#6483=VECTOR('',#37242,1.99475);
#6484=VECTOR('',#37245,1.99475);
#6485=VECTOR('',#37248,1.99475);
#6486=VECTOR('',#37251,1.99475);
#6487=VECTOR('',#37264,10.);
#6488=VECTOR('',#37265,10.);
#6489=VECTOR('',#37266,10.);
#6490=VECTOR('',#37269,10.);
#6491=VECTOR('',#37270,10.);
#6492=VECTOR('',#37273,10.);
#6493=VECTOR('',#37274,10.);
#6494=VECTOR('',#37277,10.);
#6495=VECTOR('',#37278,10.);
#6496=VECTOR('',#37281,10.);
#6497=VECTOR('',#37282,10.);
#6498=VECTOR('',#37285,10.);
#6499=VECTOR('',#37294,2.35);
#6500=CYLINDRICAL_SURFACE('',#27470,92.);
#6501=CYLINDRICAL_SURFACE('',#27496,2.);
#6502=CYLINDRICAL_SURFACE('',#27502,2.);
#6503=CYLINDRICAL_SURFACE('',#27507,2.);
#6504=CYLINDRICAL_SURFACE('',#27512,2.);
#6505=CYLINDRICAL_SURFACE('',#27516,4.00000000000002);
#6506=CYLINDRICAL_SURFACE('',#27519,4.00000000000002);
#6507=CYLINDRICAL_SURFACE('',#27525,2.);
#6508=CYLINDRICAL_SURFACE('',#27531,2.);
#6509=CYLINDRICAL_SURFACE('',#27535,2.);
#6510=CYLINDRICAL_SURFACE('',#27539,2.);
#6511=CYLINDRICAL_SURFACE('',#27544,4.00000000000002);
#6512=CYLINDRICAL_SURFACE('',#27553,2.);
#6513=CYLINDRICAL_SURFACE('',#27559,2.);
#6514=CYLINDRICAL_SURFACE('',#27564,2.);
#6515=CYLINDRICAL_SURFACE('',#27569,2.);
#6516=CYLINDRICAL_SURFACE('',#27573,3.);
#6517=CYLINDRICAL_SURFACE('',#27576,3.00000000000001);
#6518=CYLINDRICAL_SURFACE('',#27581,2.);
#6519=CYLINDRICAL_SURFACE('',#27587,2.);
#6520=CYLINDRICAL_SURFACE('',#27592,2.);
#6521=CYLINDRICAL_SURFACE('',#27597,2.);
#6522=CYLINDRICAL_SURFACE('',#27601,3.);
#6523=CYLINDRICAL_SURFACE('',#27604,2.99999999999999);
#6524=CYLINDRICAL_SURFACE('',#27612,70.2);
#6525=CYLINDRICAL_SURFACE('',#27622,20.05);
#6526=CYLINDRICAL_SURFACE('',#27624,2.);
#6527=CYLINDRICAL_SURFACE('',#27627,2.);
#6528=CYLINDRICAL_SURFACE('',#27629,57.);
#6529=CYLINDRICAL_SURFACE('',#27643,5.99999999999997);
#6530=CYLINDRICAL_SURFACE('',#27647,16.75);
#6531=CYLINDRICAL_SURFACE('',#27649,2.);
#6532=CYLINDRICAL_SURFACE('',#27651,2.);
#6533=CYLINDRICAL_SURFACE('',#27658,2.);
#6534=CYLINDRICAL_SURFACE('',#27662,5.99999999999996);
#6535=CYLINDRICAL_SURFACE('',#27666,2.);
#6536=CYLINDRICAL_SURFACE('',#27672,2.);
#6537=CYLINDRICAL_SURFACE('',#27677,2.);
#6538=CYLINDRICAL_SURFACE('',#27683,2.);
#6539=CYLINDRICAL_SURFACE('',#27706,5.99999999999999);
#6540=CYLINDRICAL_SURFACE('',#27707,16.75);
#6541=CYLINDRICAL_SURFACE('',#27709,7.);
#6542=CYLINDRICAL_SURFACE('',#27710,7.);
#6543=CYLINDRICAL_SURFACE('',#27711,6.9);
#6544=CYLINDRICAL_SURFACE('',#27714,6.9);
#6545=CYLINDRICAL_SURFACE('',#27717,16.75);
#6546=CYLINDRICAL_SURFACE('',#27724,5.05);
#6547=CYLINDRICAL_SURFACE('',#27727,5.05);
#6548=CYLINDRICAL_SURFACE('',#27730,5.05);
#6549=CYLINDRICAL_SURFACE('',#27733,5.05);
#6550=CYLINDRICAL_SURFACE('',#27736,5.05);
#6551=CYLINDRICAL_SURFACE('',#27739,5.05);
#6552=CYLINDRICAL_SURFACE('',#27742,5.05);
#6553=CYLINDRICAL_SURFACE('',#27745,5.05);
#6554=CYLINDRICAL_SURFACE('',#27748,5.05);
#6555=CYLINDRICAL_SURFACE('',#27751,5.05);
#6556=CYLINDRICAL_SURFACE('',#27754,5.05);
#6557=CYLINDRICAL_SURFACE('',#27757,5.05);
#6558=CYLINDRICAL_SURFACE('',#27763,13.);
#6559=CYLINDRICAL_SURFACE('',#27764,2.99999999999999);
#6560=CYLINDRICAL_SURFACE('',#27766,3.00000000000001);
#6561=CYLINDRICAL_SURFACE('',#27768,3.);
#6562=CYLINDRICAL_SURFACE('',#27770,2.99999999999999);
#6563=CYLINDRICAL_SURFACE('',#27772,4.00000000000001);
#6564=CYLINDRICAL_SURFACE('',#27773,6.00000000000001);
#6565=CYLINDRICAL_SURFACE('',#27775,6.00000000000001);
#6566=CYLINDRICAL_SURFACE('',#27777,6.00000000000001);
#6567=CYLINDRICAL_SURFACE('',#27779,6.00000000000001);
#6568=CYLINDRICAL_SURFACE('',#27784,5.99999999999998);
#6569=CYLINDRICAL_SURFACE('',#27790,1.5);
#6570=CYLINDRICAL_SURFACE('',#27793,1.5);
#6571=CYLINDRICAL_SURFACE('',#27798,1.5);
#6572=CYLINDRICAL_SURFACE('',#27804,1.5);
#6573=CYLINDRICAL_SURFACE('',#27807,1.5);
#6574=CYLINDRICAL_SURFACE('',#27812,1.5);
#6575=CYLINDRICAL_SURFACE('',#27815,1.5);
#6576=CYLINDRICAL_SURFACE('',#27823,92.);
#6577=CYLINDRICAL_SURFACE('',#27842,1.5);
#6578=CYLINDRICAL_SURFACE('',#27844,1.5);
#6579=CYLINDRICAL_SURFACE('',#27882,1.5);
#6580=CYLINDRICAL_SURFACE('',#27883,1.5);
#6581=CYLINDRICAL_SURFACE('',#27887,1.5);
#6582=CYLINDRICAL_SURFACE('',#27892,56.5);
#6583=CYLINDRICAL_SURFACE('',#27893,1.5);
#6584=CYLINDRICAL_SURFACE('',#27898,1.5);
#6585=CYLINDRICAL_SURFACE('',#27899,1.5);
#6586=CYLINDRICAL_SURFACE('',#27907,70.2);
#6587=CYLINDRICAL_SURFACE('',#27914,5.5);
#6588=CYLINDRICAL_SURFACE('',#27915,5.5);
#6589=CYLINDRICAL_SURFACE('',#27916,5.5);
#6590=CYLINDRICAL_SURFACE('',#27917,5.5);
#6591=CYLINDRICAL_SURFACE('',#27918,75.05);
#6592=CYLINDRICAL_SURFACE('',#27920,1.5);
#6593=CYLINDRICAL_SURFACE('',#27923,1.5);
#6594=CYLINDRICAL_SURFACE('',#27926,1.5);
#6595=CYLINDRICAL_SURFACE('',#27929,1.5);
#6596=CYLINDRICAL_SURFACE('',#27933,1.5);
#6597=CYLINDRICAL_SURFACE('',#27978,5.5);
#6598=CYLINDRICAL_SURFACE('',#27979,5.5);
#6599=CYLINDRICAL_SURFACE('',#27980,5.5);
#6600=CYLINDRICAL_SURFACE('',#27981,5.5);
#6601=CYLINDRICAL_SURFACE('',#27983,57.);
#6602=CYLINDRICAL_SURFACE('',#27993,26.01);
#6603=CYLINDRICAL_SURFACE('',#28017,7.);
#6604=CYLINDRICAL_SURFACE('',#28021,7.);
#6605=CYLINDRICAL_SURFACE('',#28034,2.55);
#6606=CYLINDRICAL_SURFACE('',#28039,6.00000000000002);
#6607=CYLINDRICAL_SURFACE('',#28041,2.55);
#6608=CYLINDRICAL_SURFACE('',#28045,2.55);
#6609=CYLINDRICAL_SURFACE('',#28050,2.55);
#6610=CYLINDRICAL_SURFACE('',#28074,7.);
#6611=CYLINDRICAL_SURFACE('',#28078,7.);
#6612=CYLINDRICAL_SURFACE('',#28082,7.);
#6613=CYLINDRICAL_SURFACE('',#28086,6.99999999999999);
#6614=CYLINDRICAL_SURFACE('',#28101,70.);
#6615=CYLINDRICAL_SURFACE('',#28144,2.);
#6616=CYLINDRICAL_SURFACE('',#28149,2.);
#6617=CYLINDRICAL_SURFACE('',#28153,2.);
#6618=CYLINDRICAL_SURFACE('',#28157,2.);
#6619=CYLINDRICAL_SURFACE('',#28160,4.);
#6620=CYLINDRICAL_SURFACE('',#28162,3.99999999999999);
#6621=CYLINDRICAL_SURFACE('',#28167,125.);
#6622=CYLINDRICAL_SURFACE('',#28182,45.);
#6623=CYLINDRICAL_SURFACE('',#28188,90.1);
#6624=CYLINDRICAL_SURFACE('',#28194,2.);
#6625=CYLINDRICAL_SURFACE('',#28201,2.);
#6626=CYLINDRICAL_SURFACE('',#28207,2.);
#6627=CYLINDRICAL_SURFACE('',#28213,2.);
#6628=CYLINDRICAL_SURFACE('',#28218,5.99999999999999);
#6629=CYLINDRICAL_SURFACE('',#28221,5.99999999999998);
#6630=CYLINDRICAL_SURFACE('',#28225,2.);
#6631=CYLINDRICAL_SURFACE('',#28232,2.);
#6632=CYLINDRICAL_SURFACE('',#28238,2.);
#6633=CYLINDRICAL_SURFACE('',#28243,2.);
#6634=CYLINDRICAL_SURFACE('',#28247,6.00000000000001);
#6635=CYLINDRICAL_SURFACE('',#28249,6.00000000000001);
#6636=CYLINDRICAL_SURFACE('',#28251,2.);
#6637=CYLINDRICAL_SURFACE('',#28258,2.);
#6638=CYLINDRICAL_SURFACE('',#28264,2.);
#6639=CYLINDRICAL_SURFACE('',#28270,2.);
#6640=CYLINDRICAL_SURFACE('',#28275,8.);
#6641=CYLINDRICAL_SURFACE('',#28281,8.);
#6642=CYLINDRICAL_SURFACE('',#28284,2.);
#6643=CYLINDRICAL_SURFACE('',#28290,2.);
#6644=CYLINDRICAL_SURFACE('',#28295,2.);
#6645=CYLINDRICAL_SURFACE('',#28300,2.);
#6646=CYLINDRICAL_SURFACE('',#28304,6.00000000000001);
#6647=CYLINDRICAL_SURFACE('',#28307,5.99999999999998);
#6648=CYLINDRICAL_SURFACE('',#28310,2.);
#6649=CYLINDRICAL_SURFACE('',#28316,2.);
#6650=CYLINDRICAL_SURFACE('',#28321,2.);
#6651=CYLINDRICAL_SURFACE('',#28325,2.);
#6652=CYLINDRICAL_SURFACE('',#28328,6.00000000000001);
#6653=CYLINDRICAL_SURFACE('',#28330,5.99999999999999);
#6654=CYLINDRICAL_SURFACE('',#28335,5.5);
#6655=CYLINDRICAL_SURFACE('',#28336,5.5);
#6656=CYLINDRICAL_SURFACE('',#28337,5.5);
#6657=CYLINDRICAL_SURFACE('',#28338,5.5);
#6658=CYLINDRICAL_SURFACE('',#28344,27.5);
#6659=CYLINDRICAL_SURFACE('',#28348,26.01);
#6660=CYLINDRICAL_SURFACE('',#28349,6.00000000000002);
#6661=CYLINDRICAL_SURFACE('',#28351,6.00000000000002);
#6662=CYLINDRICAL_SURFACE('',#28353,6.00000000000002);
#6663=CYLINDRICAL_SURFACE('',#28355,3.99999999999999);
#6664=CYLINDRICAL_SURFACE('',#28357,4.);
#6665=CYLINDRICAL_SURFACE('',#28359,3.99999999999998);
#6666=CYLINDRICAL_SURFACE('',#28361,3.99999999999999);
#6667=CYLINDRICAL_SURFACE('',#28363,3.99999999999998);
#6668=CYLINDRICAL_SURFACE('',#28365,3.99999999999999);
#6669=CYLINDRICAL_SURFACE('',#28367,8.);
#6670=CYLINDRICAL_SURFACE('',#28368,8.);
#6671=CYLINDRICAL_SURFACE('',#28369,22.5);
#6672=CYLINDRICAL_SURFACE('',#28375,70.);
#6673=CYLINDRICAL_SURFACE('',#28905,10.01);
#6674=CYLINDRICAL_SURFACE('',#29068,10.01);
#6675=CYLINDRICAL_SURFACE('',#29077,2.51);
#6676=CYLINDRICAL_SURFACE('',#29082,10.);
#6677=CYLINDRICAL_SURFACE('',#29086,12.5);
#6678=CYLINDRICAL_SURFACE('',#29090,15.);
#6679=CYLINDRICAL_SURFACE('',#29094,12.5);
#6680=CYLINDRICAL_SURFACE('',#29098,11.95);
#6681=CYLINDRICAL_SURFACE('',#29102,12.5);
#6682=CYLINDRICAL_SURFACE('',#29106,10.);
#6683=CYLINDRICAL_SURFACE('',#29123,26.);
#6684=CYLINDRICAL_SURFACE('',#29139,12.5);
#6685=CYLINDRICAL_SURFACE('',#29149,18.);
#6686=CYLINDRICAL_SURFACE('',#29153,10.);
#6687=CYLINDRICAL_SURFACE('',#29159,16.);
#6688=CYLINDRICAL_SURFACE('',#29163,13.);
#6689=CYLINDRICAL_SURFACE('',#29167,13.);
#6690=CYLINDRICAL_SURFACE('',#29174,20.);
#6691=CYLINDRICAL_SURFACE('',#29182,2.5);
#6692=CYLINDRICAL_SURFACE('',#29188,12.55);
#6693=CYLINDRICAL_SURFACE('',#29193,16.);
#6694=CYLINDRICAL_SURFACE('',#29220,16.);
#6695=CYLINDRICAL_SURFACE('',#29221,11.95);
#6696=CYLINDRICAL_SURFACE('',#29247,22.);
#6697=CYLINDRICAL_SURFACE('',#29248,27.5);
#6698=CYLINDRICAL_SURFACE('',#29305,16.7);
#6699=CYLINDRICAL_SURFACE('',#29323,5.00000000000001);
#6700=CYLINDRICAL_SURFACE('',#29326,5.00000000000002);
#6701=CYLINDRICAL_SURFACE('',#29352,5.00000000000004);
#6702=CYLINDRICAL_SURFACE('',#29354,5.00000000000001);
#6703=CYLINDRICAL_SURFACE('',#29376,4.00000000000002);
#6704=CYLINDRICAL_SURFACE('',#29378,4.00000000000002);
#6705=CYLINDRICAL_SURFACE('',#29381,3.99999999999998);
#6706=CYLINDRICAL_SURFACE('',#29383,3.99999999999999);
#6707=CYLINDRICAL_SURFACE('',#29385,2.75);
#6708=CYLINDRICAL_SURFACE('',#29386,2.75);
#6709=CYLINDRICAL_SURFACE('',#29387,2.75);
#6710=CYLINDRICAL_SURFACE('',#29388,2.75);
#6711=CYLINDRICAL_SURFACE('',#29440,25.);
#6712=CYLINDRICAL_SURFACE('',#29483,3.4);
#6713=CYLINDRICAL_SURFACE('',#29493,10.);
#6714=CYLINDRICAL_SURFACE('',#29497,4.925);
#6715=CYLINDRICAL_SURFACE('',#29499,4.925);
#6716=CYLINDRICAL_SURFACE('',#29500,4.925);
#6717=CYLINDRICAL_SURFACE('',#29501,4.925);
#6718=CYLINDRICAL_SURFACE('',#29502,4.925);
#6719=CYLINDRICAL_SURFACE('',#29503,4.925);
#6720=CYLINDRICAL_SURFACE('',#29504,4.925);
#6721=CYLINDRICAL_SURFACE('',#29505,4.925);
#6722=CYLINDRICAL_SURFACE('',#29506,4.925);
#6723=CYLINDRICAL_SURFACE('',#29507,4.925);
#6724=CYLINDRICAL_SURFACE('',#29508,4.925);
#6725=CYLINDRICAL_SURFACE('',#29509,4.925);
#6726=CYLINDRICAL_SURFACE('',#29510,4.925);
#6727=CYLINDRICAL_SURFACE('',#29511,4.925);
#6728=CYLINDRICAL_SURFACE('',#29512,4.925);
#6729=CYLINDRICAL_SURFACE('',#29513,4.925);
#6730=CYLINDRICAL_SURFACE('',#29514,4.925);
#6731=CYLINDRICAL_SURFACE('',#29515,4.925);
#6732=CYLINDRICAL_SURFACE('',#29516,4.925);
#6733=CYLINDRICAL_SURFACE('',#29517,4.925);
#6734=CYLINDRICAL_SURFACE('',#29518,4.0705);
#6735=CYLINDRICAL_SURFACE('',#29520,4.0705);
#6736=CYLINDRICAL_SURFACE('',#29522,4.0705);
#6737=CYLINDRICAL_SURFACE('',#29523,4.0705);
#6738=CYLINDRICAL_SURFACE('',#29524,4.0705);
#6739=CYLINDRICAL_SURFACE('',#29525,4.0705);
#6740=CYLINDRICAL_SURFACE('',#29526,4.0705);
#6741=CYLINDRICAL_SURFACE('',#29527,4.0705);
#6742=CYLINDRICAL_SURFACE('',#29528,4.0705);
#6743=CYLINDRICAL_SURFACE('',#29529,4.0705);
#6744=CYLINDRICAL_SURFACE('',#29530,4.0705);
#6745=CYLINDRICAL_SURFACE('',#29531,4.0705);
#6746=CYLINDRICAL_SURFACE('',#29532,4.0705);
#6747=CYLINDRICAL_SURFACE('',#29533,4.0705);
#6748=CYLINDRICAL_SURFACE('',#29534,4.0705);
#6749=CYLINDRICAL_SURFACE('',#29535,4.0705);
#6750=CYLINDRICAL_SURFACE('',#29536,4.0705);
#6751=CYLINDRICAL_SURFACE('',#29537,4.0705);
#6752=CYLINDRICAL_SURFACE('',#29538,4.0705);
#6753=CYLINDRICAL_SURFACE('',#29539,4.0705);
#6754=CYLINDRICAL_SURFACE('',#29544,4.0705);
#6755=CYLINDRICAL_SURFACE('',#29559,4.925);
#6756=CYLINDRICAL_SURFACE('',#29561,4.925);
#6757=CYLINDRICAL_SURFACE('',#29563,4.925);
#6758=CYLINDRICAL_SURFACE('',#29564,4.925);
#6759=CYLINDRICAL_SURFACE('',#29565,4.925);
#6760=CYLINDRICAL_SURFACE('',#29566,4.925);
#6761=CYLINDRICAL_SURFACE('',#29567,4.925);
#6762=CYLINDRICAL_SURFACE('',#29568,4.925);
#6763=CYLINDRICAL_SURFACE('',#29569,4.925);
#6764=CYLINDRICAL_SURFACE('',#29570,4.925);
#6765=CYLINDRICAL_SURFACE('',#29571,4.925);
#6766=CYLINDRICAL_SURFACE('',#29572,4.925);
#6767=CYLINDRICAL_SURFACE('',#29573,4.925);
#6768=CYLINDRICAL_SURFACE('',#29574,4.925);
#6769=CYLINDRICAL_SURFACE('',#29575,4.925);
#6770=CYLINDRICAL_SURFACE('',#29576,4.925);
#6771=CYLINDRICAL_SURFACE('',#29577,4.925);
#6772=CYLINDRICAL_SURFACE('',#29578,4.925);
#6773=CYLINDRICAL_SURFACE('',#29579,4.925);
#6774=CYLINDRICAL_SURFACE('',#29580,4.925);
#6775=CYLINDRICAL_SURFACE('',#29581,4.925);
#6776=CYLINDRICAL_SURFACE('',#29582,4.0705);
#6777=CYLINDRICAL_SURFACE('',#29584,4.0705);
#6778=CYLINDRICAL_SURFACE('',#29586,4.0705);
#6779=CYLINDRICAL_SURFACE('',#29587,4.0705);
#6780=CYLINDRICAL_SURFACE('',#29588,4.0705);
#6781=CYLINDRICAL_SURFACE('',#29589,4.0705);
#6782=CYLINDRICAL_SURFACE('',#29590,4.0705);
#6783=CYLINDRICAL_SURFACE('',#29591,4.0705);
#6784=CYLINDRICAL_SURFACE('',#29592,4.0705);
#6785=CYLINDRICAL_SURFACE('',#29593,4.0705);
#6786=CYLINDRICAL_SURFACE('',#29594,4.0705);
#6787=CYLINDRICAL_SURFACE('',#29595,4.0705);
#6788=CYLINDRICAL_SURFACE('',#29596,4.0705);
#6789=CYLINDRICAL_SURFACE('',#29597,4.0705);
#6790=CYLINDRICAL_SURFACE('',#29598,4.0705);
#6791=CYLINDRICAL_SURFACE('',#29599,4.0705);
#6792=CYLINDRICAL_SURFACE('',#29600,4.0705);
#6793=CYLINDRICAL_SURFACE('',#29601,4.0705);
#6794=CYLINDRICAL_SURFACE('',#29602,4.0705);
#6795=CYLINDRICAL_SURFACE('',#29603,4.0705);
#6796=CYLINDRICAL_SURFACE('',#29608,4.0705);
#6797=CYLINDRICAL_SURFACE('',#29837,4.925);
#6798=CYLINDRICAL_SURFACE('',#29841,8.);
#6799=CYLINDRICAL_SURFACE('',#29891,6.85);
#6800=CYLINDRICAL_SURFACE('',#29893,2.4505);
#6801=CYLINDRICAL_SURFACE('',#29895,2.4505);
#6802=CYLINDRICAL_SURFACE('',#29896,2.4505);
#6803=CYLINDRICAL_SURFACE('',#29897,2.4505);
#6804=CYLINDRICAL_SURFACE('',#29898,2.4505);
#6805=CYLINDRICAL_SURFACE('',#29899,2.4505);
#6806=CYLINDRICAL_SURFACE('',#29900,2.4505);
#6807=CYLINDRICAL_SURFACE('',#29901,2.4505);
#6808=CYLINDRICAL_SURFACE('',#29902,2.4505);
#6809=CYLINDRICAL_SURFACE('',#29903,2.4505);
#6810=CYLINDRICAL_SURFACE('',#29904,2.4505);
#6811=CYLINDRICAL_SURFACE('',#29905,2.4505);
#6812=CYLINDRICAL_SURFACE('',#29906,2.4505);
#6813=CYLINDRICAL_SURFACE('',#29908,1.99475);
#6814=CYLINDRICAL_SURFACE('',#29910,1.99475);
#6815=CYLINDRICAL_SURFACE('',#29911,1.99475);
#6816=CYLINDRICAL_SURFACE('',#29912,1.99475);
#6817=CYLINDRICAL_SURFACE('',#29913,1.99475);
#6818=CYLINDRICAL_SURFACE('',#29914,1.99475);
#6819=CYLINDRICAL_SURFACE('',#29915,1.99475);
#6820=CYLINDRICAL_SURFACE('',#29916,1.99475);
#6821=CYLINDRICAL_SURFACE('',#29917,1.99475);
#6822=CYLINDRICAL_SURFACE('',#29918,1.99475);
#6823=CYLINDRICAL_SURFACE('',#29919,1.99475);
#6824=CYLINDRICAL_SURFACE('',#29920,1.99475);
#6825=CYLINDRICAL_SURFACE('',#29925,1.99475);
#6826=CYLINDRICAL_SURFACE('',#29936,2.4505);
#6827=FACE_OUTER_BOUND('',#8397,.T.);
#6828=FACE_OUTER_BOUND('',#8398,.T.);
#6829=FACE_OUTER_BOUND('',#8399,.T.);
#6830=FACE_OUTER_BOUND('',#8405,.T.);
#6831=FACE_OUTER_BOUND('',#8406,.T.);
#6832=FACE_OUTER_BOUND('',#8416,.T.);
#6833=FACE_OUTER_BOUND('',#8417,.T.);
#6834=FACE_OUTER_BOUND('',#8418,.T.);
#6835=FACE_OUTER_BOUND('',#8419,.T.);
#6836=FACE_OUTER_BOUND('',#8420,.T.);
#6837=FACE_OUTER_BOUND('',#8421,.T.);
#6838=FACE_OUTER_BOUND('',#8422,.T.);
#6839=FACE_OUTER_BOUND('',#8423,.T.);
#6840=FACE_OUTER_BOUND('',#8424,.T.);
#6841=FACE_OUTER_BOUND('',#8425,.T.);
#6842=FACE_OUTER_BOUND('',#8426,.T.);
#6843=FACE_OUTER_BOUND('',#8427,.T.);
#6844=FACE_OUTER_BOUND('',#8428,.T.);
#6845=FACE_OUTER_BOUND('',#8431,.T.);
#6846=FACE_OUTER_BOUND('',#8432,.T.);
#6847=FACE_OUTER_BOUND('',#8433,.T.);
#6848=FACE_OUTER_BOUND('',#8434,.T.);
#6849=FACE_OUTER_BOUND('',#8435,.T.);
#6850=FACE_OUTER_BOUND('',#8436,.T.);
#6851=FACE_OUTER_BOUND('',#8437,.T.);
#6852=FACE_OUTER_BOUND('',#8438,.T.);
#6853=FACE_OUTER_BOUND('',#8439,.T.);
#6854=FACE_OUTER_BOUND('',#8440,.T.);
#6855=FACE_OUTER_BOUND('',#8441,.T.);
#6856=FACE_OUTER_BOUND('',#8442,.T.);
#6857=FACE_OUTER_BOUND('',#8446,.T.);
#6858=FACE_OUTER_BOUND('',#8447,.T.);
#6859=FACE_OUTER_BOUND('',#8448,.T.);
#6860=FACE_OUTER_BOUND('',#8449,.T.);
#6861=FACE_OUTER_BOUND('',#8450,.T.);
#6862=FACE_OUTER_BOUND('',#8451,.T.);
#6863=FACE_OUTER_BOUND('',#8452,.T.);
#6864=FACE_OUTER_BOUND('',#8453,.T.);
#6865=FACE_OUTER_BOUND('',#8454,.T.);
#6866=FACE_OUTER_BOUND('',#8455,.T.);
#6867=FACE_OUTER_BOUND('',#8456,.T.);
#6868=FACE_OUTER_BOUND('',#8457,.T.);
#6869=FACE_OUTER_BOUND('',#8458,.T.);
#6870=FACE_OUTER_BOUND('',#8460,.T.);
#6871=FACE_OUTER_BOUND('',#8461,.T.);
#6872=FACE_OUTER_BOUND('',#8462,.T.);
#6873=FACE_OUTER_BOUND('',#8463,.T.);
#6874=FACE_OUTER_BOUND('',#8464,.T.);
#6875=FACE_OUTER_BOUND('',#8465,.T.);
#6876=FACE_OUTER_BOUND('',#8466,.T.);
#6877=FACE_OUTER_BOUND('',#8467,.T.);
#6878=FACE_OUTER_BOUND('',#8468,.T.);
#6879=FACE_OUTER_BOUND('',#8469,.T.);
#6880=FACE_OUTER_BOUND('',#8470,.T.);
#6881=FACE_OUTER_BOUND('',#8471,.T.);
#6882=FACE_OUTER_BOUND('',#8472,.T.);
#6883=FACE_OUTER_BOUND('',#8474,.T.);
#6884=FACE_OUTER_BOUND('',#8475,.T.);
#6885=FACE_OUTER_BOUND('',#8476,.T.);
#6886=FACE_OUTER_BOUND('',#8477,.T.);
#6887=FACE_OUTER_BOUND('',#8479,.T.);
#6888=FACE_OUTER_BOUND('',#8480,.T.);
#6889=FACE_OUTER_BOUND('',#8481,.T.);
#6890=FACE_OUTER_BOUND('',#8482,.T.);
#6891=FACE_OUTER_BOUND('',#8483,.T.);
#6892=FACE_OUTER_BOUND('',#8484,.T.);
#6893=FACE_OUTER_BOUND('',#8485,.T.);
#6894=FACE_OUTER_BOUND('',#8486,.T.);
#6895=FACE_OUTER_BOUND('',#8487,.T.);
#6896=FACE_OUTER_BOUND('',#8488,.T.);
#6897=FACE_OUTER_BOUND('',#8489,.T.);
#6898=FACE_OUTER_BOUND('',#8490,.T.);
#6899=FACE_OUTER_BOUND('',#8491,.T.);
#6900=FACE_OUTER_BOUND('',#8492,.T.);
#6901=FACE_OUTER_BOUND('',#8493,.T.);
#6902=FACE_OUTER_BOUND('',#8494,.T.);
#6903=FACE_OUTER_BOUND('',#8495,.T.);
#6904=FACE_OUTER_BOUND('',#8496,.T.);
#6905=FACE_OUTER_BOUND('',#8497,.T.);
#6906=FACE_OUTER_BOUND('',#8498,.T.);
#6907=FACE_OUTER_BOUND('',#8499,.T.);
#6908=FACE_OUTER_BOUND('',#8500,.T.);
#6909=FACE_OUTER_BOUND('',#8501,.T.);
#6910=FACE_OUTER_BOUND('',#8502,.T.);
#6911=FACE_OUTER_BOUND('',#8503,.T.);
#6912=FACE_OUTER_BOUND('',#8504,.T.);
#6913=FACE_OUTER_BOUND('',#8505,.T.);
#6914=FACE_OUTER_BOUND('',#8506,.T.);
#6915=FACE_OUTER_BOUND('',#8507,.T.);
#6916=FACE_OUTER_BOUND('',#8508,.T.);
#6917=FACE_OUTER_BOUND('',#8509,.T.);
#6918=FACE_OUTER_BOUND('',#8510,.T.);
#6919=FACE_OUTER_BOUND('',#8514,.T.);
#6920=FACE_OUTER_BOUND('',#8515,.T.);
#6921=FACE_OUTER_BOUND('',#8516,.T.);
#6922=FACE_OUTER_BOUND('',#8517,.T.);
#6923=FACE_OUTER_BOUND('',#8518,.T.);
#6924=FACE_OUTER_BOUND('',#8519,.T.);
#6925=FACE_OUTER_BOUND('',#8520,.T.);
#6926=FACE_OUTER_BOUND('',#8521,.T.);
#6927=FACE_OUTER_BOUND('',#8522,.T.);
#6928=FACE_OUTER_BOUND('',#8523,.T.);
#6929=FACE_OUTER_BOUND('',#8524,.T.);
#6930=FACE_OUTER_BOUND('',#8525,.T.);
#6931=FACE_OUTER_BOUND('',#8526,.T.);
#6932=FACE_OUTER_BOUND('',#8527,.T.);
#6933=FACE_OUTER_BOUND('',#8528,.T.);
#6934=FACE_OUTER_BOUND('',#8529,.T.);
#6935=FACE_OUTER_BOUND('',#8530,.T.);
#6936=FACE_OUTER_BOUND('',#8531,.T.);
#6937=FACE_OUTER_BOUND('',#8532,.T.);
#6938=FACE_OUTER_BOUND('',#8533,.T.);
#6939=FACE_OUTER_BOUND('',#8534,.T.);
#6940=FACE_OUTER_BOUND('',#8535,.T.);
#6941=FACE_OUTER_BOUND('',#8536,.T.);
#6942=FACE_OUTER_BOUND('',#8537,.T.);
#6943=FACE_OUTER_BOUND('',#8538,.T.);
#6944=FACE_OUTER_BOUND('',#8539,.T.);
#6945=FACE_OUTER_BOUND('',#8540,.T.);
#6946=FACE_OUTER_BOUND('',#8541,.T.);
#6947=FACE_OUTER_BOUND('',#8542,.T.);
#6948=FACE_OUTER_BOUND('',#8543,.T.);
#6949=FACE_OUTER_BOUND('',#8544,.T.);
#6950=FACE_OUTER_BOUND('',#8545,.T.);
#6951=FACE_OUTER_BOUND('',#8546,.T.);
#6952=FACE_OUTER_BOUND('',#8547,.T.);
#6953=FACE_OUTER_BOUND('',#8548,.T.);
#6954=FACE_OUTER_BOUND('',#8549,.T.);
#6955=FACE_OUTER_BOUND('',#8550,.T.);
#6956=FACE_OUTER_BOUND('',#8551,.T.);
#6957=FACE_OUTER_BOUND('',#8552,.T.);
#6958=FACE_OUTER_BOUND('',#8553,.T.);
#6959=FACE_OUTER_BOUND('',#8554,.T.);
#6960=FACE_OUTER_BOUND('',#8555,.T.);
#6961=FACE_OUTER_BOUND('',#8556,.T.);
#6962=FACE_OUTER_BOUND('',#8557,.T.);
#6963=FACE_OUTER_BOUND('',#8559,.T.);
#6964=FACE_OUTER_BOUND('',#8560,.T.);
#6965=FACE_OUTER_BOUND('',#8561,.T.);
#6966=FACE_OUTER_BOUND('',#8562,.T.);
#6967=FACE_OUTER_BOUND('',#8563,.T.);
#6968=FACE_OUTER_BOUND('',#8564,.T.);
#6969=FACE_OUTER_BOUND('',#8565,.T.);
#6970=FACE_OUTER_BOUND('',#8566,.T.);
#6971=FACE_OUTER_BOUND('',#8567,.T.);
#6972=FACE_OUTER_BOUND('',#8568,.T.);
#6973=FACE_OUTER_BOUND('',#8569,.T.);
#6974=FACE_OUTER_BOUND('',#8570,.T.);
#6975=FACE_OUTER_BOUND('',#8571,.T.);
#6976=FACE_OUTER_BOUND('',#8572,.T.);
#6977=FACE_OUTER_BOUND('',#8573,.T.);
#6978=FACE_OUTER_BOUND('',#8574,.T.);
#6979=FACE_OUTER_BOUND('',#8575,.T.);
#6980=FACE_OUTER_BOUND('',#8576,.T.);
#6981=FACE_OUTER_BOUND('',#8577,.T.);
#6982=FACE_OUTER_BOUND('',#8578,.T.);
#6983=FACE_OUTER_BOUND('',#8579,.T.);
#6984=FACE_OUTER_BOUND('',#8580,.T.);
#6985=FACE_OUTER_BOUND('',#8581,.T.);
#6986=FACE_OUTER_BOUND('',#8582,.T.);
#6987=FACE_OUTER_BOUND('',#8583,.T.);
#6988=FACE_OUTER_BOUND('',#8584,.T.);
#6989=FACE_OUTER_BOUND('',#8585,.T.);
#6990=FACE_OUTER_BOUND('',#8586,.T.);
#6991=FACE_OUTER_BOUND('',#8587,.T.);
#6992=FACE_OUTER_BOUND('',#8588,.T.);
#6993=FACE_OUTER_BOUND('',#8589,.T.);
#6994=FACE_OUTER_BOUND('',#8590,.T.);
#6995=FACE_OUTER_BOUND('',#8591,.T.);
#6996=FACE_OUTER_BOUND('',#8592,.T.);
#6997=FACE_OUTER_BOUND('',#8593,.T.);
#6998=FACE_OUTER_BOUND('',#8594,.T.);
#6999=FACE_OUTER_BOUND('',#8595,.T.);
#7000=FACE_OUTER_BOUND('',#8596,.T.);
#7001=FACE_OUTER_BOUND('',#8597,.T.);
#7002=FACE_OUTER_BOUND('',#8598,.T.);
#7003=FACE_OUTER_BOUND('',#8599,.T.);
#7004=FACE_OUTER_BOUND('',#8600,.T.);
#7005=FACE_OUTER_BOUND('',#8601,.T.);
#7006=FACE_OUTER_BOUND('',#8602,.T.);
#7007=FACE_OUTER_BOUND('',#8603,.T.);
#7008=FACE_OUTER_BOUND('',#8604,.T.);
#7009=FACE_OUTER_BOUND('',#8605,.T.);
#7010=FACE_OUTER_BOUND('',#8606,.T.);
#7011=FACE_OUTER_BOUND('',#8607,.T.);
#7012=FACE_OUTER_BOUND('',#8608,.T.);
#7013=FACE_OUTER_BOUND('',#8609,.T.);
#7014=FACE_OUTER_BOUND('',#8610,.T.);
#7015=FACE_OUTER_BOUND('',#8611,.T.);
#7016=FACE_OUTER_BOUND('',#8612,.T.);
#7017=FACE_OUTER_BOUND('',#8613,.T.);
#7018=FACE_OUTER_BOUND('',#8614,.T.);
#7019=FACE_OUTER_BOUND('',#8615,.T.);
#7020=FACE_OUTER_BOUND('',#8616,.T.);
#7021=FACE_OUTER_BOUND('',#8617,.T.);
#7022=FACE_OUTER_BOUND('',#8618,.T.);
#7023=FACE_OUTER_BOUND('',#8619,.T.);
#7024=FACE_OUTER_BOUND('',#8620,.T.);
#7025=FACE_OUTER_BOUND('',#8621,.T.);
#7026=FACE_OUTER_BOUND('',#8622,.T.);
#7027=FACE_OUTER_BOUND('',#8623,.T.);
#7028=FACE_OUTER_BOUND('',#8633,.T.);
#7029=FACE_OUTER_BOUND('',#8634,.T.);
#7030=FACE_OUTER_BOUND('',#8635,.T.);
#7031=FACE_OUTER_BOUND('',#8636,.T.);
#7032=FACE_OUTER_BOUND('',#8637,.T.);
#7033=FACE_OUTER_BOUND('',#8638,.T.);
#7034=FACE_OUTER_BOUND('',#8640,.T.);
#7035=FACE_OUTER_BOUND('',#8641,.T.);
#7036=FACE_OUTER_BOUND('',#8642,.T.);
#7037=FACE_OUTER_BOUND('',#8648,.T.);
#7038=FACE_OUTER_BOUND('',#8649,.T.);
#7039=FACE_OUTER_BOUND('',#8650,.T.);
#7040=FACE_OUTER_BOUND('',#8651,.T.);
#7041=FACE_OUTER_BOUND('',#8652,.T.);
#7042=FACE_OUTER_BOUND('',#8653,.T.);
#7043=FACE_OUTER_BOUND('',#8654,.T.);
#7044=FACE_OUTER_BOUND('',#8655,.T.);
#7045=FACE_OUTER_BOUND('',#8656,.T.);
#7046=FACE_OUTER_BOUND('',#8657,.T.);
#7047=FACE_OUTER_BOUND('',#8658,.T.);
#7048=FACE_OUTER_BOUND('',#8659,.T.);
#7049=FACE_OUTER_BOUND('',#8660,.T.);
#7050=FACE_OUTER_BOUND('',#8661,.T.);
#7051=FACE_OUTER_BOUND('',#8662,.T.);
#7052=FACE_OUTER_BOUND('',#8663,.T.);
#7053=FACE_OUTER_BOUND('',#8664,.T.);
#7054=FACE_OUTER_BOUND('',#8665,.T.);
#7055=FACE_OUTER_BOUND('',#8666,.T.);
#7056=FACE_OUTER_BOUND('',#8667,.T.);
#7057=FACE_OUTER_BOUND('',#8668,.T.);
#7058=FACE_OUTER_BOUND('',#8669,.T.);
#7059=FACE_OUTER_BOUND('',#8670,.T.);
#7060=FACE_OUTER_BOUND('',#8671,.T.);
#7061=FACE_OUTER_BOUND('',#8672,.T.);
#7062=FACE_OUTER_BOUND('',#8673,.T.);
#7063=FACE_OUTER_BOUND('',#8674,.T.);
#7064=FACE_OUTER_BOUND('',#8675,.T.);
#7065=FACE_OUTER_BOUND('',#8676,.T.);
#7066=FACE_OUTER_BOUND('',#8677,.T.);
#7067=FACE_OUTER_BOUND('',#8678,.T.);
#7068=FACE_OUTER_BOUND('',#8679,.T.);
#7069=FACE_OUTER_BOUND('',#8680,.T.);
#7070=FACE_OUTER_BOUND('',#8681,.T.);
#7071=FACE_OUTER_BOUND('',#8682,.T.);
#7072=FACE_OUTER_BOUND('',#8683,.T.);
#7073=FACE_OUTER_BOUND('',#8684,.T.);
#7074=FACE_OUTER_BOUND('',#8685,.T.);
#7075=FACE_OUTER_BOUND('',#8686,.T.);
#7076=FACE_OUTER_BOUND('',#8687,.T.);
#7077=FACE_OUTER_BOUND('',#8688,.T.);
#7078=FACE_OUTER_BOUND('',#8689,.T.);
#7079=FACE_OUTER_BOUND('',#8690,.T.);
#7080=FACE_OUTER_BOUND('',#8691,.T.);
#7081=FACE_OUTER_BOUND('',#8692,.T.);
#7082=FACE_OUTER_BOUND('',#8693,.T.);
#7083=FACE_OUTER_BOUND('',#8694,.T.);
#7084=FACE_OUTER_BOUND('',#8695,.T.);
#7085=FACE_OUTER_BOUND('',#8696,.T.);
#7086=FACE_OUTER_BOUND('',#8697,.T.);
#7087=FACE_OUTER_BOUND('',#8698,.T.);
#7088=FACE_OUTER_BOUND('',#8699,.T.);
#7089=FACE_OUTER_BOUND('',#8700,.T.);
#7090=FACE_OUTER_BOUND('',#8701,.T.);
#7091=FACE_OUTER_BOUND('',#8702,.T.);
#7092=FACE_OUTER_BOUND('',#8703,.T.);
#7093=FACE_OUTER_BOUND('',#8704,.T.);
#7094=FACE_OUTER_BOUND('',#8705,.T.);
#7095=FACE_OUTER_BOUND('',#8706,.T.);
#7096=FACE_OUTER_BOUND('',#8707,.T.);
#7097=FACE_OUTER_BOUND('',#8708,.T.);
#7098=FACE_OUTER_BOUND('',#8709,.T.);
#7099=FACE_OUTER_BOUND('',#8710,.T.);
#7100=FACE_OUTER_BOUND('',#8711,.T.);
#7101=FACE_OUTER_BOUND('',#8712,.T.);
#7102=FACE_OUTER_BOUND('',#8713,.T.);
#7103=FACE_OUTER_BOUND('',#8714,.T.);
#7104=FACE_OUTER_BOUND('',#8715,.T.);
#7105=FACE_OUTER_BOUND('',#8716,.T.);
#7106=FACE_OUTER_BOUND('',#8717,.T.);
#7107=FACE_OUTER_BOUND('',#8718,.T.);
#7108=FACE_OUTER_BOUND('',#8719,.T.);
#7109=FACE_OUTER_BOUND('',#8720,.T.);
#7110=FACE_OUTER_BOUND('',#8721,.T.);
#7111=FACE_OUTER_BOUND('',#8722,.T.);
#7112=FACE_OUTER_BOUND('',#8723,.T.);
#7113=FACE_OUTER_BOUND('',#8724,.T.);
#7114=FACE_OUTER_BOUND('',#8725,.T.);
#7115=FACE_OUTER_BOUND('',#8726,.T.);
#7116=FACE_OUTER_BOUND('',#8727,.T.);
#7117=FACE_OUTER_BOUND('',#8728,.T.);
#7118=FACE_OUTER_BOUND('',#8729,.T.);
#7119=FACE_OUTER_BOUND('',#8730,.T.);
#7120=FACE_OUTER_BOUND('',#8731,.T.);
#7121=FACE_OUTER_BOUND('',#8732,.T.);
#7122=FACE_OUTER_BOUND('',#8733,.T.);
#7123=FACE_OUTER_BOUND('',#8734,.T.);
#7124=FACE_OUTER_BOUND('',#8735,.T.);
#7125=FACE_OUTER_BOUND('',#8736,.T.);
#7126=FACE_OUTER_BOUND('',#8737,.T.);
#7127=FACE_OUTER_BOUND('',#8738,.T.);
#7128=FACE_OUTER_BOUND('',#8739,.T.);
#7129=FACE_OUTER_BOUND('',#8740,.T.);
#7130=FACE_OUTER_BOUND('',#8741,.T.);
#7131=FACE_OUTER_BOUND('',#8742,.T.);
#7132=FACE_OUTER_BOUND('',#8743,.T.);
#7133=FACE_OUTER_BOUND('',#8744,.T.);
#7134=FACE_OUTER_BOUND('',#8745,.T.);
#7135=FACE_OUTER_BOUND('',#8746,.T.);
#7136=FACE_OUTER_BOUND('',#8747,.T.);
#7137=FACE_OUTER_BOUND('',#8748,.T.);
#7138=FACE_OUTER_BOUND('',#8749,.T.);
#7139=FACE_OUTER_BOUND('',#8750,.T.);
#7140=FACE_OUTER_BOUND('',#8751,.T.);
#7141=FACE_OUTER_BOUND('',#8752,.T.);
#7142=FACE_OUTER_BOUND('',#8753,.T.);
#7143=FACE_OUTER_BOUND('',#8754,.T.);
#7144=FACE_OUTER_BOUND('',#8755,.T.);
#7145=FACE_OUTER_BOUND('',#8756,.T.);
#7146=FACE_OUTER_BOUND('',#8757,.T.);
#7147=FACE_OUTER_BOUND('',#8758,.T.);
#7148=FACE_OUTER_BOUND('',#8759,.T.);
#7149=FACE_OUTER_BOUND('',#8760,.T.);
#7150=FACE_OUTER_BOUND('',#8761,.T.);
#7151=FACE_OUTER_BOUND('',#8762,.T.);
#7152=FACE_OUTER_BOUND('',#8763,.T.);
#7153=FACE_OUTER_BOUND('',#8764,.T.);
#7154=FACE_OUTER_BOUND('',#8765,.T.);
#7155=FACE_OUTER_BOUND('',#8766,.T.);
#7156=FACE_OUTER_BOUND('',#8767,.T.);
#7157=FACE_OUTER_BOUND('',#8768,.T.);
#7158=FACE_OUTER_BOUND('',#8769,.T.);
#7159=FACE_OUTER_BOUND('',#8770,.T.);
#7160=FACE_OUTER_BOUND('',#8771,.T.);
#7161=FACE_OUTER_BOUND('',#8772,.T.);
#7162=FACE_OUTER_BOUND('',#8773,.T.);
#7163=FACE_OUTER_BOUND('',#8774,.T.);
#7164=FACE_OUTER_BOUND('',#8775,.T.);
#7165=FACE_OUTER_BOUND('',#8776,.T.);
#7166=FACE_OUTER_BOUND('',#8777,.T.);
#7167=FACE_OUTER_BOUND('',#8779,.T.);
#7168=FACE_OUTER_BOUND('',#8780,.T.);
#7169=FACE_OUTER_BOUND('',#8781,.T.);
#7170=FACE_OUTER_BOUND('',#8782,.T.);
#7171=FACE_OUTER_BOUND('',#8783,.T.);
#7172=FACE_OUTER_BOUND('',#8784,.T.);
#7173=FACE_OUTER_BOUND('',#8785,.T.);
#7174=FACE_OUTER_BOUND('',#8786,.T.);
#7175=FACE_OUTER_BOUND('',#8788,.T.);
#7176=FACE_OUTER_BOUND('',#8789,.T.);
#7177=FACE_OUTER_BOUND('',#8791,.T.);
#7178=FACE_OUTER_BOUND('',#8792,.T.);
#7179=FACE_OUTER_BOUND('',#8796,.T.);
#7180=FACE_OUTER_BOUND('',#8797,.T.);
#7181=FACE_OUTER_BOUND('',#8798,.T.);
#7182=FACE_OUTER_BOUND('',#8799,.T.);
#7183=FACE_OUTER_BOUND('',#8800,.T.);
#7184=FACE_OUTER_BOUND('',#8801,.T.);
#7185=FACE_OUTER_BOUND('',#8803,.T.);
#7186=FACE_OUTER_BOUND('',#8804,.T.);
#7187=FACE_OUTER_BOUND('',#8805,.T.);
#7188=FACE_OUTER_BOUND('',#8806,.T.);
#7189=FACE_OUTER_BOUND('',#8807,.T.);
#7190=FACE_OUTER_BOUND('',#8808,.T.);
#7191=FACE_OUTER_BOUND('',#8809,.T.);
#7192=FACE_OUTER_BOUND('',#8810,.T.);
#7193=FACE_OUTER_BOUND('',#8811,.T.);
#7194=FACE_OUTER_BOUND('',#8812,.T.);
#7195=FACE_OUTER_BOUND('',#8813,.T.);
#7196=FACE_OUTER_BOUND('',#8814,.T.);
#7197=FACE_OUTER_BOUND('',#8815,.T.);
#7198=FACE_OUTER_BOUND('',#8821,.T.);
#7199=FACE_OUTER_BOUND('',#8822,.T.);
#7200=FACE_OUTER_BOUND('',#8823,.T.);
#7201=FACE_OUTER_BOUND('',#8824,.T.);
#7202=FACE_OUTER_BOUND('',#8825,.T.);
#7203=FACE_OUTER_BOUND('',#8831,.T.);
#7204=FACE_OUTER_BOUND('',#8832,.T.);
#7205=FACE_OUTER_BOUND('',#8833,.T.);
#7206=FACE_OUTER_BOUND('',#8834,.T.);
#7207=FACE_OUTER_BOUND('',#8835,.T.);
#7208=FACE_OUTER_BOUND('',#8836,.T.);
#7209=FACE_OUTER_BOUND('',#8837,.T.);
#7210=FACE_OUTER_BOUND('',#8838,.T.);
#7211=FACE_OUTER_BOUND('',#8839,.T.);
#7212=FACE_OUTER_BOUND('',#8842,.T.);
#7213=FACE_OUTER_BOUND('',#8843,.T.);
#7214=FACE_OUTER_BOUND('',#8844,.T.);
#7215=FACE_OUTER_BOUND('',#8845,.T.);
#7216=FACE_OUTER_BOUND('',#8851,.T.);
#7217=FACE_OUTER_BOUND('',#8852,.T.);
#7218=FACE_OUTER_BOUND('',#8858,.T.);
#7219=FACE_OUTER_BOUND('',#8859,.T.);
#7220=FACE_OUTER_BOUND('',#8860,.T.);
#7221=FACE_OUTER_BOUND('',#8861,.T.);
#7222=FACE_OUTER_BOUND('',#8862,.T.);
#7223=FACE_OUTER_BOUND('',#8863,.T.);
#7224=FACE_OUTER_BOUND('',#8864,.T.);
#7225=FACE_OUTER_BOUND('',#8865,.T.);
#7226=FACE_OUTER_BOUND('',#8866,.T.);
#7227=FACE_OUTER_BOUND('',#8867,.T.);
#7228=FACE_OUTER_BOUND('',#8868,.T.);
#7229=FACE_OUTER_BOUND('',#8869,.T.);
#7230=FACE_OUTER_BOUND('',#8870,.T.);
#7231=FACE_OUTER_BOUND('',#8871,.T.);
#7232=FACE_OUTER_BOUND('',#8872,.T.);
#7233=FACE_OUTER_BOUND('',#8873,.T.);
#7234=FACE_OUTER_BOUND('',#8874,.T.);
#7235=FACE_OUTER_BOUND('',#8875,.T.);
#7236=FACE_OUTER_BOUND('',#8876,.T.);
#7237=FACE_OUTER_BOUND('',#8877,.T.);
#7238=FACE_OUTER_BOUND('',#8878,.T.);
#7239=FACE_OUTER_BOUND('',#8879,.T.);
#7240=FACE_OUTER_BOUND('',#8880,.T.);
#7241=FACE_OUTER_BOUND('',#8881,.T.);
#7242=FACE_OUTER_BOUND('',#8882,.T.);
#7243=FACE_OUTER_BOUND('',#8883,.T.);
#7244=FACE_OUTER_BOUND('',#8884,.T.);
#7245=FACE_OUTER_BOUND('',#8885,.T.);
#7246=FACE_OUTER_BOUND('',#8886,.T.);
#7247=FACE_OUTER_BOUND('',#8887,.T.);
#7248=FACE_OUTER_BOUND('',#8888,.T.);
#7249=FACE_OUTER_BOUND('',#8889,.T.);
#7250=FACE_OUTER_BOUND('',#8890,.T.);
#7251=FACE_OUTER_BOUND('',#8891,.T.);
#7252=FACE_OUTER_BOUND('',#8892,.T.);
#7253=FACE_OUTER_BOUND('',#8894,.T.);
#7254=FACE_OUTER_BOUND('',#8895,.T.);
#7255=FACE_OUTER_BOUND('',#8896,.T.);
#7256=FACE_OUTER_BOUND('',#8897,.T.);
#7257=FACE_OUTER_BOUND('',#8898,.T.);
#7258=FACE_OUTER_BOUND('',#8899,.T.);
#7259=FACE_OUTER_BOUND('',#8900,.T.);
#7260=FACE_OUTER_BOUND('',#8901,.T.);
#7261=FACE_OUTER_BOUND('',#8902,.T.);
#7262=FACE_OUTER_BOUND('',#8903,.T.);
#7263=FACE_OUTER_BOUND('',#8904,.T.);
#7264=FACE_OUTER_BOUND('',#8905,.T.);
#7265=FACE_OUTER_BOUND('',#8906,.T.);
#7266=FACE_OUTER_BOUND('',#8908,.T.);
#7267=FACE_OUTER_BOUND('',#8909,.T.);
#7268=FACE_OUTER_BOUND('',#8910,.T.);
#7269=FACE_OUTER_BOUND('',#8911,.T.);
#7270=FACE_OUTER_BOUND('',#8912,.T.);
#7271=FACE_OUTER_BOUND('',#8913,.T.);
#7272=FACE_OUTER_BOUND('',#8914,.T.);
#7273=FACE_OUTER_BOUND('',#8915,.T.);
#7274=FACE_OUTER_BOUND('',#8916,.T.);
#7275=FACE_OUTER_BOUND('',#8917,.T.);
#7276=FACE_OUTER_BOUND('',#8918,.T.);
#7277=FACE_OUTER_BOUND('',#8919,.T.);
#7278=FACE_OUTER_BOUND('',#8921,.T.);
#7279=FACE_OUTER_BOUND('',#8922,.T.);
#7280=FACE_OUTER_BOUND('',#8923,.T.);
#7281=FACE_OUTER_BOUND('',#8924,.T.);
#7282=FACE_OUTER_BOUND('',#8925,.T.);
#7283=FACE_OUTER_BOUND('',#8926,.T.);
#7284=FACE_OUTER_BOUND('',#8927,.T.);
#7285=FACE_OUTER_BOUND('',#8928,.T.);
#7286=FACE_OUTER_BOUND('',#8929,.T.);
#7287=FACE_OUTER_BOUND('',#8930,.T.);
#7288=FACE_OUTER_BOUND('',#8931,.T.);
#7289=FACE_OUTER_BOUND('',#8932,.T.);
#7290=FACE_OUTER_BOUND('',#8934,.T.);
#7291=FACE_OUTER_BOUND('',#8935,.T.);
#7292=FACE_OUTER_BOUND('',#8936,.T.);
#7293=FACE_OUTER_BOUND('',#8937,.T.);
#7294=FACE_OUTER_BOUND('',#8938,.T.);
#7295=FACE_OUTER_BOUND('',#8939,.T.);
#7296=FACE_OUTER_BOUND('',#8940,.T.);
#7297=FACE_OUTER_BOUND('',#8941,.T.);
#7298=FACE_OUTER_BOUND('',#8942,.T.);
#7299=FACE_OUTER_BOUND('',#8943,.T.);
#7300=FACE_OUTER_BOUND('',#8944,.T.);
#7301=FACE_OUTER_BOUND('',#8945,.T.);
#7302=FACE_OUTER_BOUND('',#8946,.T.);
#7303=FACE_OUTER_BOUND('',#8947,.T.);
#7304=FACE_OUTER_BOUND('',#8948,.T.);
#7305=FACE_OUTER_BOUND('',#8949,.T.);
#7306=FACE_OUTER_BOUND('',#8950,.T.);
#7307=FACE_OUTER_BOUND('',#8951,.T.);
#7308=FACE_OUTER_BOUND('',#8952,.T.);
#7309=FACE_OUTER_BOUND('',#8953,.T.);
#7310=FACE_OUTER_BOUND('',#8954,.T.);
#7311=FACE_OUTER_BOUND('',#8955,.T.);
#7312=FACE_OUTER_BOUND('',#8956,.T.);
#7313=FACE_OUTER_BOUND('',#8957,.T.);
#7314=FACE_OUTER_BOUND('',#8958,.T.);
#7315=FACE_OUTER_BOUND('',#8959,.T.);
#7316=FACE_OUTER_BOUND('',#8960,.T.);
#7317=FACE_OUTER_BOUND('',#8961,.T.);
#7318=FACE_OUTER_BOUND('',#8962,.T.);
#7319=FACE_OUTER_BOUND('',#8963,.T.);
#7320=FACE_OUTER_BOUND('',#8964,.T.);
#7321=FACE_OUTER_BOUND('',#8965,.T.);
#7322=FACE_OUTER_BOUND('',#8966,.T.);
#7323=FACE_OUTER_BOUND('',#8967,.T.);
#7324=FACE_OUTER_BOUND('',#8969,.T.);
#7325=FACE_OUTER_BOUND('',#8970,.T.);
#7326=FACE_OUTER_BOUND('',#8972,.T.);
#7327=FACE_OUTER_BOUND('',#8973,.T.);
#7328=FACE_OUTER_BOUND('',#8974,.T.);
#7329=FACE_OUTER_BOUND('',#8975,.T.);
#7330=FACE_OUTER_BOUND('',#8976,.T.);
#7331=FACE_OUTER_BOUND('',#8977,.T.);
#7332=FACE_OUTER_BOUND('',#8978,.T.);
#7333=FACE_OUTER_BOUND('',#8979,.T.);
#7334=FACE_OUTER_BOUND('',#8980,.T.);
#7335=FACE_OUTER_BOUND('',#8981,.T.);
#7336=FACE_OUTER_BOUND('',#8982,.T.);
#7337=FACE_OUTER_BOUND('',#8983,.T.);
#7338=FACE_OUTER_BOUND('',#8984,.T.);
#7339=FACE_OUTER_BOUND('',#8985,.T.);
#7340=FACE_OUTER_BOUND('',#8986,.T.);
#7341=FACE_OUTER_BOUND('',#8987,.T.);
#7342=FACE_OUTER_BOUND('',#8988,.T.);
#7343=FACE_OUTER_BOUND('',#8989,.T.);
#7344=FACE_OUTER_BOUND('',#8990,.T.);
#7345=FACE_OUTER_BOUND('',#8991,.T.);
#7346=FACE_OUTER_BOUND('',#8992,.T.);
#7347=FACE_OUTER_BOUND('',#8993,.T.);
#7348=FACE_OUTER_BOUND('',#8994,.T.);
#7349=FACE_OUTER_BOUND('',#8995,.T.);
#7350=FACE_OUTER_BOUND('',#8996,.T.);
#7351=FACE_OUTER_BOUND('',#8997,.T.);
#7352=FACE_OUTER_BOUND('',#8998,.T.);
#7353=FACE_OUTER_BOUND('',#8999,.T.);
#7354=FACE_OUTER_BOUND('',#9000,.T.);
#7355=FACE_OUTER_BOUND('',#9001,.T.);
#7356=FACE_OUTER_BOUND('',#9002,.T.);
#7357=FACE_OUTER_BOUND('',#9003,.T.);
#7358=FACE_OUTER_BOUND('',#9004,.T.);
#7359=FACE_OUTER_BOUND('',#9005,.T.);
#7360=FACE_OUTER_BOUND('',#9006,.T.);
#7361=FACE_OUTER_BOUND('',#9007,.T.);
#7362=FACE_OUTER_BOUND('',#9008,.T.);
#7363=FACE_OUTER_BOUND('',#9009,.T.);
#7364=FACE_OUTER_BOUND('',#9010,.T.);
#7365=FACE_OUTER_BOUND('',#9011,.T.);
#7366=FACE_OUTER_BOUND('',#9012,.T.);
#7367=FACE_OUTER_BOUND('',#9013,.T.);
#7368=FACE_OUTER_BOUND('',#9014,.T.);
#7369=FACE_OUTER_BOUND('',#9015,.T.);
#7370=FACE_OUTER_BOUND('',#9016,.T.);
#7371=FACE_OUTER_BOUND('',#9017,.T.);
#7372=FACE_OUTER_BOUND('',#9018,.T.);
#7373=FACE_OUTER_BOUND('',#9019,.T.);
#7374=FACE_OUTER_BOUND('',#9020,.T.);
#7375=FACE_OUTER_BOUND('',#9021,.T.);
#7376=FACE_OUTER_BOUND('',#9023,.T.);
#7377=FACE_OUTER_BOUND('',#9024,.T.);
#7378=FACE_OUTER_BOUND('',#9025,.T.);
#7379=FACE_OUTER_BOUND('',#9026,.T.);
#7380=FACE_OUTER_BOUND('',#9027,.T.);
#7381=FACE_OUTER_BOUND('',#9028,.T.);
#7382=FACE_OUTER_BOUND('',#9029,.T.);
#7383=FACE_OUTER_BOUND('',#9030,.T.);
#7384=FACE_OUTER_BOUND('',#9031,.T.);
#7385=FACE_OUTER_BOUND('',#9032,.T.);
#7386=FACE_OUTER_BOUND('',#9033,.T.);
#7387=FACE_OUTER_BOUND('',#9034,.T.);
#7388=FACE_OUTER_BOUND('',#9035,.T.);
#7389=FACE_OUTER_BOUND('',#9036,.T.);
#7390=FACE_OUTER_BOUND('',#9037,.T.);
#7391=FACE_OUTER_BOUND('',#9038,.T.);
#7392=FACE_OUTER_BOUND('',#9039,.T.);
#7393=FACE_OUTER_BOUND('',#9040,.T.);
#7394=FACE_OUTER_BOUND('',#9041,.T.);
#7395=FACE_OUTER_BOUND('',#9042,.T.);
#7396=FACE_OUTER_BOUND('',#9043,.T.);
#7397=FACE_OUTER_BOUND('',#9044,.T.);
#7398=FACE_OUTER_BOUND('',#9045,.T.);
#7399=FACE_OUTER_BOUND('',#9046,.T.);
#7400=FACE_OUTER_BOUND('',#9047,.T.);
#7401=FACE_OUTER_BOUND('',#9048,.T.);
#7402=FACE_OUTER_BOUND('',#9049,.T.);
#7403=FACE_OUTER_BOUND('',#9050,.T.);
#7404=FACE_OUTER_BOUND('',#9051,.T.);
#7405=FACE_OUTER_BOUND('',#9052,.T.);
#7406=FACE_OUTER_BOUND('',#9053,.T.);
#7407=FACE_OUTER_BOUND('',#9054,.T.);
#7408=FACE_OUTER_BOUND('',#9055,.T.);
#7409=FACE_OUTER_BOUND('',#9056,.T.);
#7410=FACE_OUTER_BOUND('',#9057,.T.);
#7411=FACE_OUTER_BOUND('',#9058,.T.);
#7412=FACE_OUTER_BOUND('',#9059,.T.);
#7413=FACE_OUTER_BOUND('',#9060,.T.);
#7414=FACE_OUTER_BOUND('',#9061,.T.);
#7415=FACE_OUTER_BOUND('',#9062,.T.);
#7416=FACE_OUTER_BOUND('',#9063,.T.);
#7417=FACE_OUTER_BOUND('',#9064,.T.);
#7418=FACE_OUTER_BOUND('',#9065,.T.);
#7419=FACE_OUTER_BOUND('',#9066,.T.);
#7420=FACE_OUTER_BOUND('',#9067,.T.);
#7421=FACE_OUTER_BOUND('',#9068,.T.);
#7422=FACE_OUTER_BOUND('',#9069,.T.);
#7423=FACE_OUTER_BOUND('',#9070,.T.);
#7424=FACE_OUTER_BOUND('',#9071,.T.);
#7425=FACE_OUTER_BOUND('',#9072,.T.);
#7426=FACE_OUTER_BOUND('',#9073,.T.);
#7427=FACE_OUTER_BOUND('',#9074,.T.);
#7428=FACE_OUTER_BOUND('',#9075,.T.);
#7429=FACE_OUTER_BOUND('',#9076,.T.);
#7430=FACE_OUTER_BOUND('',#9077,.T.);
#7431=FACE_OUTER_BOUND('',#9078,.T.);
#7432=FACE_OUTER_BOUND('',#9079,.T.);
#7433=FACE_OUTER_BOUND('',#9080,.T.);
#7434=FACE_OUTER_BOUND('',#9081,.T.);
#7435=FACE_OUTER_BOUND('',#9082,.T.);
#7436=FACE_OUTER_BOUND('',#9083,.T.);
#7437=FACE_OUTER_BOUND('',#9084,.T.);
#7438=FACE_OUTER_BOUND('',#9085,.T.);
#7439=FACE_OUTER_BOUND('',#9086,.T.);
#7440=FACE_OUTER_BOUND('',#9087,.T.);
#7441=FACE_OUTER_BOUND('',#9088,.T.);
#7442=FACE_OUTER_BOUND('',#9089,.T.);
#7443=FACE_OUTER_BOUND('',#9090,.T.);
#7444=FACE_OUTER_BOUND('',#9091,.T.);
#7445=FACE_OUTER_BOUND('',#9092,.T.);
#7446=FACE_OUTER_BOUND('',#9093,.T.);
#7447=FACE_OUTER_BOUND('',#9094,.T.);
#7448=FACE_OUTER_BOUND('',#9095,.T.);
#7449=FACE_OUTER_BOUND('',#9096,.T.);
#7450=FACE_OUTER_BOUND('',#9097,.T.);
#7451=FACE_OUTER_BOUND('',#9098,.T.);
#7452=FACE_OUTER_BOUND('',#9099,.T.);
#7453=FACE_OUTER_BOUND('',#9100,.T.);
#7454=FACE_OUTER_BOUND('',#9101,.T.);
#7455=FACE_OUTER_BOUND('',#9102,.T.);
#7456=FACE_OUTER_BOUND('',#9103,.T.);
#7457=FACE_OUTER_BOUND('',#9104,.T.);
#7458=FACE_OUTER_BOUND('',#9105,.T.);
#7459=FACE_OUTER_BOUND('',#9106,.T.);
#7460=FACE_OUTER_BOUND('',#9107,.T.);
#7461=FACE_OUTER_BOUND('',#9108,.T.);
#7462=FACE_OUTER_BOUND('',#9109,.T.);
#7463=FACE_OUTER_BOUND('',#9110,.T.);
#7464=FACE_OUTER_BOUND('',#9111,.T.);
#7465=FACE_OUTER_BOUND('',#9112,.T.);
#7466=FACE_OUTER_BOUND('',#9113,.T.);
#7467=FACE_OUTER_BOUND('',#9114,.T.);
#7468=FACE_OUTER_BOUND('',#9115,.T.);
#7469=FACE_OUTER_BOUND('',#9116,.T.);
#7470=FACE_OUTER_BOUND('',#9117,.T.);
#7471=FACE_OUTER_BOUND('',#9118,.T.);
#7472=FACE_OUTER_BOUND('',#9119,.T.);
#7473=FACE_OUTER_BOUND('',#9120,.T.);
#7474=FACE_OUTER_BOUND('',#9121,.T.);
#7475=FACE_OUTER_BOUND('',#9122,.T.);
#7476=FACE_OUTER_BOUND('',#9123,.T.);
#7477=FACE_OUTER_BOUND('',#9124,.T.);
#7478=FACE_OUTER_BOUND('',#9125,.T.);
#7479=FACE_OUTER_BOUND('',#9126,.T.);
#7480=FACE_OUTER_BOUND('',#9127,.T.);
#7481=FACE_OUTER_BOUND('',#9128,.T.);
#7482=FACE_OUTER_BOUND('',#9129,.T.);
#7483=FACE_OUTER_BOUND('',#9130,.T.);
#7484=FACE_OUTER_BOUND('',#9131,.T.);
#7485=FACE_OUTER_BOUND('',#9132,.T.);
#7486=FACE_OUTER_BOUND('',#9133,.T.);
#7487=FACE_OUTER_BOUND('',#9134,.T.);
#7488=FACE_OUTER_BOUND('',#9135,.T.);
#7489=FACE_OUTER_BOUND('',#9136,.T.);
#7490=FACE_OUTER_BOUND('',#9137,.T.);
#7491=FACE_OUTER_BOUND('',#9138,.T.);
#7492=FACE_OUTER_BOUND('',#9139,.T.);
#7493=FACE_OUTER_BOUND('',#9140,.T.);
#7494=FACE_OUTER_BOUND('',#9141,.T.);
#7495=FACE_OUTER_BOUND('',#9142,.T.);
#7496=FACE_OUTER_BOUND('',#9143,.T.);
#7497=FACE_OUTER_BOUND('',#9144,.T.);
#7498=FACE_OUTER_BOUND('',#9145,.T.);
#7499=FACE_OUTER_BOUND('',#9146,.T.);
#7500=FACE_OUTER_BOUND('',#9147,.T.);
#7501=FACE_OUTER_BOUND('',#9148,.T.);
#7502=FACE_OUTER_BOUND('',#9149,.T.);
#7503=FACE_OUTER_BOUND('',#9150,.T.);
#7504=FACE_OUTER_BOUND('',#9151,.T.);
#7505=FACE_OUTER_BOUND('',#9152,.T.);
#7506=FACE_OUTER_BOUND('',#9153,.T.);
#7507=FACE_OUTER_BOUND('',#9154,.T.);
#7508=FACE_OUTER_BOUND('',#9155,.T.);
#7509=FACE_OUTER_BOUND('',#9156,.T.);
#7510=FACE_OUTER_BOUND('',#9157,.T.);
#7511=FACE_OUTER_BOUND('',#9158,.T.);
#7512=FACE_OUTER_BOUND('',#9159,.T.);
#7513=FACE_OUTER_BOUND('',#9160,.T.);
#7514=FACE_OUTER_BOUND('',#9162,.T.);
#7515=FACE_OUTER_BOUND('',#9163,.T.);
#7516=FACE_OUTER_BOUND('',#9164,.T.);
#7517=FACE_OUTER_BOUND('',#9165,.T.);
#7518=FACE_OUTER_BOUND('',#9166,.T.);
#7519=FACE_OUTER_BOUND('',#9167,.T.);
#7520=FACE_OUTER_BOUND('',#9168,.T.);
#7521=FACE_OUTER_BOUND('',#9169,.T.);
#7522=FACE_OUTER_BOUND('',#9170,.T.);
#7523=FACE_OUTER_BOUND('',#9171,.T.);
#7524=FACE_OUTER_BOUND('',#9172,.T.);
#7525=FACE_OUTER_BOUND('',#9173,.T.);
#7526=FACE_OUTER_BOUND('',#9174,.T.);
#7527=FACE_OUTER_BOUND('',#9175,.T.);
#7528=FACE_OUTER_BOUND('',#9176,.T.);
#7529=FACE_OUTER_BOUND('',#9177,.T.);
#7530=FACE_OUTER_BOUND('',#9178,.T.);
#7531=FACE_OUTER_BOUND('',#9179,.T.);
#7532=FACE_OUTER_BOUND('',#9180,.T.);
#7533=FACE_OUTER_BOUND('',#9181,.T.);
#7534=FACE_OUTER_BOUND('',#9182,.T.);
#7535=FACE_OUTER_BOUND('',#9183,.T.);
#7536=FACE_OUTER_BOUND('',#9184,.T.);
#7537=FACE_OUTER_BOUND('',#9185,.T.);
#7538=FACE_OUTER_BOUND('',#9186,.T.);
#7539=FACE_OUTER_BOUND('',#9187,.T.);
#7540=FACE_OUTER_BOUND('',#9188,.T.);
#7541=FACE_OUTER_BOUND('',#9189,.T.);
#7542=FACE_OUTER_BOUND('',#9190,.T.);
#7543=FACE_OUTER_BOUND('',#9191,.T.);
#7544=FACE_OUTER_BOUND('',#9192,.T.);
#7545=FACE_OUTER_BOUND('',#9193,.T.);
#7546=FACE_OUTER_BOUND('',#9194,.T.);
#7547=FACE_OUTER_BOUND('',#9195,.T.);
#7548=FACE_OUTER_BOUND('',#9196,.T.);
#7549=FACE_OUTER_BOUND('',#9197,.T.);
#7550=FACE_OUTER_BOUND('',#9198,.T.);
#7551=FACE_OUTER_BOUND('',#9199,.T.);
#7552=FACE_OUTER_BOUND('',#9200,.T.);
#7553=FACE_OUTER_BOUND('',#9201,.T.);
#7554=FACE_OUTER_BOUND('',#9202,.T.);
#7555=FACE_OUTER_BOUND('',#9203,.T.);
#7556=FACE_OUTER_BOUND('',#9204,.T.);
#7557=FACE_OUTER_BOUND('',#9205,.T.);
#7558=FACE_OUTER_BOUND('',#9206,.T.);
#7559=FACE_OUTER_BOUND('',#9207,.T.);
#7560=FACE_OUTER_BOUND('',#9208,.T.);
#7561=FACE_OUTER_BOUND('',#9209,.T.);
#7562=FACE_OUTER_BOUND('',#9210,.T.);
#7563=FACE_OUTER_BOUND('',#9211,.T.);
#7564=FACE_OUTER_BOUND('',#9212,.T.);
#7565=FACE_OUTER_BOUND('',#9213,.T.);
#7566=FACE_OUTER_BOUND('',#9214,.T.);
#7567=FACE_OUTER_BOUND('',#9215,.T.);
#7568=FACE_OUTER_BOUND('',#9216,.T.);
#7569=FACE_OUTER_BOUND('',#9217,.T.);
#7570=FACE_OUTER_BOUND('',#9218,.T.);
#7571=FACE_OUTER_BOUND('',#9219,.T.);
#7572=FACE_OUTER_BOUND('',#9220,.T.);
#7573=FACE_OUTER_BOUND('',#9221,.T.);
#7574=FACE_OUTER_BOUND('',#9222,.T.);
#7575=FACE_OUTER_BOUND('',#9223,.T.);
#7576=FACE_OUTER_BOUND('',#9224,.T.);
#7577=FACE_OUTER_BOUND('',#9225,.T.);
#7578=FACE_OUTER_BOUND('',#9226,.T.);
#7579=FACE_OUTER_BOUND('',#9227,.T.);
#7580=FACE_OUTER_BOUND('',#9228,.T.);
#7581=FACE_OUTER_BOUND('',#9229,.T.);
#7582=FACE_OUTER_BOUND('',#9230,.T.);
#7583=FACE_OUTER_BOUND('',#9231,.T.);
#7584=FACE_OUTER_BOUND('',#9232,.T.);
#7585=FACE_OUTER_BOUND('',#9233,.T.);
#7586=FACE_OUTER_BOUND('',#9234,.T.);
#7587=FACE_OUTER_BOUND('',#9235,.T.);
#7588=FACE_OUTER_BOUND('',#9236,.T.);
#7589=FACE_OUTER_BOUND('',#9237,.T.);
#7590=FACE_OUTER_BOUND('',#9238,.T.);
#7591=FACE_OUTER_BOUND('',#9239,.T.);
#7592=FACE_OUTER_BOUND('',#9240,.T.);
#7593=FACE_OUTER_BOUND('',#9241,.T.);
#7594=FACE_OUTER_BOUND('',#9242,.T.);
#7595=FACE_OUTER_BOUND('',#9243,.T.);
#7596=FACE_OUTER_BOUND('',#9244,.T.);
#7597=FACE_OUTER_BOUND('',#9245,.T.);
#7598=FACE_OUTER_BOUND('',#9246,.T.);
#7599=FACE_OUTER_BOUND('',#9247,.T.);
#7600=FACE_OUTER_BOUND('',#9248,.T.);
#7601=FACE_OUTER_BOUND('',#9249,.T.);
#7602=FACE_OUTER_BOUND('',#9250,.T.);
#7603=FACE_OUTER_BOUND('',#9251,.T.);
#7604=FACE_OUTER_BOUND('',#9252,.T.);
#7605=FACE_OUTER_BOUND('',#9253,.T.);
#7606=FACE_OUTER_BOUND('',#9254,.T.);
#7607=FACE_OUTER_BOUND('',#9255,.T.);
#7608=FACE_OUTER_BOUND('',#9256,.T.);
#7609=FACE_OUTER_BOUND('',#9257,.T.);
#7610=FACE_OUTER_BOUND('',#9258,.T.);
#7611=FACE_OUTER_BOUND('',#9259,.T.);
#7612=FACE_OUTER_BOUND('',#9260,.T.);
#7613=FACE_OUTER_BOUND('',#9261,.T.);
#7614=FACE_OUTER_BOUND('',#9262,.T.);
#7615=FACE_OUTER_BOUND('',#9263,.T.);
#7616=FACE_OUTER_BOUND('',#9264,.T.);
#7617=FACE_OUTER_BOUND('',#9265,.T.);
#7618=FACE_OUTER_BOUND('',#9266,.T.);
#7619=FACE_OUTER_BOUND('',#9267,.T.);
#7620=FACE_OUTER_BOUND('',#9268,.T.);
#7621=FACE_OUTER_BOUND('',#9269,.T.);
#7622=FACE_OUTER_BOUND('',#9270,.T.);
#7623=FACE_OUTER_BOUND('',#9271,.T.);
#7624=FACE_OUTER_BOUND('',#9272,.T.);
#7625=FACE_OUTER_BOUND('',#9273,.T.);
#7626=FACE_OUTER_BOUND('',#9274,.T.);
#7627=FACE_OUTER_BOUND('',#9275,.T.);
#7628=FACE_OUTER_BOUND('',#9276,.T.);
#7629=FACE_OUTER_BOUND('',#9277,.T.);
#7630=FACE_OUTER_BOUND('',#9278,.T.);
#7631=FACE_OUTER_BOUND('',#9279,.T.);
#7632=FACE_OUTER_BOUND('',#9280,.T.);
#7633=FACE_OUTER_BOUND('',#9281,.T.);
#7634=FACE_OUTER_BOUND('',#9282,.T.);
#7635=FACE_OUTER_BOUND('',#9283,.T.);
#7636=FACE_OUTER_BOUND('',#9284,.T.);
#7637=FACE_OUTER_BOUND('',#9285,.T.);
#7638=FACE_OUTER_BOUND('',#9286,.T.);
#7639=FACE_OUTER_BOUND('',#9287,.T.);
#7640=FACE_OUTER_BOUND('',#9288,.T.);
#7641=FACE_OUTER_BOUND('',#9289,.T.);
#7642=FACE_OUTER_BOUND('',#9290,.T.);
#7643=FACE_OUTER_BOUND('',#9291,.T.);
#7644=FACE_OUTER_BOUND('',#9292,.T.);
#7645=FACE_OUTER_BOUND('',#9293,.T.);
#7646=FACE_OUTER_BOUND('',#9294,.T.);
#7647=FACE_OUTER_BOUND('',#9295,.T.);
#7648=FACE_OUTER_BOUND('',#9296,.T.);
#7649=FACE_OUTER_BOUND('',#9297,.T.);
#7650=FACE_OUTER_BOUND('',#9298,.T.);
#7651=FACE_OUTER_BOUND('',#9299,.T.);
#7652=FACE_OUTER_BOUND('',#9300,.T.);
#7653=FACE_OUTER_BOUND('',#9301,.T.);
#7654=FACE_OUTER_BOUND('',#9302,.T.);
#7655=FACE_OUTER_BOUND('',#9303,.T.);
#7656=FACE_OUTER_BOUND('',#9304,.T.);
#7657=FACE_OUTER_BOUND('',#9305,.T.);
#7658=FACE_OUTER_BOUND('',#9306,.T.);
#7659=FACE_OUTER_BOUND('',#9307,.T.);
#7660=FACE_OUTER_BOUND('',#9308,.T.);
#7661=FACE_OUTER_BOUND('',#9309,.T.);
#7662=FACE_OUTER_BOUND('',#9310,.T.);
#7663=FACE_OUTER_BOUND('',#9311,.T.);
#7664=FACE_OUTER_BOUND('',#9312,.T.);
#7665=FACE_OUTER_BOUND('',#9313,.T.);
#7666=FACE_OUTER_BOUND('',#9314,.T.);
#7667=FACE_OUTER_BOUND('',#9315,.T.);
#7668=FACE_OUTER_BOUND('',#9316,.T.);
#7669=FACE_OUTER_BOUND('',#9317,.T.);
#7670=FACE_OUTER_BOUND('',#9318,.T.);
#7671=FACE_OUTER_BOUND('',#9319,.T.);
#7672=FACE_OUTER_BOUND('',#9320,.T.);
#7673=FACE_OUTER_BOUND('',#9321,.T.);
#7674=FACE_OUTER_BOUND('',#9322,.T.);
#7675=FACE_OUTER_BOUND('',#9323,.T.);
#7676=FACE_OUTER_BOUND('',#9324,.T.);
#7677=FACE_OUTER_BOUND('',#9325,.T.);
#7678=FACE_OUTER_BOUND('',#9326,.T.);
#7679=FACE_OUTER_BOUND('',#9327,.T.);
#7680=FACE_OUTER_BOUND('',#9328,.T.);
#7681=FACE_OUTER_BOUND('',#9329,.T.);
#7682=FACE_OUTER_BOUND('',#9330,.T.);
#7683=FACE_OUTER_BOUND('',#9331,.T.);
#7684=FACE_OUTER_BOUND('',#9332,.T.);
#7685=FACE_OUTER_BOUND('',#9333,.T.);
#7686=FACE_OUTER_BOUND('',#9334,.T.);
#7687=FACE_OUTER_BOUND('',#9335,.T.);
#7688=FACE_OUTER_BOUND('',#9336,.T.);
#7689=FACE_OUTER_BOUND('',#9337,.T.);
#7690=FACE_OUTER_BOUND('',#9338,.T.);
#7691=FACE_OUTER_BOUND('',#9339,.T.);
#7692=FACE_OUTER_BOUND('',#9340,.T.);
#7693=FACE_OUTER_BOUND('',#9341,.T.);
#7694=FACE_OUTER_BOUND('',#9342,.T.);
#7695=FACE_OUTER_BOUND('',#9343,.T.);
#7696=FACE_OUTER_BOUND('',#9344,.T.);
#7697=FACE_OUTER_BOUND('',#9345,.T.);
#7698=FACE_OUTER_BOUND('',#9346,.T.);
#7699=FACE_OUTER_BOUND('',#9347,.T.);
#7700=FACE_OUTER_BOUND('',#9348,.T.);
#7701=FACE_OUTER_BOUND('',#9349,.T.);
#7702=FACE_OUTER_BOUND('',#9350,.T.);
#7703=FACE_OUTER_BOUND('',#9351,.T.);
#7704=FACE_OUTER_BOUND('',#9352,.T.);
#7705=FACE_OUTER_BOUND('',#9353,.T.);
#7706=FACE_OUTER_BOUND('',#9354,.T.);
#7707=FACE_OUTER_BOUND('',#9355,.T.);
#7708=FACE_OUTER_BOUND('',#9356,.T.);
#7709=FACE_OUTER_BOUND('',#9357,.T.);
#7710=FACE_OUTER_BOUND('',#9358,.T.);
#7711=FACE_OUTER_BOUND('',#9359,.T.);
#7712=FACE_OUTER_BOUND('',#9360,.T.);
#7713=FACE_OUTER_BOUND('',#9361,.T.);
#7714=FACE_OUTER_BOUND('',#9362,.T.);
#7715=FACE_OUTER_BOUND('',#9363,.T.);
#7716=FACE_OUTER_BOUND('',#9364,.T.);
#7717=FACE_OUTER_BOUND('',#9365,.T.);
#7718=FACE_OUTER_BOUND('',#9366,.T.);
#7719=FACE_OUTER_BOUND('',#9367,.T.);
#7720=FACE_OUTER_BOUND('',#9368,.T.);
#7721=FACE_OUTER_BOUND('',#9369,.T.);
#7722=FACE_OUTER_BOUND('',#9370,.T.);
#7723=FACE_OUTER_BOUND('',#9371,.T.);
#7724=FACE_OUTER_BOUND('',#9372,.T.);
#7725=FACE_OUTER_BOUND('',#9373,.T.);
#7726=FACE_OUTER_BOUND('',#9374,.T.);
#7727=FACE_OUTER_BOUND('',#9375,.T.);
#7728=FACE_OUTER_BOUND('',#9376,.T.);
#7729=FACE_OUTER_BOUND('',#9377,.T.);
#7730=FACE_OUTER_BOUND('',#9378,.T.);
#7731=FACE_OUTER_BOUND('',#9379,.T.);
#7732=FACE_OUTER_BOUND('',#9380,.T.);
#7733=FACE_OUTER_BOUND('',#9381,.T.);
#7734=FACE_OUTER_BOUND('',#9382,.T.);
#7735=FACE_OUTER_BOUND('',#9383,.T.);
#7736=FACE_OUTER_BOUND('',#9384,.T.);
#7737=FACE_OUTER_BOUND('',#9385,.T.);
#7738=FACE_OUTER_BOUND('',#9386,.T.);
#7739=FACE_OUTER_BOUND('',#9387,.T.);
#7740=FACE_OUTER_BOUND('',#9388,.T.);
#7741=FACE_OUTER_BOUND('',#9389,.T.);
#7742=FACE_OUTER_BOUND('',#9390,.T.);
#7743=FACE_OUTER_BOUND('',#9391,.T.);
#7744=FACE_OUTER_BOUND('',#9392,.T.);
#7745=FACE_OUTER_BOUND('',#9393,.T.);
#7746=FACE_OUTER_BOUND('',#9394,.T.);
#7747=FACE_OUTER_BOUND('',#9395,.T.);
#7748=FACE_OUTER_BOUND('',#9396,.T.);
#7749=FACE_OUTER_BOUND('',#9397,.T.);
#7750=FACE_OUTER_BOUND('',#9398,.T.);
#7751=FACE_OUTER_BOUND('',#9399,.T.);
#7752=FACE_OUTER_BOUND('',#9400,.T.);
#7753=FACE_OUTER_BOUND('',#9401,.T.);
#7754=FACE_OUTER_BOUND('',#9402,.T.);
#7755=FACE_OUTER_BOUND('',#9403,.T.);
#7756=FACE_OUTER_BOUND('',#9404,.T.);
#7757=FACE_OUTER_BOUND('',#9405,.T.);
#7758=FACE_OUTER_BOUND('',#9406,.T.);
#7759=FACE_OUTER_BOUND('',#9407,.T.);
#7760=FACE_OUTER_BOUND('',#9408,.T.);
#7761=FACE_OUTER_BOUND('',#9409,.T.);
#7762=FACE_OUTER_BOUND('',#9410,.T.);
#7763=FACE_OUTER_BOUND('',#9411,.T.);
#7764=FACE_OUTER_BOUND('',#9412,.T.);
#7765=FACE_OUTER_BOUND('',#9413,.T.);
#7766=FACE_OUTER_BOUND('',#9414,.T.);
#7767=FACE_OUTER_BOUND('',#9415,.T.);
#7768=FACE_OUTER_BOUND('',#9416,.T.);
#7769=FACE_OUTER_BOUND('',#9417,.T.);
#7770=FACE_OUTER_BOUND('',#9418,.T.);
#7771=FACE_OUTER_BOUND('',#9419,.T.);
#7772=FACE_OUTER_BOUND('',#9420,.T.);
#7773=FACE_OUTER_BOUND('',#9421,.T.);
#7774=FACE_OUTER_BOUND('',#9422,.T.);
#7775=FACE_OUTER_BOUND('',#9423,.T.);
#7776=FACE_OUTER_BOUND('',#9424,.T.);
#7777=FACE_OUTER_BOUND('',#9425,.T.);
#7778=FACE_OUTER_BOUND('',#9426,.T.);
#7779=FACE_OUTER_BOUND('',#9427,.T.);
#7780=FACE_OUTER_BOUND('',#9428,.T.);
#7781=FACE_OUTER_BOUND('',#9429,.T.);
#7782=FACE_OUTER_BOUND('',#9430,.T.);
#7783=FACE_OUTER_BOUND('',#9431,.T.);
#7784=FACE_OUTER_BOUND('',#9432,.T.);
#7785=FACE_OUTER_BOUND('',#9433,.T.);
#7786=FACE_OUTER_BOUND('',#9434,.T.);
#7787=FACE_OUTER_BOUND('',#9435,.T.);
#7788=FACE_OUTER_BOUND('',#9436,.T.);
#7789=FACE_OUTER_BOUND('',#9437,.T.);
#7790=FACE_OUTER_BOUND('',#9438,.T.);
#7791=FACE_OUTER_BOUND('',#9439,.T.);
#7792=FACE_OUTER_BOUND('',#9440,.T.);
#7793=FACE_OUTER_BOUND('',#9441,.T.);
#7794=FACE_OUTER_BOUND('',#9442,.T.);
#7795=FACE_OUTER_BOUND('',#9443,.T.);
#7796=FACE_OUTER_BOUND('',#9444,.T.);
#7797=FACE_OUTER_BOUND('',#9445,.T.);
#7798=FACE_OUTER_BOUND('',#9446,.T.);
#7799=FACE_OUTER_BOUND('',#9447,.T.);
#7800=FACE_OUTER_BOUND('',#9448,.T.);
#7801=FACE_OUTER_BOUND('',#9450,.T.);
#7802=FACE_OUTER_BOUND('',#9451,.T.);
#7803=FACE_OUTER_BOUND('',#9452,.T.);
#7804=FACE_OUTER_BOUND('',#9454,.T.);
#7805=FACE_OUTER_BOUND('',#9455,.T.);
#7806=FACE_OUTER_BOUND('',#9457,.T.);
#7807=FACE_OUTER_BOUND('',#9458,.T.);
#7808=FACE_OUTER_BOUND('',#9460,.T.);
#7809=FACE_OUTER_BOUND('',#9461,.T.);
#7810=FACE_OUTER_BOUND('',#9463,.T.);
#7811=FACE_OUTER_BOUND('',#9464,.T.);
#7812=FACE_OUTER_BOUND('',#9466,.T.);
#7813=FACE_OUTER_BOUND('',#9468,.T.);
#7814=FACE_OUTER_BOUND('',#9469,.T.);
#7815=FACE_OUTER_BOUND('',#9470,.T.);
#7816=FACE_OUTER_BOUND('',#9471,.T.);
#7817=FACE_OUTER_BOUND('',#9473,.T.);
#7818=FACE_OUTER_BOUND('',#9474,.T.);
#7819=FACE_OUTER_BOUND('',#9476,.T.);
#7820=FACE_OUTER_BOUND('',#9477,.T.);
#7821=FACE_OUTER_BOUND('',#9478,.T.);
#7822=FACE_OUTER_BOUND('',#9479,.T.);
#7823=FACE_OUTER_BOUND('',#9481,.T.);
#7824=FACE_OUTER_BOUND('',#9482,.T.);
#7825=FACE_OUTER_BOUND('',#9484,.T.);
#7826=FACE_OUTER_BOUND('',#9485,.T.);
#7827=FACE_OUTER_BOUND('',#9487,.T.);
#7828=FACE_OUTER_BOUND('',#9488,.T.);
#7829=FACE_OUTER_BOUND('',#9489,.T.);
#7830=FACE_OUTER_BOUND('',#9490,.T.);
#7831=FACE_OUTER_BOUND('',#9492,.T.);
#7832=FACE_OUTER_BOUND('',#9493,.T.);
#7833=FACE_OUTER_BOUND('',#9494,.T.);
#7834=FACE_OUTER_BOUND('',#9496,.T.);
#7835=FACE_OUTER_BOUND('',#9497,.T.);
#7836=FACE_OUTER_BOUND('',#9499,.T.);
#7837=FACE_OUTER_BOUND('',#9500,.T.);
#7838=FACE_OUTER_BOUND('',#9501,.T.);
#7839=FACE_OUTER_BOUND('',#9503,.T.);
#7840=FACE_OUTER_BOUND('',#9504,.T.);
#7841=FACE_OUTER_BOUND('',#9506,.T.);
#7842=FACE_OUTER_BOUND('',#9507,.T.);
#7843=FACE_OUTER_BOUND('',#9509,.T.);
#7844=FACE_OUTER_BOUND('',#9510,.T.);
#7845=FACE_OUTER_BOUND('',#9511,.T.);
#7846=FACE_OUTER_BOUND('',#9513,.T.);
#7847=FACE_OUTER_BOUND('',#9514,.T.);
#7848=FACE_OUTER_BOUND('',#9515,.T.);
#7849=FACE_OUTER_BOUND('',#9516,.T.);
#7850=FACE_OUTER_BOUND('',#9517,.T.);
#7851=FACE_OUTER_BOUND('',#9518,.T.);
#7852=FACE_OUTER_BOUND('',#9519,.T.);
#7853=FACE_OUTER_BOUND('',#9521,.T.);
#7854=FACE_OUTER_BOUND('',#9522,.T.);
#7855=FACE_OUTER_BOUND('',#9524,.T.);
#7856=FACE_OUTER_BOUND('',#9525,.T.);
#7857=FACE_OUTER_BOUND('',#9526,.T.);
#7858=FACE_OUTER_BOUND('',#9527,.T.);
#7859=FACE_OUTER_BOUND('',#9528,.T.);
#7860=FACE_OUTER_BOUND('',#9529,.T.);
#7861=FACE_OUTER_BOUND('',#9530,.T.);
#7862=FACE_OUTER_BOUND('',#9531,.T.);
#7863=FACE_OUTER_BOUND('',#9532,.T.);
#7864=FACE_OUTER_BOUND('',#9533,.T.);
#7865=FACE_OUTER_BOUND('',#9534,.T.);
#7866=FACE_OUTER_BOUND('',#9535,.T.);
#7867=FACE_OUTER_BOUND('',#9536,.T.);
#7868=FACE_OUTER_BOUND('',#9537,.T.);
#7869=FACE_OUTER_BOUND('',#9538,.T.);
#7870=FACE_OUTER_BOUND('',#9539,.T.);
#7871=FACE_OUTER_BOUND('',#9540,.T.);
#7872=FACE_OUTER_BOUND('',#9541,.T.);
#7873=FACE_OUTER_BOUND('',#9542,.T.);
#7874=FACE_OUTER_BOUND('',#9543,.T.);
#7875=FACE_OUTER_BOUND('',#9544,.T.);
#7876=FACE_OUTER_BOUND('',#9545,.T.);
#7877=FACE_OUTER_BOUND('',#9546,.T.);
#7878=FACE_OUTER_BOUND('',#9547,.T.);
#7879=FACE_OUTER_BOUND('',#9548,.T.);
#7880=FACE_OUTER_BOUND('',#9549,.T.);
#7881=FACE_OUTER_BOUND('',#9550,.T.);
#7882=FACE_OUTER_BOUND('',#9551,.T.);
#7883=FACE_OUTER_BOUND('',#9552,.T.);
#7884=FACE_OUTER_BOUND('',#9553,.T.);
#7885=FACE_OUTER_BOUND('',#9554,.T.);
#7886=FACE_OUTER_BOUND('',#9555,.T.);
#7887=FACE_OUTER_BOUND('',#9556,.T.);
#7888=FACE_OUTER_BOUND('',#9557,.T.);
#7889=FACE_OUTER_BOUND('',#9558,.T.);
#7890=FACE_OUTER_BOUND('',#9559,.T.);
#7891=FACE_OUTER_BOUND('',#9560,.T.);
#7892=FACE_OUTER_BOUND('',#9561,.T.);
#7893=FACE_OUTER_BOUND('',#9562,.T.);
#7894=FACE_OUTER_BOUND('',#9563,.T.);
#7895=FACE_OUTER_BOUND('',#9564,.T.);
#7896=FACE_OUTER_BOUND('',#9565,.T.);
#7897=FACE_OUTER_BOUND('',#9566,.T.);
#7898=FACE_OUTER_BOUND('',#9567,.T.);
#7899=FACE_OUTER_BOUND('',#9568,.T.);
#7900=FACE_OUTER_BOUND('',#9569,.T.);
#7901=FACE_OUTER_BOUND('',#9570,.T.);
#7902=FACE_OUTER_BOUND('',#9571,.T.);
#7903=FACE_OUTER_BOUND('',#9572,.T.);
#7904=FACE_OUTER_BOUND('',#9573,.T.);
#7905=FACE_OUTER_BOUND('',#9574,.T.);
#7906=FACE_OUTER_BOUND('',#9575,.T.);
#7907=FACE_OUTER_BOUND('',#9576,.T.);
#7908=FACE_OUTER_BOUND('',#9577,.T.);
#7909=FACE_OUTER_BOUND('',#9578,.T.);
#7910=FACE_OUTER_BOUND('',#9579,.T.);
#7911=FACE_OUTER_BOUND('',#9580,.T.);
#7912=FACE_OUTER_BOUND('',#9581,.T.);
#7913=FACE_OUTER_BOUND('',#9582,.T.);
#7914=FACE_OUTER_BOUND('',#9583,.T.);
#7915=FACE_OUTER_BOUND('',#9584,.T.);
#7916=FACE_OUTER_BOUND('',#9585,.T.);
#7917=FACE_OUTER_BOUND('',#9586,.T.);
#7918=FACE_OUTER_BOUND('',#9587,.T.);
#7919=FACE_OUTER_BOUND('',#9588,.T.);
#7920=FACE_OUTER_BOUND('',#9589,.T.);
#7921=FACE_OUTER_BOUND('',#9590,.T.);
#7922=FACE_OUTER_BOUND('',#9591,.T.);
#7923=FACE_OUTER_BOUND('',#9592,.T.);
#7924=FACE_OUTER_BOUND('',#9593,.T.);
#7925=FACE_OUTER_BOUND('',#9594,.T.);
#7926=FACE_OUTER_BOUND('',#9595,.T.);
#7927=FACE_OUTER_BOUND('',#9596,.T.);
#7928=FACE_OUTER_BOUND('',#9597,.T.);
#7929=FACE_OUTER_BOUND('',#9598,.T.);
#7930=FACE_OUTER_BOUND('',#9599,.T.);
#7931=FACE_OUTER_BOUND('',#9600,.T.);
#7932=FACE_OUTER_BOUND('',#9601,.T.);
#7933=FACE_OUTER_BOUND('',#9602,.T.);
#7934=FACE_OUTER_BOUND('',#9603,.T.);
#7935=FACE_OUTER_BOUND('',#9604,.T.);
#7936=FACE_OUTER_BOUND('',#9605,.T.);
#7937=FACE_OUTER_BOUND('',#9606,.T.);
#7938=FACE_OUTER_BOUND('',#9607,.T.);
#7939=FACE_OUTER_BOUND('',#9608,.T.);
#7940=FACE_OUTER_BOUND('',#9609,.T.);
#7941=FACE_OUTER_BOUND('',#9615,.T.);
#7942=FACE_OUTER_BOUND('',#9616,.T.);
#7943=FACE_OUTER_BOUND('',#9617,.T.);
#7944=FACE_OUTER_BOUND('',#9618,.T.);
#7945=FACE_OUTER_BOUND('',#9619,.T.);
#7946=FACE_OUTER_BOUND('',#9620,.T.);
#7947=FACE_OUTER_BOUND('',#9621,.T.);
#7948=FACE_OUTER_BOUND('',#9622,.T.);
#7949=FACE_OUTER_BOUND('',#9623,.T.);
#7950=FACE_OUTER_BOUND('',#9624,.T.);
#7951=FACE_OUTER_BOUND('',#9625,.T.);
#7952=FACE_OUTER_BOUND('',#9626,.T.);
#7953=FACE_OUTER_BOUND('',#9631,.T.);
#7954=FACE_OUTER_BOUND('',#9632,.T.);
#7955=FACE_OUTER_BOUND('',#9633,.T.);
#7956=FACE_OUTER_BOUND('',#9634,.T.);
#7957=FACE_OUTER_BOUND('',#9635,.T.);
#7958=FACE_OUTER_BOUND('',#9636,.T.);
#7959=FACE_OUTER_BOUND('',#9637,.T.);
#7960=FACE_OUTER_BOUND('',#9638,.T.);
#7961=FACE_OUTER_BOUND('',#9639,.T.);
#7962=FACE_OUTER_BOUND('',#9640,.T.);
#7963=FACE_OUTER_BOUND('',#9641,.T.);
#7964=FACE_OUTER_BOUND('',#9642,.T.);
#7965=FACE_OUTER_BOUND('',#9643,.T.);
#7966=FACE_OUTER_BOUND('',#9644,.T.);
#7967=FACE_OUTER_BOUND('',#9645,.T.);
#7968=FACE_OUTER_BOUND('',#9646,.T.);
#7969=FACE_OUTER_BOUND('',#9647,.T.);
#7970=FACE_OUTER_BOUND('',#9648,.T.);
#7971=FACE_OUTER_BOUND('',#9649,.T.);
#7972=FACE_OUTER_BOUND('',#9650,.T.);
#7973=FACE_OUTER_BOUND('',#9651,.T.);
#7974=FACE_OUTER_BOUND('',#9652,.T.);
#7975=FACE_OUTER_BOUND('',#9653,.T.);
#7976=FACE_OUTER_BOUND('',#9654,.T.);
#7977=FACE_OUTER_BOUND('',#9655,.T.);
#7978=FACE_OUTER_BOUND('',#9656,.T.);
#7979=FACE_OUTER_BOUND('',#9657,.T.);
#7980=FACE_OUTER_BOUND('',#9659,.T.);
#7981=FACE_OUTER_BOUND('',#9660,.T.);
#7982=FACE_OUTER_BOUND('',#9661,.T.);
#7983=FACE_OUTER_BOUND('',#9662,.T.);
#7984=FACE_OUTER_BOUND('',#9663,.T.);
#7985=FACE_OUTER_BOUND('',#9664,.T.);
#7986=FACE_OUTER_BOUND('',#9665,.T.);
#7987=FACE_OUTER_BOUND('',#9666,.T.);
#7988=FACE_OUTER_BOUND('',#9667,.T.);
#7989=FACE_OUTER_BOUND('',#9668,.T.);
#7990=FACE_OUTER_BOUND('',#9669,.T.);
#7991=FACE_OUTER_BOUND('',#9670,.T.);
#7992=FACE_OUTER_BOUND('',#9671,.T.);
#7993=FACE_OUTER_BOUND('',#9672,.T.);
#7994=FACE_OUTER_BOUND('',#9673,.T.);
#7995=FACE_OUTER_BOUND('',#9674,.T.);
#7996=FACE_OUTER_BOUND('',#9675,.T.);
#7997=FACE_OUTER_BOUND('',#9676,.T.);
#7998=FACE_OUTER_BOUND('',#9677,.T.);
#7999=FACE_OUTER_BOUND('',#9678,.T.);
#8000=FACE_OUTER_BOUND('',#9679,.T.);
#8001=FACE_OUTER_BOUND('',#9680,.T.);
#8002=FACE_OUTER_BOUND('',#9681,.T.);
#8003=FACE_OUTER_BOUND('',#9682,.T.);
#8004=FACE_OUTER_BOUND('',#9683,.T.);
#8005=FACE_OUTER_BOUND('',#9685,.T.);
#8006=FACE_OUTER_BOUND('',#9686,.T.);
#8007=FACE_OUTER_BOUND('',#9687,.T.);
#8008=FACE_OUTER_BOUND('',#9688,.T.);
#8009=FACE_OUTER_BOUND('',#9689,.T.);
#8010=FACE_OUTER_BOUND('',#9690,.T.);
#8011=FACE_OUTER_BOUND('',#9691,.T.);
#8012=FACE_OUTER_BOUND('',#9692,.T.);
#8013=FACE_OUTER_BOUND('',#9693,.T.);
#8014=FACE_OUTER_BOUND('',#9694,.T.);
#8015=FACE_OUTER_BOUND('',#9695,.T.);
#8016=FACE_OUTER_BOUND('',#9696,.T.);
#8017=FACE_OUTER_BOUND('',#9697,.T.);
#8018=FACE_OUTER_BOUND('',#9698,.T.);
#8019=FACE_OUTER_BOUND('',#9699,.T.);
#8020=FACE_OUTER_BOUND('',#9700,.T.);
#8021=FACE_OUTER_BOUND('',#9701,.T.);
#8022=FACE_OUTER_BOUND('',#9702,.T.);
#8023=FACE_OUTER_BOUND('',#9703,.T.);
#8024=FACE_OUTER_BOUND('',#9704,.T.);
#8025=FACE_OUTER_BOUND('',#9705,.T.);
#8026=FACE_OUTER_BOUND('',#9706,.T.);
#8027=FACE_OUTER_BOUND('',#9707,.T.);
#8028=FACE_OUTER_BOUND('',#9708,.T.);
#8029=FACE_OUTER_BOUND('',#9709,.T.);
#8030=FACE_OUTER_BOUND('',#9710,.T.);
#8031=FACE_OUTER_BOUND('',#9711,.T.);
#8032=FACE_OUTER_BOUND('',#9712,.T.);
#8033=FACE_OUTER_BOUND('',#9713,.T.);
#8034=FACE_OUTER_BOUND('',#9714,.T.);
#8035=FACE_OUTER_BOUND('',#9715,.T.);
#8036=FACE_OUTER_BOUND('',#9716,.T.);
#8037=FACE_OUTER_BOUND('',#9717,.T.);
#8038=FACE_OUTER_BOUND('',#9718,.T.);
#8039=FACE_OUTER_BOUND('',#9719,.T.);
#8040=FACE_OUTER_BOUND('',#9720,.T.);
#8041=FACE_OUTER_BOUND('',#9721,.T.);
#8042=FACE_OUTER_BOUND('',#9722,.T.);
#8043=FACE_OUTER_BOUND('',#9723,.T.);
#8044=FACE_OUTER_BOUND('',#9724,.T.);
#8045=FACE_OUTER_BOUND('',#9725,.T.);
#8046=FACE_OUTER_BOUND('',#9726,.T.);
#8047=FACE_OUTER_BOUND('',#9727,.T.);
#8048=FACE_OUTER_BOUND('',#9728,.T.);
#8049=FACE_OUTER_BOUND('',#9729,.T.);
#8050=FACE_OUTER_BOUND('',#9730,.T.);
#8051=FACE_OUTER_BOUND('',#9731,.T.);
#8052=FACE_OUTER_BOUND('',#9732,.T.);
#8053=FACE_OUTER_BOUND('',#9733,.T.);
#8054=FACE_OUTER_BOUND('',#9734,.T.);
#8055=FACE_OUTER_BOUND('',#9735,.T.);
#8056=FACE_OUTER_BOUND('',#9737,.T.);
#8057=FACE_OUTER_BOUND('',#9738,.T.);
#8058=FACE_OUTER_BOUND('',#9739,.T.);
#8059=FACE_OUTER_BOUND('',#9740,.T.);
#8060=FACE_OUTER_BOUND('',#9741,.T.);
#8061=FACE_OUTER_BOUND('',#9742,.T.);
#8062=FACE_OUTER_BOUND('',#9743,.T.);
#8063=FACE_OUTER_BOUND('',#9744,.T.);
#8064=FACE_OUTER_BOUND('',#9745,.T.);
#8065=FACE_OUTER_BOUND('',#9746,.T.);
#8066=FACE_OUTER_BOUND('',#9747,.T.);
#8067=FACE_OUTER_BOUND('',#9748,.T.);
#8068=FACE_OUTER_BOUND('',#9749,.T.);
#8069=FACE_OUTER_BOUND('',#9750,.T.);
#8070=FACE_OUTER_BOUND('',#9751,.T.);
#8071=FACE_OUTER_BOUND('',#9752,.T.);
#8072=FACE_OUTER_BOUND('',#9753,.T.);
#8073=FACE_OUTER_BOUND('',#9754,.T.);
#8074=FACE_OUTER_BOUND('',#9755,.T.);
#8075=FACE_OUTER_BOUND('',#9756,.T.);
#8076=FACE_OUTER_BOUND('',#9757,.T.);
#8077=FACE_OUTER_BOUND('',#9758,.T.);
#8078=FACE_OUTER_BOUND('',#9759,.T.);
#8079=FACE_OUTER_BOUND('',#9760,.T.);
#8080=FACE_OUTER_BOUND('',#9761,.T.);
#8081=FACE_OUTER_BOUND('',#9762,.T.);
#8082=FACE_OUTER_BOUND('',#9763,.T.);
#8083=FACE_OUTER_BOUND('',#9764,.T.);
#8084=FACE_OUTER_BOUND('',#9765,.T.);
#8085=FACE_OUTER_BOUND('',#9766,.T.);
#8086=FACE_OUTER_BOUND('',#9767,.T.);
#8087=FACE_OUTER_BOUND('',#9768,.T.);
#8088=FACE_OUTER_BOUND('',#9769,.T.);
#8089=FACE_OUTER_BOUND('',#9770,.T.);
#8090=FACE_OUTER_BOUND('',#9771,.T.);
#8091=FACE_OUTER_BOUND('',#9772,.T.);
#8092=FACE_OUTER_BOUND('',#9773,.T.);
#8093=FACE_OUTER_BOUND('',#9774,.T.);
#8094=FACE_OUTER_BOUND('',#9775,.T.);
#8095=FACE_OUTER_BOUND('',#9776,.T.);
#8096=FACE_OUTER_BOUND('',#9777,.T.);
#8097=FACE_OUTER_BOUND('',#9778,.T.);
#8098=FACE_OUTER_BOUND('',#9779,.T.);
#8099=FACE_OUTER_BOUND('',#9780,.T.);
#8100=FACE_OUTER_BOUND('',#9781,.T.);
#8101=FACE_OUTER_BOUND('',#9782,.T.);
#8102=FACE_OUTER_BOUND('',#9783,.T.);
#8103=FACE_OUTER_BOUND('',#9784,.T.);
#8104=FACE_OUTER_BOUND('',#9785,.T.);
#8105=FACE_OUTER_BOUND('',#9787,.T.);
#8106=FACE_OUTER_BOUND('',#9788,.T.);
#8107=FACE_OUTER_BOUND('',#9789,.T.);
#8108=FACE_OUTER_BOUND('',#9790,.T.);
#8109=FACE_OUTER_BOUND('',#9791,.T.);
#8110=FACE_OUTER_BOUND('',#9792,.T.);
#8111=FACE_OUTER_BOUND('',#9793,.T.);
#8112=FACE_OUTER_BOUND('',#9794,.T.);
#8113=FACE_OUTER_BOUND('',#9795,.T.);
#8114=FACE_OUTER_BOUND('',#9796,.T.);
#8115=FACE_OUTER_BOUND('',#9797,.T.);
#8116=FACE_OUTER_BOUND('',#9798,.T.);
#8117=FACE_OUTER_BOUND('',#9799,.T.);
#8118=FACE_OUTER_BOUND('',#9800,.T.);
#8119=FACE_OUTER_BOUND('',#9801,.T.);
#8120=FACE_OUTER_BOUND('',#9802,.T.);
#8121=FACE_OUTER_BOUND('',#9803,.T.);
#8122=FACE_OUTER_BOUND('',#9804,.T.);
#8123=FACE_OUTER_BOUND('',#9805,.T.);
#8124=FACE_OUTER_BOUND('',#9806,.T.);
#8125=FACE_OUTER_BOUND('',#9807,.T.);
#8126=FACE_OUTER_BOUND('',#9808,.T.);
#8127=FACE_OUTER_BOUND('',#9809,.T.);
#8128=FACE_OUTER_BOUND('',#9810,.T.);
#8129=FACE_OUTER_BOUND('',#9811,.T.);
#8130=FACE_OUTER_BOUND('',#9812,.T.);
#8131=FACE_OUTER_BOUND('',#9813,.T.);
#8132=FACE_OUTER_BOUND('',#9814,.T.);
#8133=FACE_OUTER_BOUND('',#9815,.T.);
#8134=FACE_OUTER_BOUND('',#9816,.T.);
#8135=FACE_OUTER_BOUND('',#9817,.T.);
#8136=FACE_OUTER_BOUND('',#9818,.T.);
#8137=FACE_OUTER_BOUND('',#9819,.T.);
#8138=FACE_OUTER_BOUND('',#9820,.T.);
#8139=FACE_OUTER_BOUND('',#9821,.T.);
#8140=FACE_OUTER_BOUND('',#9822,.T.);
#8141=FACE_OUTER_BOUND('',#9823,.T.);
#8142=FACE_OUTER_BOUND('',#9824,.T.);
#8143=FACE_OUTER_BOUND('',#9825,.T.);
#8144=FACE_OUTER_BOUND('',#9826,.T.);
#8145=FACE_OUTER_BOUND('',#9827,.T.);
#8146=FACE_OUTER_BOUND('',#9828,.T.);
#8147=FACE_OUTER_BOUND('',#9829,.T.);
#8148=FACE_OUTER_BOUND('',#9830,.T.);
#8149=FACE_OUTER_BOUND('',#9831,.T.);
#8150=FACE_OUTER_BOUND('',#9832,.T.);
#8151=FACE_OUTER_BOUND('',#9833,.T.);
#8152=FACE_OUTER_BOUND('',#9834,.T.);
#8153=FACE_OUTER_BOUND('',#9835,.T.);
#8154=FACE_OUTER_BOUND('',#9836,.T.);
#8155=FACE_OUTER_BOUND('',#9837,.T.);
#8156=FACE_OUTER_BOUND('',#9838,.T.);
#8157=FACE_OUTER_BOUND('',#9839,.T.);
#8158=FACE_OUTER_BOUND('',#9840,.T.);
#8159=FACE_OUTER_BOUND('',#9841,.T.);
#8160=FACE_OUTER_BOUND('',#9842,.T.);
#8161=FACE_OUTER_BOUND('',#9843,.T.);
#8162=FACE_OUTER_BOUND('',#9844,.T.);
#8163=FACE_OUTER_BOUND('',#9845,.T.);
#8164=FACE_OUTER_BOUND('',#9846,.T.);
#8165=FACE_OUTER_BOUND('',#9847,.T.);
#8166=FACE_OUTER_BOUND('',#9848,.T.);
#8167=FACE_OUTER_BOUND('',#9849,.T.);
#8168=FACE_OUTER_BOUND('',#9850,.T.);
#8169=FACE_OUTER_BOUND('',#9851,.T.);
#8170=FACE_OUTER_BOUND('',#9852,.T.);
#8171=FACE_OUTER_BOUND('',#9853,.T.);
#8172=FACE_OUTER_BOUND('',#9854,.T.);
#8173=FACE_OUTER_BOUND('',#9855,.T.);
#8174=FACE_OUTER_BOUND('',#9856,.T.);
#8175=FACE_OUTER_BOUND('',#9857,.T.);
#8176=FACE_OUTER_BOUND('',#9858,.T.);
#8177=FACE_OUTER_BOUND('',#9859,.T.);
#8178=FACE_OUTER_BOUND('',#9860,.T.);
#8179=FACE_OUTER_BOUND('',#9861,.T.);
#8180=FACE_OUTER_BOUND('',#9862,.T.);
#8181=FACE_OUTER_BOUND('',#9863,.T.);
#8182=FACE_OUTER_BOUND('',#9864,.T.);
#8183=FACE_OUTER_BOUND('',#9865,.T.);
#8184=FACE_OUTER_BOUND('',#9866,.T.);
#8185=FACE_OUTER_BOUND('',#9867,.T.);
#8186=FACE_OUTER_BOUND('',#9868,.T.);
#8187=FACE_OUTER_BOUND('',#9869,.T.);
#8188=FACE_OUTER_BOUND('',#9870,.T.);
#8189=FACE_OUTER_BOUND('',#9871,.T.);
#8190=FACE_OUTER_BOUND('',#9872,.T.);
#8191=FACE_OUTER_BOUND('',#9873,.T.);
#8192=FACE_OUTER_BOUND('',#9874,.T.);
#8193=FACE_OUTER_BOUND('',#9875,.T.);
#8194=FACE_OUTER_BOUND('',#9876,.T.);
#8195=FACE_OUTER_BOUND('',#9877,.T.);
#8196=FACE_OUTER_BOUND('',#9878,.T.);
#8197=FACE_OUTER_BOUND('',#9879,.T.);
#8198=FACE_OUTER_BOUND('',#9880,.T.);
#8199=FACE_OUTER_BOUND('',#9881,.T.);
#8200=FACE_OUTER_BOUND('',#9882,.T.);
#8201=FACE_OUTER_BOUND('',#9883,.T.);
#8202=FACE_OUTER_BOUND('',#9884,.T.);
#8203=FACE_OUTER_BOUND('',#9885,.T.);
#8204=FACE_OUTER_BOUND('',#9886,.T.);
#8205=FACE_OUTER_BOUND('',#9887,.T.);
#8206=FACE_OUTER_BOUND('',#9888,.T.);
#8207=FACE_OUTER_BOUND('',#9889,.T.);
#8208=FACE_OUTER_BOUND('',#9890,.T.);
#8209=FACE_OUTER_BOUND('',#9891,.T.);
#8210=FACE_OUTER_BOUND('',#9892,.T.);
#8211=FACE_OUTER_BOUND('',#9893,.T.);
#8212=FACE_OUTER_BOUND('',#9894,.T.);
#8213=FACE_OUTER_BOUND('',#9895,.T.);
#8214=FACE_OUTER_BOUND('',#9896,.T.);
#8215=FACE_OUTER_BOUND('',#9897,.T.);
#8216=FACE_OUTER_BOUND('',#9898,.T.);
#8217=FACE_OUTER_BOUND('',#9899,.T.);
#8218=FACE_OUTER_BOUND('',#9900,.T.);
#8219=FACE_OUTER_BOUND('',#9901,.T.);
#8220=FACE_OUTER_BOUND('',#9902,.T.);
#8221=FACE_OUTER_BOUND('',#9903,.T.);
#8222=FACE_OUTER_BOUND('',#9904,.T.);
#8223=FACE_OUTER_BOUND('',#9905,.T.);
#8224=FACE_OUTER_BOUND('',#9906,.T.);
#8225=FACE_OUTER_BOUND('',#9907,.T.);
#8226=FACE_OUTER_BOUND('',#9908,.T.);
#8227=FACE_OUTER_BOUND('',#9909,.T.);
#8228=FACE_OUTER_BOUND('',#9910,.T.);
#8229=FACE_OUTER_BOUND('',#9911,.T.);
#8230=FACE_OUTER_BOUND('',#9912,.T.);
#8231=FACE_OUTER_BOUND('',#9913,.T.);
#8232=FACE_OUTER_BOUND('',#9914,.T.);
#8233=FACE_OUTER_BOUND('',#9915,.T.);
#8234=FACE_OUTER_BOUND('',#9916,.T.);
#8235=FACE_OUTER_BOUND('',#9917,.T.);
#8236=FACE_OUTER_BOUND('',#9918,.T.);
#8237=FACE_OUTER_BOUND('',#9919,.T.);
#8238=FACE_OUTER_BOUND('',#9920,.T.);
#8239=FACE_OUTER_BOUND('',#9921,.T.);
#8240=FACE_OUTER_BOUND('',#9922,.T.);
#8241=FACE_OUTER_BOUND('',#9923,.T.);
#8242=FACE_OUTER_BOUND('',#9924,.T.);
#8243=FACE_OUTER_BOUND('',#9925,.T.);
#8244=FACE_OUTER_BOUND('',#9926,.T.);
#8245=FACE_OUTER_BOUND('',#9927,.T.);
#8246=FACE_OUTER_BOUND('',#9928,.T.);
#8247=FACE_OUTER_BOUND('',#9929,.T.);
#8248=FACE_OUTER_BOUND('',#9930,.T.);
#8249=FACE_OUTER_BOUND('',#9931,.T.);
#8250=FACE_OUTER_BOUND('',#9932,.T.);
#8251=FACE_OUTER_BOUND('',#9933,.T.);
#8252=FACE_OUTER_BOUND('',#9934,.T.);
#8253=FACE_OUTER_BOUND('',#9935,.T.);
#8254=FACE_OUTER_BOUND('',#9936,.T.);
#8255=FACE_OUTER_BOUND('',#9937,.T.);
#8256=FACE_OUTER_BOUND('',#9938,.T.);
#8257=FACE_OUTER_BOUND('',#9939,.T.);
#8258=FACE_OUTER_BOUND('',#9940,.T.);
#8259=FACE_OUTER_BOUND('',#9941,.T.);
#8260=FACE_OUTER_BOUND('',#9942,.T.);
#8261=FACE_OUTER_BOUND('',#9943,.T.);
#8262=FACE_OUTER_BOUND('',#9944,.T.);
#8263=FACE_OUTER_BOUND('',#9945,.T.);
#8264=FACE_OUTER_BOUND('',#9946,.T.);
#8265=FACE_OUTER_BOUND('',#9947,.T.);
#8266=FACE_OUTER_BOUND('',#9948,.T.);
#8267=FACE_OUTER_BOUND('',#9949,.T.);
#8268=FACE_OUTER_BOUND('',#9950,.T.);
#8269=FACE_OUTER_BOUND('',#9951,.T.);
#8270=FACE_OUTER_BOUND('',#9952,.T.);
#8271=FACE_OUTER_BOUND('',#9953,.T.);
#8272=FACE_OUTER_BOUND('',#9954,.T.);
#8273=FACE_OUTER_BOUND('',#9955,.T.);
#8274=FACE_OUTER_BOUND('',#9956,.T.);
#8275=FACE_OUTER_BOUND('',#9957,.T.);
#8276=FACE_OUTER_BOUND('',#9958,.T.);
#8277=FACE_OUTER_BOUND('',#9959,.T.);
#8278=FACE_OUTER_BOUND('',#9960,.T.);
#8279=FACE_OUTER_BOUND('',#9961,.T.);
#8280=FACE_OUTER_BOUND('',#9962,.T.);
#8281=FACE_OUTER_BOUND('',#9963,.T.);
#8282=FACE_OUTER_BOUND('',#9964,.T.);
#8283=FACE_OUTER_BOUND('',#9965,.T.);
#8284=FACE_OUTER_BOUND('',#9966,.T.);
#8285=FACE_OUTER_BOUND('',#9967,.T.);
#8286=FACE_OUTER_BOUND('',#9968,.T.);
#8287=FACE_OUTER_BOUND('',#9969,.T.);
#8288=FACE_OUTER_BOUND('',#9970,.T.);
#8289=FACE_OUTER_BOUND('',#9971,.T.);
#8290=FACE_OUTER_BOUND('',#9972,.T.);
#8291=FACE_OUTER_BOUND('',#9973,.T.);
#8292=FACE_OUTER_BOUND('',#9974,.T.);
#8293=FACE_OUTER_BOUND('',#9975,.T.);
#8294=FACE_OUTER_BOUND('',#9976,.T.);
#8295=FACE_OUTER_BOUND('',#9977,.T.);
#8296=FACE_OUTER_BOUND('',#9978,.T.);
#8297=FACE_OUTER_BOUND('',#9979,.T.);
#8298=FACE_OUTER_BOUND('',#9980,.T.);
#8299=FACE_OUTER_BOUND('',#9981,.T.);
#8300=FACE_OUTER_BOUND('',#9982,.T.);
#8301=FACE_OUTER_BOUND('',#9983,.T.);
#8302=FACE_OUTER_BOUND('',#9984,.T.);
#8303=FACE_OUTER_BOUND('',#9985,.T.);
#8304=FACE_OUTER_BOUND('',#9986,.T.);
#8305=FACE_OUTER_BOUND('',#9987,.T.);
#8306=FACE_OUTER_BOUND('',#9988,.T.);
#8307=FACE_OUTER_BOUND('',#9989,.T.);
#8308=FACE_OUTER_BOUND('',#9990,.T.);
#8309=FACE_OUTER_BOUND('',#9991,.T.);
#8310=FACE_OUTER_BOUND('',#9992,.T.);
#8311=FACE_OUTER_BOUND('',#9994,.T.);
#8312=FACE_OUTER_BOUND('',#10030,.T.);
#8313=FACE_OUTER_BOUND('',#10031,.T.);
#8314=FACE_OUTER_BOUND('',#10033,.T.);
#8315=FACE_OUTER_BOUND('',#10034,.T.);
#8316=FACE_OUTER_BOUND('',#10035,.T.);
#8317=FACE_OUTER_BOUND('',#10036,.T.);
#8318=FACE_OUTER_BOUND('',#10037,.T.);
#8319=FACE_OUTER_BOUND('',#10038,.T.);
#8320=FACE_OUTER_BOUND('',#10039,.T.);
#8321=FACE_OUTER_BOUND('',#10040,.T.);
#8322=FACE_OUTER_BOUND('',#10041,.T.);
#8323=FACE_OUTER_BOUND('',#10042,.T.);
#8324=FACE_OUTER_BOUND('',#10043,.T.);
#8325=FACE_OUTER_BOUND('',#10044,.T.);
#8326=FACE_OUTER_BOUND('',#10045,.T.);
#8327=FACE_OUTER_BOUND('',#10046,.T.);
#8328=FACE_OUTER_BOUND('',#10047,.T.);
#8329=FACE_OUTER_BOUND('',#10048,.T.);
#8330=FACE_OUTER_BOUND('',#10049,.T.);
#8331=FACE_OUTER_BOUND('',#10050,.T.);
#8332=FACE_OUTER_BOUND('',#10051,.T.);
#8333=FACE_OUTER_BOUND('',#10052,.T.);
#8334=FACE_OUTER_BOUND('',#10053,.T.);
#8335=FACE_OUTER_BOUND('',#10054,.T.);
#8336=FACE_OUTER_BOUND('',#10056,.T.);
#8337=FACE_OUTER_BOUND('',#10057,.T.);
#8338=FACE_OUTER_BOUND('',#10058,.T.);
#8339=FACE_OUTER_BOUND('',#10059,.T.);
#8340=FACE_OUTER_BOUND('',#10060,.T.);
#8341=FACE_OUTER_BOUND('',#10061,.T.);
#8342=FACE_OUTER_BOUND('',#10062,.T.);
#8343=FACE_OUTER_BOUND('',#10063,.T.);
#8344=FACE_OUTER_BOUND('',#10064,.T.);
#8345=FACE_OUTER_BOUND('',#10065,.T.);
#8346=FACE_OUTER_BOUND('',#10066,.T.);
#8347=FACE_OUTER_BOUND('',#10067,.T.);
#8348=FACE_OUTER_BOUND('',#10068,.T.);
#8349=FACE_OUTER_BOUND('',#10069,.T.);
#8350=FACE_OUTER_BOUND('',#10071,.T.);
#8351=FACE_OUTER_BOUND('',#10072,.T.);
#8352=FACE_OUTER_BOUND('',#10073,.T.);
#8353=FACE_OUTER_BOUND('',#10074,.T.);
#8354=FACE_OUTER_BOUND('',#10075,.T.);
#8355=FACE_OUTER_BOUND('',#10076,.T.);
#8356=FACE_OUTER_BOUND('',#10077,.T.);
#8357=FACE_OUTER_BOUND('',#10078,.T.);
#8358=FACE_OUTER_BOUND('',#10079,.T.);
#8359=FACE_OUTER_BOUND('',#10080,.T.);
#8360=FACE_OUTER_BOUND('',#10081,.T.);
#8361=FACE_OUTER_BOUND('',#10082,.T.);
#8362=FACE_OUTER_BOUND('',#10083,.T.);
#8363=FACE_OUTER_BOUND('',#10084,.T.);
#8364=FACE_OUTER_BOUND('',#10085,.T.);
#8365=FACE_OUTER_BOUND('',#10086,.T.);
#8366=FACE_OUTER_BOUND('',#10087,.T.);
#8367=FACE_OUTER_BOUND('',#10088,.T.);
#8368=FACE_OUTER_BOUND('',#10089,.T.);
#8369=FACE_OUTER_BOUND('',#10090,.T.);
#8370=FACE_OUTER_BOUND('',#10091,.T.);
#8371=FACE_OUTER_BOUND('',#10092,.T.);
#8372=FACE_OUTER_BOUND('',#10093,.T.);
#8373=FACE_OUTER_BOUND('',#10094,.T.);
#8374=FACE_OUTER_BOUND('',#10095,.T.);
#8375=FACE_OUTER_BOUND('',#10096,.T.);
#8376=FACE_OUTER_BOUND('',#10097,.T.);
#8377=FACE_OUTER_BOUND('',#10098,.T.);
#8378=FACE_OUTER_BOUND('',#10099,.T.);
#8379=FACE_OUTER_BOUND('',#10100,.T.);
#8380=FACE_OUTER_BOUND('',#10101,.T.);
#8381=FACE_OUTER_BOUND('',#10102,.T.);
#8382=FACE_OUTER_BOUND('',#10103,.T.);
#8383=FACE_OUTER_BOUND('',#10104,.T.);
#8384=FACE_OUTER_BOUND('',#10105,.T.);
#8385=FACE_OUTER_BOUND('',#10106,.T.);
#8386=FACE_OUTER_BOUND('',#10107,.T.);
#8387=FACE_OUTER_BOUND('',#10108,.T.);
#8388=FACE_OUTER_BOUND('',#10109,.T.);
#8389=FACE_OUTER_BOUND('',#10110,.T.);
#8390=FACE_OUTER_BOUND('',#10111,.T.);
#8391=FACE_OUTER_BOUND('',#10112,.T.);
#8392=FACE_OUTER_BOUND('',#10113,.T.);
#8393=FACE_OUTER_BOUND('',#10114,.T.);
#8394=FACE_OUTER_BOUND('',#10115,.T.);
#8395=FACE_OUTER_BOUND('',#10116,.T.);
#8396=FACE_OUTER_BOUND('',#10118,.T.);
#8397=EDGE_LOOP('',(#17802,#17803,#17804,#17805,#17806,#17807,#17808,#17809));
#8398=EDGE_LOOP('',(#17810,#17811,#17812,#17813,#17814,#17815,#17816,#17817,
#17818,#17819,#17820,#17821,#17822,#17823,#17824,#17825));
#8399=EDGE_LOOP('',(#17826));
#8400=EDGE_LOOP('',(#17827));
#8401=EDGE_LOOP('',(#17828));
#8402=EDGE_LOOP('',(#17829));
#8403=EDGE_LOOP('',(#17830));
#8404=EDGE_LOOP('',(#17831));
#8405=EDGE_LOOP('',(#17832,#17833,#17834,#17835,#17836,#17837,#17838,#17839));
#8406=EDGE_LOOP('',(#17840));
#8407=EDGE_LOOP('',(#17841));
#8408=EDGE_LOOP('',(#17842));
#8409=EDGE_LOOP('',(#17843));
#8410=EDGE_LOOP('',(#17844));
#8411=EDGE_LOOP('',(#17845));
#8412=EDGE_LOOP('',(#17846));
#8413=EDGE_LOOP('',(#17847));
#8414=EDGE_LOOP('',(#17848));
#8415=EDGE_LOOP('',(#17849));
#8416=EDGE_LOOP('',(#17850,#17851,#17852,#17853));
#8417=EDGE_LOOP('',(#17854,#17855,#17856,#17857));
#8418=EDGE_LOOP('',(#17858,#17859,#17860,#17861));
#8419=EDGE_LOOP('',(#17862,#17863,#17864,#17865));
#8420=EDGE_LOOP('',(#17866,#17867,#17868,#17869));
#8421=EDGE_LOOP('',(#17870,#17871,#17872,#17873));
#8422=EDGE_LOOP('',(#17874,#17875,#17876,#17877));
#8423=EDGE_LOOP('',(#17878,#17879,#17880,#17881));
#8424=EDGE_LOOP('',(#17882,#17883,#17884,#17885));
#8425=EDGE_LOOP('',(#17886,#17887,#17888,#17889));
#8426=EDGE_LOOP('',(#17890,#17891,#17892,#17893));
#8427=EDGE_LOOP('',(#17894,#17895,#17896,#17897));
#8428=EDGE_LOOP('',(#17898,#17899,#17900,#17901,#17902,#17903,#17904,#17905));
#8429=EDGE_LOOP('',(#17906));
#8430=EDGE_LOOP('',(#17907));
#8431=EDGE_LOOP('',(#17908,#17909,#17910,#17911));
#8432=EDGE_LOOP('',(#17912,#17913,#17914,#17915));
#8433=EDGE_LOOP('',(#17916,#17917,#17918,#17919));
#8434=EDGE_LOOP('',(#17920,#17921,#17922,#17923));
#8435=EDGE_LOOP('',(#17924,#17925,#17926,#17927));
#8436=EDGE_LOOP('',(#17928,#17929,#17930,#17931));
#8437=EDGE_LOOP('',(#17932,#17933,#17934,#17935));
#8438=EDGE_LOOP('',(#17936,#17937,#17938,#17939));
#8439=EDGE_LOOP('',(#17940,#17941,#17942,#17943));
#8440=EDGE_LOOP('',(#17944,#17945,#17946,#17947));
#8441=EDGE_LOOP('',(#17948,#17949,#17950,#17951));
#8442=EDGE_LOOP('',(#17952,#17953,#17954,#17955,#17956,#17957,#17958,#17959));
#8443=EDGE_LOOP('',(#17960,#17961,#17962,#17963,#17964,#17965,#17966,#17967));
#8444=EDGE_LOOP('',(#17968));
#8445=EDGE_LOOP('',(#17969));
#8446=EDGE_LOOP('',(#17970,#17971,#17972,#17973));
#8447=EDGE_LOOP('',(#17974,#17975,#17976,#17977));
#8448=EDGE_LOOP('',(#17978,#17979,#17980,#17981));
#8449=EDGE_LOOP('',(#17982,#17983,#17984,#17985));
#8450=EDGE_LOOP('',(#17986,#17987,#17988,#17989));
#8451=EDGE_LOOP('',(#17990,#17991,#17992,#17993));
#8452=EDGE_LOOP('',(#17994,#17995,#17996,#17997));
#8453=EDGE_LOOP('',(#17998,#17999,#18000,#18001));
#8454=EDGE_LOOP('',(#18002,#18003,#18004,#18005));
#8455=EDGE_LOOP('',(#18006,#18007,#18008,#18009));
#8456=EDGE_LOOP('',(#18010,#18011,#18012,#18013));
#8457=EDGE_LOOP('',(#18014,#18015,#18016,#18017));
#8458=EDGE_LOOP('',(#18018,#18019,#18020,#18021,#18022,#18023,#18024,#18025));
#8459=EDGE_LOOP('',(#18026));
#8460=EDGE_LOOP('',(#18027,#18028,#18029,#18030));
#8461=EDGE_LOOP('',(#18031,#18032,#18033,#18034));
#8462=EDGE_LOOP('',(#18035,#18036,#18037,#18038));
#8463=EDGE_LOOP('',(#18039,#18040,#18041,#18042));
#8464=EDGE_LOOP('',(#18043,#18044,#18045,#18046));
#8465=EDGE_LOOP('',(#18047,#18048,#18049,#18050));
#8466=EDGE_LOOP('',(#18051,#18052,#18053,#18054));
#8467=EDGE_LOOP('',(#18055,#18056,#18057,#18058));
#8468=EDGE_LOOP('',(#18059,#18060,#18061,#18062));
#8469=EDGE_LOOP('',(#18063,#18064,#18065,#18066));
#8470=EDGE_LOOP('',(#18067,#18068,#18069,#18070));
#8471=EDGE_LOOP('',(#18071,#18072,#18073,#18074));
#8472=EDGE_LOOP('',(#18075,#18076,#18077,#18078,#18079,#18080,#18081,#18082));
#8473=EDGE_LOOP('',(#18083));
#8474=EDGE_LOOP('',(#18084,#18085,#18086,#18087));
#8475=EDGE_LOOP('',(#18088,#18089,#18090,#18091,#18092,#18093,#18094,#18095,
#18096,#18097));
#8476=EDGE_LOOP('',(#18098,#18099,#18100,#18101));
#8477=EDGE_LOOP('',(#18102,#18103,#18104,#18105));
#8478=EDGE_LOOP('',(#18106));
#8479=EDGE_LOOP('',(#18107,#18108,#18109,#18110));
#8480=EDGE_LOOP('',(#18111,#18112,#18113,#18114));
#8481=EDGE_LOOP('',(#18115,#18116,#18117,#18118));
#8482=EDGE_LOOP('',(#18119,#18120,#18121,#18122));
#8483=EDGE_LOOP('',(#18123,#18124,#18125,#18126));
#8484=EDGE_LOOP('',(#18127,#18128,#18129,#18130));
#8485=EDGE_LOOP('',(#18131,#18132,#18133,#18134));
#8486=EDGE_LOOP('',(#18135,#18136,#18137,#18138,#18139));
#8487=EDGE_LOOP('',(#18140,#18141,#18142,#18143));
#8488=EDGE_LOOP('',(#18144,#18145,#18146,#18147));
#8489=EDGE_LOOP('',(#18148,#18149,#18150,#18151));
#8490=EDGE_LOOP('',(#18152,#18153,#18154,#18155,#18156,#18157));
#8491=EDGE_LOOP('',(#18158,#18159,#18160,#18161));
#8492=EDGE_LOOP('',(#18162,#18163,#18164,#18165,#18166,#18167,#18168,#18169));
#8493=EDGE_LOOP('',(#18170,#18171,#18172,#18173,#18174));
#8494=EDGE_LOOP('',(#18175,#18176,#18177,#18178));
#8495=EDGE_LOOP('',(#18179,#18180,#18181,#18182));
#8496=EDGE_LOOP('',(#18183,#18184,#18185,#18186));
#8497=EDGE_LOOP('',(#18187,#18188,#18189,#18190));
#8498=EDGE_LOOP('',(#18191,#18192,#18193,#18194,#18195,#18196));
#8499=EDGE_LOOP('',(#18197,#18198,#18199,#18200,#18201,#18202));
#8500=EDGE_LOOP('',(#18203,#18204,#18205,#18206,#18207,#18208));
#8501=EDGE_LOOP('',(#18209,#18210,#18211,#18212));
#8502=EDGE_LOOP('',(#18213,#18214,#18215,#18216));
#8503=EDGE_LOOP('',(#18217,#18218,#18219,#18220));
#8504=EDGE_LOOP('',(#18221,#18222,#18223,#18224));
#8505=EDGE_LOOP('',(#18225,#18226,#18227,#18228));
#8506=EDGE_LOOP('',(#18229,#18230,#18231,#18232));
#8507=EDGE_LOOP('',(#18233,#18234,#18235,#18236));
#8508=EDGE_LOOP('',(#18237,#18238,#18239,#18240));
#8509=EDGE_LOOP('',(#18241,#18242,#18243,#18244));
#8510=EDGE_LOOP('',(#18245,#18246,#18247,#18248,#18249,#18250,#18251,#18252));
#8511=EDGE_LOOP('',(#18253,#18254,#18255,#18256,#18257,#18258,#18259,#18260));
#8512=EDGE_LOOP('',(#18261,#18262,#18263,#18264,#18265,#18266,#18267,#18268));
#8513=EDGE_LOOP('',(#18269));
#8514=EDGE_LOOP('',(#18270,#18271,#18272,#18273,#18274));
#8515=EDGE_LOOP('',(#18275,#18276,#18277,#18278));
#8516=EDGE_LOOP('',(#18279,#18280,#18281,#18282));
#8517=EDGE_LOOP('',(#18283,#18284,#18285,#18286));
#8518=EDGE_LOOP('',(#18287,#18288,#18289,#18290,#18291,#18292));
#8519=EDGE_LOOP('',(#18293,#18294,#18295,#18296,#18297,#18298,#18299,#18300));
#8520=EDGE_LOOP('',(#18301,#18302,#18303,#18304));
#8521=EDGE_LOOP('',(#18305,#18306,#18307,#18308));
#8522=EDGE_LOOP('',(#18309,#18310,#18311,#18312));
#8523=EDGE_LOOP('',(#18313));
#8524=EDGE_LOOP('',(#18314,#18315,#18316,#18317));
#8525=EDGE_LOOP('',(#18318));
#8526=EDGE_LOOP('',(#18319,#18320,#18321,#18322));
#8527=EDGE_LOOP('',(#18323));
#8528=EDGE_LOOP('',(#18324));
#8529=EDGE_LOOP('',(#18325,#18326,#18327,#18328));
#8530=EDGE_LOOP('',(#18329));
#8531=EDGE_LOOP('',(#18330,#18331,#18332,#18333));
#8532=EDGE_LOOP('',(#18334,#18335,#18336,#18337));
#8533=EDGE_LOOP('',(#18338));
#8534=EDGE_LOOP('',(#18339,#18340,#18341,#18342));
#8535=EDGE_LOOP('',(#18343));
#8536=EDGE_LOOP('',(#18344,#18345,#18346,#18347));
#8537=EDGE_LOOP('',(#18348));
#8538=EDGE_LOOP('',(#18349,#18350,#18351,#18352));
#8539=EDGE_LOOP('',(#18353));
#8540=EDGE_LOOP('',(#18354,#18355,#18356,#18357));
#8541=EDGE_LOOP('',(#18358));
#8542=EDGE_LOOP('',(#18359,#18360,#18361,#18362));
#8543=EDGE_LOOP('',(#18363));
#8544=EDGE_LOOP('',(#18364,#18365,#18366,#18367));
#8545=EDGE_LOOP('',(#18368));
#8546=EDGE_LOOP('',(#18369,#18370,#18371,#18372));
#8547=EDGE_LOOP('',(#18373));
#8548=EDGE_LOOP('',(#18374,#18375,#18376,#18377));
#8549=EDGE_LOOP('',(#18378));
#8550=EDGE_LOOP('',(#18379,#18380,#18381,#18382));
#8551=EDGE_LOOP('',(#18383));
#8552=EDGE_LOOP('',(#18384,#18385,#18386,#18387));
#8553=EDGE_LOOP('',(#18388));
#8554=EDGE_LOOP('',(#18389,#18390,#18391,#18392));
#8555=EDGE_LOOP('',(#18393));
#8556=EDGE_LOOP('',(#18394,#18395,#18396,#18397,#18398));
#8557=EDGE_LOOP('',(#18399));
#8558=EDGE_LOOP('',(#18400));
#8559=EDGE_LOOP('',(#18401,#18402,#18403,#18404));
#8560=EDGE_LOOP('',(#18405,#18406,#18407,#18408));
#8561=EDGE_LOOP('',(#18409,#18410,#18411,#18412));
#8562=EDGE_LOOP('',(#18413,#18414,#18415,#18416));
#8563=EDGE_LOOP('',(#18417,#18418,#18419,#18420));
#8564=EDGE_LOOP('',(#18421,#18422,#18423,#18424));
#8565=EDGE_LOOP('',(#18425,#18426,#18427,#18428));
#8566=EDGE_LOOP('',(#18429,#18430,#18431,#18432));
#8567=EDGE_LOOP('',(#18433,#18434,#18435,#18436));
#8568=EDGE_LOOP('',(#18437,#18438,#18439,#18440));
#8569=EDGE_LOOP('',(#18441,#18442,#18443,#18444));
#8570=EDGE_LOOP('',(#18445,#18446,#18447,#18448));
#8571=EDGE_LOOP('',(#18449,#18450,#18451,#18452));
#8572=EDGE_LOOP('',(#18453,#18454,#18455,#18456));
#8573=EDGE_LOOP('',(#18457,#18458,#18459,#18460));
#8574=EDGE_LOOP('',(#18461,#18462,#18463,#18464));
#8575=EDGE_LOOP('',(#18465,#18466,#18467,#18468));
#8576=EDGE_LOOP('',(#18469,#18470,#18471,#18472));
#8577=EDGE_LOOP('',(#18473,#18474,#18475,#18476,#18477,#18478,#18479));
#8578=EDGE_LOOP('',(#18480,#18481,#18482,#18483,#18484,#18485));
#8579=EDGE_LOOP('',(#18486,#18487,#18488,#18489,#18490,#18491));
#8580=EDGE_LOOP('',(#18492,#18493,#18494,#18495));
#8581=EDGE_LOOP('',(#18496,#18497,#18498,#18499));
#8582=EDGE_LOOP('',(#18500,#18501,#18502,#18503));
#8583=EDGE_LOOP('',(#18504,#18505,#18506,#18507,#18508,#18509,#18510));
#8584=EDGE_LOOP('',(#18511,#18512,#18513,#18514,#18515,#18516));
#8585=EDGE_LOOP('',(#18517,#18518,#18519,#18520));
#8586=EDGE_LOOP('',(#18521,#18522,#18523,#18524));
#8587=EDGE_LOOP('',(#18525,#18526,#18527,#18528));
#8588=EDGE_LOOP('',(#18529,#18530,#18531,#18532));
#8589=EDGE_LOOP('',(#18533,#18534,#18535,#18536,#18537));
#8590=EDGE_LOOP('',(#18538,#18539,#18540,#18541));
#8591=EDGE_LOOP('',(#18542,#18543,#18544,#18545));
#8592=EDGE_LOOP('',(#18546,#18547,#18548,#18549));
#8593=EDGE_LOOP('',(#18550,#18551,#18552,#18553));
#8594=EDGE_LOOP('',(#18554,#18555,#18556,#18557,#18558));
#8595=EDGE_LOOP('',(#18559,#18560,#18561,#18562,#18563));
#8596=EDGE_LOOP('',(#18564,#18565,#18566,#18567));
#8597=EDGE_LOOP('',(#18568,#18569,#18570,#18571));
#8598=EDGE_LOOP('',(#18572,#18573,#18574,#18575));
#8599=EDGE_LOOP('',(#18576,#18577,#18578,#18579));
#8600=EDGE_LOOP('',(#18580,#18581,#18582,#18583,#18584,#18585));
#8601=EDGE_LOOP('',(#18586,#18587,#18588,#18589,#18590,#18591));
#8602=EDGE_LOOP('',(#18592,#18593,#18594,#18595));
#8603=EDGE_LOOP('',(#18596,#18597,#18598,#18599));
#8604=EDGE_LOOP('',(#18600,#18601,#18602,#18603));
#8605=EDGE_LOOP('',(#18604,#18605,#18606,#18607));
#8606=EDGE_LOOP('',(#18608,#18609,#18610,#18611,#18612));
#8607=EDGE_LOOP('',(#18613,#18614,#18615,#18616));
#8608=EDGE_LOOP('',(#18617,#18618,#18619,#18620));
#8609=EDGE_LOOP('',(#18621,#18622,#18623,#18624));
#8610=EDGE_LOOP('',(#18625,#18626,#18627,#18628));
#8611=EDGE_LOOP('',(#18629,#18630,#18631,#18632,#18633,#18634));
#8612=EDGE_LOOP('',(#18635,#18636,#18637,#18638,#18639,#18640));
#8613=EDGE_LOOP('',(#18641,#18642,#18643,#18644));
#8614=EDGE_LOOP('',(#18645,#18646,#18647,#18648));
#8615=EDGE_LOOP('',(#18649,#18650,#18651,#18652));
#8616=EDGE_LOOP('',(#18653,#18654,#18655,#18656));
#8617=EDGE_LOOP('',(#18657,#18658,#18659,#18660,#18661));
#8618=EDGE_LOOP('',(#18662,#18663,#18664,#18665));
#8619=EDGE_LOOP('',(#18666,#18667,#18668,#18669));
#8620=EDGE_LOOP('',(#18670,#18671,#18672,#18673));
#8621=EDGE_LOOP('',(#18674,#18675,#18676,#18677));
#8622=EDGE_LOOP('',(#18678,#18679,#18680,#18681));
#8623=EDGE_LOOP('',(#18682));
#8624=EDGE_LOOP('',(#18683));
#8625=EDGE_LOOP('',(#18684));
#8626=EDGE_LOOP('',(#18685));
#8627=EDGE_LOOP('',(#18686));
#8628=EDGE_LOOP('',(#18687));
#8629=EDGE_LOOP('',(#18688));
#8630=EDGE_LOOP('',(#18689));
#8631=EDGE_LOOP('',(#18690));
#8632=EDGE_LOOP('',(#18691,#18692,#18693,#18694,#18695,#18696,#18697,#18698,
#18699,#18700,#18701,#18702,#18703,#18704,#18705,#18706,#18707,#18708,#18709,
#18710,#18711,#18712,#18713,#18714));
#8633=EDGE_LOOP('',(#18715,#18716,#18717,#18718,#18719));
#8634=EDGE_LOOP('',(#18720,#18721,#18722,#18723));
#8635=EDGE_LOOP('',(#18724,#18725,#18726,#18727,#18728));
#8636=EDGE_LOOP('',(#18729,#18730,#18731,#18732));
#8637=EDGE_LOOP('',(#18733,#18734,#18735,#18736));
#8638=EDGE_LOOP('',(#18737));
#8639=EDGE_LOOP('',(#18738,#18739,#18740,#18741,#18742,#18743,#18744,#18745,
#18746,#18747,#18748,#18749,#18750,#18751,#18752,#18753,#18754,#18755,#18756,
#18757,#18758,#18759,#18760,#18761,#18762));
#8640=EDGE_LOOP('',(#18763,#18764,#18765,#18766));
#8641=EDGE_LOOP('',(#18767,#18768,#18769,#18770));
#8642=EDGE_LOOP('',(#18771));
#8643=EDGE_LOOP('',(#18772,#18773,#18774,#18775,#18776,#18777,#18778,#18779,
#18780,#18781,#18782,#18783,#18784,#18785,#18786,#18787,#18788,#18789,#18790,
#18791,#18792,#18793,#18794,#18795,#18796,#18797,#18798,#18799,#18800,#18801,
#18802,#18803,#18804,#18805,#18806));
#8644=EDGE_LOOP('',(#18807,#18808,#18809,#18810,#18811,#18812,#18813,#18814,
#18815,#18816,#18817));
#8645=EDGE_LOOP('',(#18818,#18819,#18820,#18821,#18822,#18823,#18824,#18825,
#18826,#18827,#18828,#18829));
#8646=EDGE_LOOP('',(#18830,#18831,#18832,#18833,#18834,#18835,#18836,#18837,
#18838,#18839,#18840,#18841,#18842,#18843));
#8647=EDGE_LOOP('',(#18844,#18845,#18846,#18847,#18848,#18849,#18850,#18851,
#18852,#18853,#18854,#18855,#18856,#18857,#18858,#18859,#18860,#18861,#18862,
#18863,#18864,#18865,#18866,#18867,#18868,#18869));
#8648=EDGE_LOOP('',(#18870,#18871,#18872,#18873,#18874));
#8649=EDGE_LOOP('',(#18875,#18876,#18877,#18878));
#8650=EDGE_LOOP('',(#18879,#18880,#18881));
#8651=EDGE_LOOP('',(#18882,#18883,#18884,#18885));
#8652=EDGE_LOOP('',(#18886,#18887,#18888,#18889));
#8653=EDGE_LOOP('',(#18890,#18891,#18892,#18893));
#8654=EDGE_LOOP('',(#18894,#18895,#18896,#18897,#18898,#18899,#18900,#18901,
#18902,#18903,#18904,#18905,#18906,#18907,#18908,#18909,#18910,#18911,#18912,
#18913,#18914,#18915,#18916,#18917,#18918,#18919,#18920,#18921));
#8655=EDGE_LOOP('',(#18922,#18923,#18924,#18925,#18926));
#8656=EDGE_LOOP('',(#18927,#18928,#18929,#18930));
#8657=EDGE_LOOP('',(#18931,#18932,#18933,#18934));
#8658=EDGE_LOOP('',(#18935,#18936,#18937,#18938));
#8659=EDGE_LOOP('',(#18939,#18940,#18941,#18942));
#8660=EDGE_LOOP('',(#18943,#18944,#18945,#18946));
#8661=EDGE_LOOP('',(#18947,#18948,#18949,#18950,#18951));
#8662=EDGE_LOOP('',(#18952,#18953,#18954,#18955,#18956,#18957,#18958,#18959,
#18960,#18961,#18962));
#8663=EDGE_LOOP('',(#18963,#18964,#18965,#18966,#18967,#18968,#18969,#18970,
#18971,#18972,#18973,#18974,#18975,#18976,#18977,#18978,#18979,#18980,#18981,
#18982,#18983));
#8664=EDGE_LOOP('',(#18984,#18985,#18986,#18987,#18988,#18989));
#8665=EDGE_LOOP('',(#18990,#18991,#18992,#18993,#18994,#18995));
#8666=EDGE_LOOP('',(#18996,#18997,#18998,#18999,#19000,#19001));
#8667=EDGE_LOOP('',(#19002,#19003,#19004,#19005,#19006,#19007));
#8668=EDGE_LOOP('',(#19008,#19009,#19010,#19011,#19012));
#8669=EDGE_LOOP('',(#19013,#19014,#19015,#19016));
#8670=EDGE_LOOP('',(#19017,#19018,#19019,#19020));
#8671=EDGE_LOOP('',(#19021,#19022,#19023,#19024));
#8672=EDGE_LOOP('',(#19025,#19026,#19027,#19028,#19029));
#8673=EDGE_LOOP('',(#19030,#19031,#19032,#19033));
#8674=EDGE_LOOP('',(#19034,#19035,#19036,#19037));
#8675=EDGE_LOOP('',(#19038,#19039,#19040,#19041));
#8676=EDGE_LOOP('',(#19042,#19043,#19044,#19045));
#8677=EDGE_LOOP('',(#19046,#19047,#19048,#19049));
#8678=EDGE_LOOP('',(#19050,#19051,#19052,#19053,#19054,#19055,#19056));
#8679=EDGE_LOOP('',(#19057,#19058,#19059,#19060));
#8680=EDGE_LOOP('',(#19061,#19062,#19063,#19064,#19065,#19066,#19067,#19068));
#8681=EDGE_LOOP('',(#19069,#19070,#19071,#19072));
#8682=EDGE_LOOP('',(#19073,#19074,#19075,#19076));
#8683=EDGE_LOOP('',(#19077,#19078,#19079,#19080));
#8684=EDGE_LOOP('',(#19081,#19082,#19083,#19084));
#8685=EDGE_LOOP('',(#19085,#19086,#19087,#19088));
#8686=EDGE_LOOP('',(#19089,#19090,#19091,#19092));
#8687=EDGE_LOOP('',(#19093,#19094,#19095,#19096));
#8688=EDGE_LOOP('',(#19097,#19098,#19099,#19100));
#8689=EDGE_LOOP('',(#19101,#19102,#19103,#19104));
#8690=EDGE_LOOP('',(#19105,#19106,#19107,#19108));
#8691=EDGE_LOOP('',(#19109,#19110,#19111,#19112));
#8692=EDGE_LOOP('',(#19113,#19114,#19115,#19116,#19117,#19118,#19119,#19120,
#19121,#19122,#19123,#19124));
#8693=EDGE_LOOP('',(#19125,#19126,#19127,#19128));
#8694=EDGE_LOOP('',(#19129,#19130,#19131,#19132));
#8695=EDGE_LOOP('',(#19133,#19134,#19135,#19136));
#8696=EDGE_LOOP('',(#19137,#19138,#19139,#19140));
#8697=EDGE_LOOP('',(#19141,#19142,#19143,#19144));
#8698=EDGE_LOOP('',(#19145,#19146,#19147,#19148));
#8699=EDGE_LOOP('',(#19149,#19150,#19151,#19152));
#8700=EDGE_LOOP('',(#19153,#19154,#19155,#19156));
#8701=EDGE_LOOP('',(#19157,#19158,#19159,#19160));
#8702=EDGE_LOOP('',(#19161,#19162,#19163,#19164));
#8703=EDGE_LOOP('',(#19165,#19166,#19167,#19168));
#8704=EDGE_LOOP('',(#19169,#19170,#19171,#19172));
#8705=EDGE_LOOP('',(#19173,#19174,#19175,#19176));
#8706=EDGE_LOOP('',(#19177,#19178,#19179,#19180,#19181,#19182,#19183,#19184,
#19185,#19186,#19187,#19188,#19189,#19190));
#8707=EDGE_LOOP('',(#19191,#19192,#19193,#19194));
#8708=EDGE_LOOP('',(#19195,#19196,#19197,#19198));
#8709=EDGE_LOOP('',(#19199,#19200,#19201,#19202));
#8710=EDGE_LOOP('',(#19203,#19204,#19205,#19206));
#8711=EDGE_LOOP('',(#19207,#19208,#19209,#19210));
#8712=EDGE_LOOP('',(#19211,#19212,#19213,#19214));
#8713=EDGE_LOOP('',(#19215,#19216,#19217,#19218));
#8714=EDGE_LOOP('',(#19219,#19220,#19221,#19222));
#8715=EDGE_LOOP('',(#19223,#19224,#19225,#19226));
#8716=EDGE_LOOP('',(#19227,#19228,#19229,#19230));
#8717=EDGE_LOOP('',(#19231,#19232,#19233,#19234));
#8718=EDGE_LOOP('',(#19235,#19236,#19237,#19238));
#8719=EDGE_LOOP('',(#19239,#19240,#19241,#19242));
#8720=EDGE_LOOP('',(#19243,#19244,#19245,#19246));
#8721=EDGE_LOOP('',(#19247,#19248,#19249,#19250));
#8722=EDGE_LOOP('',(#19251,#19252,#19253,#19254));
#8723=EDGE_LOOP('',(#19255,#19256,#19257,#19258));
#8724=EDGE_LOOP('',(#19259,#19260,#19261,#19262));
#8725=EDGE_LOOP('',(#19263,#19264,#19265,#19266));
#8726=EDGE_LOOP('',(#19267,#19268,#19269,#19270));
#8727=EDGE_LOOP('',(#19271,#19272,#19273,#19274));
#8728=EDGE_LOOP('',(#19275,#19276,#19277,#19278));
#8729=EDGE_LOOP('',(#19279,#19280,#19281,#19282));
#8730=EDGE_LOOP('',(#19283,#19284,#19285,#19286));
#8731=EDGE_LOOP('',(#19287,#19288,#19289,#19290));
#8732=EDGE_LOOP('',(#19291,#19292,#19293,#19294));
#8733=EDGE_LOOP('',(#19295,#19296,#19297,#19298));
#8734=EDGE_LOOP('',(#19299,#19300,#19301,#19302));
#8735=EDGE_LOOP('',(#19303,#19304,#19305,#19306));
#8736=EDGE_LOOP('',(#19307,#19308,#19309,#19310));
#8737=EDGE_LOOP('',(#19311,#19312,#19313,#19314));
#8738=EDGE_LOOP('',(#19315,#19316,#19317,#19318));
#8739=EDGE_LOOP('',(#19319,#19320,#19321,#19322));
#8740=EDGE_LOOP('',(#19323,#19324,#19325,#19326));
#8741=EDGE_LOOP('',(#19327,#19328,#19329,#19330));
#8742=EDGE_LOOP('',(#19331,#19332,#19333,#19334,#19335,#19336,#19337,#19338,
#19339,#19340,#19341,#19342,#19343,#19344,#19345,#19346,#19347,#19348,#19349,
#19350,#19351,#19352,#19353,#19354,#19355,#19356,#19357,#19358,#19359,#19360,
#19361,#19362,#19363,#19364,#19365));
#8743=EDGE_LOOP('',(#19366,#19367,#19368,#19369));
#8744=EDGE_LOOP('',(#19370,#19371,#19372,#19373));
#8745=EDGE_LOOP('',(#19374,#19375,#19376,#19377));
#8746=EDGE_LOOP('',(#19378,#19379,#19380,#19381));
#8747=EDGE_LOOP('',(#19382,#19383,#19384,#19385));
#8748=EDGE_LOOP('',(#19386,#19387,#19388,#19389));
#8749=EDGE_LOOP('',(#19390,#19391,#19392,#19393,#19394));
#8750=EDGE_LOOP('',(#19395,#19396,#19397,#19398));
#8751=EDGE_LOOP('',(#19399,#19400,#19401,#19402));
#8752=EDGE_LOOP('',(#19403,#19404,#19405,#19406));
#8753=EDGE_LOOP('',(#19407,#19408,#19409,#19410));
#8754=EDGE_LOOP('',(#19411,#19412,#19413,#19414));
#8755=EDGE_LOOP('',(#19415,#19416,#19417,#19418));
#8756=EDGE_LOOP('',(#19419,#19420,#19421,#19422));
#8757=EDGE_LOOP('',(#19423,#19424,#19425,#19426));
#8758=EDGE_LOOP('',(#19427,#19428,#19429,#19430));
#8759=EDGE_LOOP('',(#19431,#19432,#19433,#19434));
#8760=EDGE_LOOP('',(#19435,#19436,#19437,#19438,#19439,#19440,#19441,#19442,
#19443,#19444,#19445,#19446,#19447,#19448,#19449,#19450,#19451,#19452,#19453));
#8761=EDGE_LOOP('',(#19454,#19455,#19456,#19457));
#8762=EDGE_LOOP('',(#19458,#19459,#19460,#19461));
#8763=EDGE_LOOP('',(#19462,#19463,#19464,#19465));
#8764=EDGE_LOOP('',(#19466,#19467,#19468,#19469));
#8765=EDGE_LOOP('',(#19470,#19471,#19472,#19473));
#8766=EDGE_LOOP('',(#19474,#19475,#19476,#19477));
#8767=EDGE_LOOP('',(#19478,#19479,#19480,#19481));
#8768=EDGE_LOOP('',(#19482,#19483,#19484,#19485));
#8769=EDGE_LOOP('',(#19486,#19487,#19488,#19489));
#8770=EDGE_LOOP('',(#19490,#19491,#19492,#19493));
#8771=EDGE_LOOP('',(#19494,#19495,#19496,#19497));
#8772=EDGE_LOOP('',(#19498,#19499,#19500,#19501,#19502,#19503,#19504,#19505,
#19506,#19507,#19508));
#8773=EDGE_LOOP('',(#19509,#19510,#19511,#19512,#19513,#19514));
#8774=EDGE_LOOP('',(#19515,#19516,#19517,#19518,#19519,#19520));
#8775=EDGE_LOOP('',(#19521,#19522,#19523,#19524,#19525,#19526));
#8776=EDGE_LOOP('',(#19527,#19528,#19529,#19530,#19531,#19532));
#8777=EDGE_LOOP('',(#19533));
#8778=EDGE_LOOP('',(#19534));
#8779=EDGE_LOOP('',(#19535,#19536,#19537,#19538));
#8780=EDGE_LOOP('',(#19539,#19540,#19541,#19542));
#8781=EDGE_LOOP('',(#19543,#19544,#19545,#19546));
#8782=EDGE_LOOP('',(#19547,#19548,#19549,#19550,#19551));
#8783=EDGE_LOOP('',(#19552,#19553,#19554,#19555));
#8784=EDGE_LOOP('',(#19556,#19557,#19558,#19559));
#8785=EDGE_LOOP('',(#19560,#19561,#19562,#19563));
#8786=EDGE_LOOP('',(#19564,#19565,#19566,#19567,#19568,#19569,#19570,#19571));
#8787=EDGE_LOOP('',(#19572));
#8788=EDGE_LOOP('',(#19573,#19574,#19575,#19576));
#8789=EDGE_LOOP('',(#19577));
#8790=EDGE_LOOP('',(#19578));
#8791=EDGE_LOOP('',(#19579,#19580,#19581,#19582));
#8792=EDGE_LOOP('',(#19583,#19584,#19585,#19586,#19587,#19588,#19589,#19590,
#19591,#19592,#19593));
#8793=EDGE_LOOP('',(#19594));
#8794=EDGE_LOOP('',(#19595,#19596,#19597,#19598,#19599,#19600,#19601,#19602));
#8795=EDGE_LOOP('',(#19603));
#8796=EDGE_LOOP('',(#19604,#19605,#19606,#19607));
#8797=EDGE_LOOP('',(#19608,#19609,#19610,#19611));
#8798=EDGE_LOOP('',(#19612,#19613,#19614,#19615));
#8799=EDGE_LOOP('',(#19616,#19617,#19618,#19619));
#8800=EDGE_LOOP('',(#19620,#19621,#19622,#19623,#19624));
#8801=EDGE_LOOP('',(#19625,#19626,#19627,#19628,#19629,#19630,#19631,#19632,
#19633,#19634,#19635,#19636,#19637));
#8802=EDGE_LOOP('',(#19638,#19639,#19640,#19641,#19642,#19643,#19644,#19645));
#8803=EDGE_LOOP('',(#19646,#19647,#19648,#19649,#19650,#19651));
#8804=EDGE_LOOP('',(#19652,#19653,#19654,#19655,#19656));
#8805=EDGE_LOOP('',(#19657,#19658,#19659,#19660));
#8806=EDGE_LOOP('',(#19661,#19662,#19663,#19664,#19665,#19666,#19667,#19668));
#8807=EDGE_LOOP('',(#19669,#19670,#19671,#19672,#19673,#19674));
#8808=EDGE_LOOP('',(#19675,#19676,#19677,#19678));
#8809=EDGE_LOOP('',(#19679,#19680,#19681,#19682,#19683));
#8810=EDGE_LOOP('',(#19684,#19685,#19686,#19687,#19688,#19689));
#8811=EDGE_LOOP('',(#19690,#19691,#19692,#19693,#19694));
#8812=EDGE_LOOP('',(#19695,#19696,#19697,#19698));
#8813=EDGE_LOOP('',(#19699,#19700,#19701,#19702,#19703,#19704));
#8814=EDGE_LOOP('',(#19705,#19706,#19707,#19708));
#8815=EDGE_LOOP('',(#19709,#19710,#19711,#19712,#19713,#19714,#19715,#19716));
#8816=EDGE_LOOP('',(#19717));
#8817=EDGE_LOOP('',(#19718));
#8818=EDGE_LOOP('',(#19719,#19720,#19721,#19722,#19723,#19724,#19725,#19726));
#8819=EDGE_LOOP('',(#19727));
#8820=EDGE_LOOP('',(#19728));
#8821=EDGE_LOOP('',(#19729,#19730,#19731,#19732));
#8822=EDGE_LOOP('',(#19733,#19734,#19735,#19736));
#8823=EDGE_LOOP('',(#19737,#19738,#19739,#19740));
#8824=EDGE_LOOP('',(#19741,#19742,#19743,#19744));
#8825=EDGE_LOOP('',(#19745));
#8826=EDGE_LOOP('',(#19746));
#8827=EDGE_LOOP('',(#19747));
#8828=EDGE_LOOP('',(#19748));
#8829=EDGE_LOOP('',(#19749));
#8830=EDGE_LOOP('',(#19750));
#8831=EDGE_LOOP('',(#19751,#19752,#19753,#19754));
#8832=EDGE_LOOP('',(#19755,#19756,#19757,#19758));
#8833=EDGE_LOOP('',(#19759,#19760,#19761,#19762));
#8834=EDGE_LOOP('',(#19763,#19764,#19765,#19766));
#8835=EDGE_LOOP('',(#19767,#19768,#19769,#19770));
#8836=EDGE_LOOP('',(#19771,#19772,#19773,#19774));
#8837=EDGE_LOOP('',(#19775,#19776,#19777,#19778));
#8838=EDGE_LOOP('',(#19779,#19780,#19781,#19782));
#8839=EDGE_LOOP('',(#19783,#19784,#19785,#19786,#19787,#19788,#19789,#19790));
#8840=EDGE_LOOP('',(#19791));
#8841=EDGE_LOOP('',(#19792));
#8842=EDGE_LOOP('',(#19793,#19794,#19795,#19796));
#8843=EDGE_LOOP('',(#19797,#19798,#19799,#19800));
#8844=EDGE_LOOP('',(#19801,#19802,#19803,#19804));
#8845=EDGE_LOOP('',(#19805));
#8846=EDGE_LOOP('',(#19806));
#8847=EDGE_LOOP('',(#19807));
#8848=EDGE_LOOP('',(#19808));
#8849=EDGE_LOOP('',(#19809));
#8850=EDGE_LOOP('',(#19810));
#8851=EDGE_LOOP('',(#19811,#19812,#19813,#19814));
#8852=EDGE_LOOP('',(#19815));
#8853=EDGE_LOOP('',(#19816));
#8854=EDGE_LOOP('',(#19817));
#8855=EDGE_LOOP('',(#19818));
#8856=EDGE_LOOP('',(#19819));
#8857=EDGE_LOOP('',(#19820));
#8858=EDGE_LOOP('',(#19821,#19822,#19823,#19824));
#8859=EDGE_LOOP('',(#19825,#19826,#19827,#19828));
#8860=EDGE_LOOP('',(#19829,#19830,#19831,#19832));
#8861=EDGE_LOOP('',(#19833,#19834,#19835,#19836));
#8862=EDGE_LOOP('',(#19837,#19838,#19839,#19840,#19841,#19842,#19843,#19844,
#19845,#19846,#19847,#19848,#19849,#19850,#19851,#19852,#19853,#19854,#19855,
#19856,#19857,#19858));
#8863=EDGE_LOOP('',(#19859,#19860,#19861,#19862));
#8864=EDGE_LOOP('',(#19863,#19864));
#8865=EDGE_LOOP('',(#19865,#19866,#19867,#19868));
#8866=EDGE_LOOP('',(#19869,#19870));
#8867=EDGE_LOOP('',(#19871,#19872,#19873,#19874));
#8868=EDGE_LOOP('',(#19875,#19876));
#8869=EDGE_LOOP('',(#19877,#19878,#19879,#19880));
#8870=EDGE_LOOP('',(#19881,#19882,#19883,#19884));
#8871=EDGE_LOOP('',(#19885,#19886,#19887,#19888));
#8872=EDGE_LOOP('',(#19889,#19890,#19891,#19892));
#8873=EDGE_LOOP('',(#19893,#19894,#19895,#19896));
#8874=EDGE_LOOP('',(#19897,#19898,#19899,#19900));
#8875=EDGE_LOOP('',(#19901,#19902,#19903,#19904));
#8876=EDGE_LOOP('',(#19905,#19906,#19907,#19908));
#8877=EDGE_LOOP('',(#19909,#19910,#19911,#19912));
#8878=EDGE_LOOP('',(#19913,#19914,#19915,#19916,#19917));
#8879=EDGE_LOOP('',(#19918,#19919,#19920,#19921));
#8880=EDGE_LOOP('',(#19922,#19923,#19924,#19925));
#8881=EDGE_LOOP('',(#19926,#19927,#19928,#19929));
#8882=EDGE_LOOP('',(#19930,#19931,#19932,#19933,#19934,#19935));
#8883=EDGE_LOOP('',(#19936,#19937,#19938,#19939,#19940,#19941,#19942));
#8884=EDGE_LOOP('',(#19943,#19944,#19945,#19946));
#8885=EDGE_LOOP('',(#19947,#19948,#19949,#19950));
#8886=EDGE_LOOP('',(#19951,#19952,#19953,#19954));
#8887=EDGE_LOOP('',(#19955,#19956,#19957,#19958));
#8888=EDGE_LOOP('',(#19959,#19960,#19961,#19962));
#8889=EDGE_LOOP('',(#19963,#19964,#19965,#19966,#19967));
#8890=EDGE_LOOP('',(#19968,#19969,#19970,#19971,#19972));
#8891=EDGE_LOOP('',(#19973,#19974,#19975,#19976));
#8892=EDGE_LOOP('',(#19977));
#8893=EDGE_LOOP('',(#19978));
#8894=EDGE_LOOP('',(#19979,#19980,#19981,#19982));
#8895=EDGE_LOOP('',(#19983,#19984,#19985,#19986));
#8896=EDGE_LOOP('',(#19987,#19988,#19989,#19990));
#8897=EDGE_LOOP('',(#19991,#19992,#19993,#19994));
#8898=EDGE_LOOP('',(#19995,#19996,#19997,#19998));
#8899=EDGE_LOOP('',(#19999,#20000,#20001,#20002));
#8900=EDGE_LOOP('',(#20003,#20004,#20005,#20006));
#8901=EDGE_LOOP('',(#20007,#20008,#20009,#20010));
#8902=EDGE_LOOP('',(#20011,#20012,#20013,#20014));
#8903=EDGE_LOOP('',(#20015,#20016,#20017,#20018));
#8904=EDGE_LOOP('',(#20019,#20020,#20021,#20022));
#8905=EDGE_LOOP('',(#20023,#20024,#20025,#20026));
#8906=EDGE_LOOP('',(#20027,#20028,#20029,#20030,#20031,#20032,#20033,#20034));
#8907=EDGE_LOOP('',(#20035,#20036,#20037,#20038,#20039,#20040,#20041,#20042));
#8908=EDGE_LOOP('',(#20043,#20044,#20045,#20046));
#8909=EDGE_LOOP('',(#20047,#20048,#20049,#20050));
#8910=EDGE_LOOP('',(#20051,#20052,#20053,#20054));
#8911=EDGE_LOOP('',(#20055,#20056,#20057,#20058));
#8912=EDGE_LOOP('',(#20059,#20060,#20061,#20062));
#8913=EDGE_LOOP('',(#20063,#20064,#20065,#20066));
#8914=EDGE_LOOP('',(#20067,#20068,#20069,#20070));
#8915=EDGE_LOOP('',(#20071,#20072,#20073,#20074));
#8916=EDGE_LOOP('',(#20075,#20076,#20077,#20078));
#8917=EDGE_LOOP('',(#20079,#20080,#20081,#20082));
#8918=EDGE_LOOP('',(#20083,#20084,#20085,#20086));
#8919=EDGE_LOOP('',(#20087,#20088,#20089,#20090,#20091));
#8920=EDGE_LOOP('',(#20092,#20093,#20094,#20095,#20096,#20097,#20098,#20099));
#8921=EDGE_LOOP('',(#20100,#20101,#20102,#20103));
#8922=EDGE_LOOP('',(#20104,#20105,#20106,#20107));
#8923=EDGE_LOOP('',(#20108,#20109,#20110,#20111));
#8924=EDGE_LOOP('',(#20112,#20113,#20114,#20115));
#8925=EDGE_LOOP('',(#20116,#20117,#20118,#20119));
#8926=EDGE_LOOP('',(#20120,#20121,#20122,#20123));
#8927=EDGE_LOOP('',(#20124,#20125,#20126,#20127));
#8928=EDGE_LOOP('',(#20128,#20129,#20130,#20131));
#8929=EDGE_LOOP('',(#20132,#20133,#20134,#20135));
#8930=EDGE_LOOP('',(#20136,#20137,#20138,#20139,#20140,#20141,#20142,#20143,
#20144,#20145,#20146,#20147));
#8931=EDGE_LOOP('',(#20148,#20149,#20150,#20151));
#8932=EDGE_LOOP('',(#20152,#20153,#20154,#20155,#20156,#20157,#20158,#20159));
#8933=EDGE_LOOP('',(#20160));
#8934=EDGE_LOOP('',(#20161,#20162,#20163,#20164));
#8935=EDGE_LOOP('',(#20165,#20166,#20167,#20168));
#8936=EDGE_LOOP('',(#20169,#20170,#20171,#20172));
#8937=EDGE_LOOP('',(#20173,#20174,#20175,#20176));
#8938=EDGE_LOOP('',(#20177,#20178,#20179,#20180));
#8939=EDGE_LOOP('',(#20181,#20182,#20183,#20184));
#8940=EDGE_LOOP('',(#20185,#20186,#20187,#20188));
#8941=EDGE_LOOP('',(#20189,#20190,#20191,#20192));
#8942=EDGE_LOOP('',(#20193,#20194,#20195,#20196));
#8943=EDGE_LOOP('',(#20197,#20198,#20199,#20200));
#8944=EDGE_LOOP('',(#20201,#20202,#20203,#20204));
#8945=EDGE_LOOP('',(#20205,#20206,#20207,#20208));
#8946=EDGE_LOOP('',(#20209,#20210,#20211,#20212));
#8947=EDGE_LOOP('',(#20213,#20214,#20215,#20216));
#8948=EDGE_LOOP('',(#20217,#20218,#20219,#20220));
#8949=EDGE_LOOP('',(#20221,#20222,#20223,#20224));
#8950=EDGE_LOOP('',(#20225,#20226,#20227,#20228));
#8951=EDGE_LOOP('',(#20229,#20230,#20231,#20232));
#8952=EDGE_LOOP('',(#20233,#20234,#20235,#20236));
#8953=EDGE_LOOP('',(#20237,#20238,#20239,#20240));
#8954=EDGE_LOOP('',(#20241,#20242,#20243,#20244));
#8955=EDGE_LOOP('',(#20245,#20246,#20247,#20248));
#8956=EDGE_LOOP('',(#20249,#20250,#20251,#20252));
#8957=EDGE_LOOP('',(#20253));
#8958=EDGE_LOOP('',(#20254));
#8959=EDGE_LOOP('',(#20255));
#8960=EDGE_LOOP('',(#20256));
#8961=EDGE_LOOP('',(#20257,#20258,#20259,#20260));
#8962=EDGE_LOOP('',(#20261,#20262,#20263,#20264));
#8963=EDGE_LOOP('',(#20265,#20266,#20267,#20268));
#8964=EDGE_LOOP('',(#20269,#20270,#20271,#20272));
#8965=EDGE_LOOP('',(#20273,#20274,#20275,#20276));
#8966=EDGE_LOOP('',(#20277,#20278,#20279,#20280));
#8967=EDGE_LOOP('',(#20281));
#8968=EDGE_LOOP('',(#20282));
#8969=EDGE_LOOP('',(#20283,#20284,#20285,#20286));
#8970=EDGE_LOOP('',(#20287));
#8971=EDGE_LOOP('',(#20288));
#8972=EDGE_LOOP('',(#20289,#20290,#20291,#20292));
#8973=EDGE_LOOP('',(#20293,#20294,#20295,#20296));
#8974=EDGE_LOOP('',(#20297,#20298,#20299,#20300,#20301));
#8975=EDGE_LOOP('',(#20302,#20303,#20304,#20305,#20306,#20307,#20308,#20309));
#8976=EDGE_LOOP('',(#20310,#20311,#20312,#20313,#20314));
#8977=EDGE_LOOP('',(#20315,#20316,#20317,#20318));
#8978=EDGE_LOOP('',(#20319,#20320,#20321,#20322));
#8979=EDGE_LOOP('',(#20323,#20324,#20325,#20326));
#8980=EDGE_LOOP('',(#20327,#20328,#20329,#20330));
#8981=EDGE_LOOP('',(#20331,#20332,#20333,#20334));
#8982=EDGE_LOOP('',(#20335,#20336,#20337,#20338));
#8983=EDGE_LOOP('',(#20339,#20340,#20341,#20342));
#8984=EDGE_LOOP('',(#20343,#20344,#20345,#20346));
#8985=EDGE_LOOP('',(#20347,#20348,#20349,#20350,#20351));
#8986=EDGE_LOOP('',(#20352,#20353,#20354,#20355,#20356));
#8987=EDGE_LOOP('',(#20357,#20358,#20359,#20360,#20361));
#8988=EDGE_LOOP('',(#20362,#20363,#20364,#20365));
#8989=EDGE_LOOP('',(#20366,#20367,#20368,#20369));
#8990=EDGE_LOOP('',(#20370,#20371,#20372,#20373,#20374,#20375,#20376,#20377));
#8991=EDGE_LOOP('',(#20378,#20379,#20380,#20381));
#8992=EDGE_LOOP('',(#20382,#20383,#20384,#20385));
#8993=EDGE_LOOP('',(#20386,#20387,#20388,#20389));
#8994=EDGE_LOOP('',(#20390,#20391,#20392,#20393));
#8995=EDGE_LOOP('',(#20394,#20395,#20396,#20397));
#8996=EDGE_LOOP('',(#20398,#20399,#20400,#20401));
#8997=EDGE_LOOP('',(#20402,#20403,#20404,#20405,#20406,#20407,#20408,#20409,
#20410,#20411,#20412,#20413,#20414,#20415,#20416,#20417,#20418,#20419,#20420,
#20421,#20422,#20423,#20424,#20425,#20426,#20427,#20428,#20429,#20430,#20431,
#20432,#20433,#20434,#20435,#20436,#20437,#20438,#20439,#20440,#20441,#20442,
#20443,#20444,#20445,#20446,#20447,#20448,#20449,#20450,#20451,#20452,#20453,
#20454,#20455,#20456,#20457,#20458,#20459,#20460,#20461,#20462,#20463,#20464,
#20465,#20466,#20467,#20468,#20469,#20470,#20471,#20472,#20473,#20474,#20475,
#20476,#20477,#20478,#20479,#20480,#20481,#20482,#20483,#20484,#20485,#20486,
#20487,#20488,#20489,#20490,#20491,#20492,#20493,#20494,#20495,#20496,#20497,
#20498,#20499,#20500,#20501,#20502,#20503,#20504,#20505,#20506,#20507,#20508,
#20509,#20510,#20511,#20512,#20513,#20514,#20515,#20516,#20517,#20518,#20519,
#20520,#20521,#20522,#20523,#20524,#20525,#20526,#20527,#20528,#20529,#20530,
#20531,#20532,#20533,#20534,#20535,#20536,#20537,#20538,#20539,#20540,#20541,
#20542,#20543,#20544,#20545,#20546,#20547,#20548,#20549,#20550,#20551,#20552,
#20553,#20554,#20555,#20556,#20557,#20558,#20559,#20560,#20561,#20562,#20563,
#20564,#20565,#20566,#20567,#20568,#20569,#20570,#20571,#20572,#20573,#20574,
#20575,#20576,#20577,#20578,#20579,#20580,#20581,#20582,#20583,#20584,#20585,
#20586,#20587,#20588,#20589,#20590,#20591,#20592,#20593,#20594,#20595,#20596,
#20597,#20598,#20599,#20600,#20601,#20602,#20603,#20604,#20605,#20606,#20607,
#20608,#20609,#20610,#20611,#20612,#20613,#20614,#20615,#20616,#20617,#20618,
#20619,#20620,#20621,#20622,#20623,#20624,#20625,#20626,#20627,#20628,#20629,
#20630,#20631,#20632,#20633,#20634,#20635,#20636,#20637,#20638,#20639,#20640,
#20641,#20642,#20643,#20644,#20645,#20646,#20647,#20648,#20649,#20650,#20651,
#20652,#20653,#20654,#20655,#20656,#20657,#20658,#20659,#20660,#20661,#20662,
#20663,#20664,#20665,#20666,#20667,#20668,#20669,#20670,#20671,#20672,#20673,
#20674,#20675,#20676,#20677,#20678,#20679,#20680,#20681,#20682,#20683,#20684,
#20685,#20686,#20687,#20688,#20689,#20690,#20691,#20692,#20693,#20694,#20695,
#20696,#20697,#20698,#20699,#20700,#20701,#20702,#20703,#20704,#20705,#20706,
#20707,#20708,#20709,#20710,#20711,#20712,#20713,#20714,#20715,#20716,#20717,
#20718,#20719,#20720,#20721,#20722,#20723,#20724,#20725,#20726,#20727,#20728,
#20729,#20730,#20731,#20732,#20733,#20734,#20735,#20736,#20737,#20738,#20739,
#20740,#20741,#20742,#20743,#20744,#20745,#20746,#20747,#20748,#20749,#20750,
#20751,#20752,#20753,#20754,#20755,#20756,#20757,#20758,#20759,#20760,#20761,
#20762,#20763,#20764,#20765));
#8998=EDGE_LOOP('',(#20766,#20767,#20768,#20769));
#8999=EDGE_LOOP('',(#20770,#20771,#20772,#20773));
#9000=EDGE_LOOP('',(#20774,#20775,#20776,#20777));
#9001=EDGE_LOOP('',(#20778,#20779,#20780,#20781));
#9002=EDGE_LOOP('',(#20782,#20783,#20784,#20785));
#9003=EDGE_LOOP('',(#20786,#20787,#20788,#20789));
#9004=EDGE_LOOP('',(#20790,#20791,#20792,#20793));
#9005=EDGE_LOOP('',(#20794,#20795,#20796,#20797));
#9006=EDGE_LOOP('',(#20798,#20799,#20800,#20801));
#9007=EDGE_LOOP('',(#20802,#20803,#20804,#20805));
#9008=EDGE_LOOP('',(#20806,#20807,#20808,#20809));
#9009=EDGE_LOOP('',(#20810,#20811,#20812,#20813));
#9010=EDGE_LOOP('',(#20814,#20815,#20816,#20817));
#9011=EDGE_LOOP('',(#20818,#20819,#20820,#20821));
#9012=EDGE_LOOP('',(#20822,#20823,#20824,#20825));
#9013=EDGE_LOOP('',(#20826,#20827,#20828,#20829));
#9014=EDGE_LOOP('',(#20830,#20831,#20832,#20833));
#9015=EDGE_LOOP('',(#20834,#20835,#20836,#20837));
#9016=EDGE_LOOP('',(#20838,#20839,#20840,#20841));
#9017=EDGE_LOOP('',(#20842,#20843,#20844,#20845));
#9018=EDGE_LOOP('',(#20846,#20847,#20848,#20849));
#9019=EDGE_LOOP('',(#20850,#20851,#20852,#20853));
#9020=EDGE_LOOP('',(#20854,#20855,#20856,#20857));
#9021=EDGE_LOOP('',(#20858,#20859,#20860,#20861,#20862,#20863,#20864,#20865,
#20866,#20867,#20868,#20869,#20870,#20871,#20872,#20873,#20874,#20875,#20876,
#20877,#20878,#20879,#20880,#20881,#20882,#20883,#20884,#20885,#20886,#20887,
#20888,#20889,#20890,#20891,#20892,#20893,#20894,#20895,#20896,#20897,#20898,
#20899,#20900,#20901,#20902,#20903,#20904,#20905,#20906,#20907,#20908,#20909,
#20910,#20911,#20912,#20913,#20914,#20915,#20916,#20917,#20918,#20919,#20920,
#20921,#20922,#20923,#20924,#20925,#20926,#20927,#20928,#20929,#20930,#20931,
#20932,#20933,#20934,#20935,#20936,#20937,#20938,#20939,#20940,#20941,#20942,
#20943,#20944,#20945,#20946,#20947,#20948,#20949,#20950,#20951,#20952,#20953,
#20954,#20955,#20956,#20957,#20958,#20959,#20960,#20961,#20962,#20963,#20964,
#20965,#20966,#20967,#20968,#20969,#20970,#20971,#20972,#20973,#20974,#20975,
#20976,#20977,#20978));
#9022=EDGE_LOOP('',(#20979,#20980,#20981,#20982,#20983,#20984,#20985,#20986));
#9023=EDGE_LOOP('',(#20987,#20988,#20989,#20990));
#9024=EDGE_LOOP('',(#20991,#20992,#20993,#20994));
#9025=EDGE_LOOP('',(#20995,#20996,#20997,#20998));
#9026=EDGE_LOOP('',(#20999,#21000,#21001,#21002));
#9027=EDGE_LOOP('',(#21003,#21004,#21005,#21006));
#9028=EDGE_LOOP('',(#21007,#21008,#21009,#21010));
#9029=EDGE_LOOP('',(#21011,#21012,#21013,#21014));
#9030=EDGE_LOOP('',(#21015,#21016,#21017,#21018));
#9031=EDGE_LOOP('',(#21019,#21020,#21021,#21022));
#9032=EDGE_LOOP('',(#21023,#21024,#21025,#21026));
#9033=EDGE_LOOP('',(#21027,#21028,#21029,#21030));
#9034=EDGE_LOOP('',(#21031,#21032,#21033,#21034));
#9035=EDGE_LOOP('',(#21035,#21036,#21037,#21038));
#9036=EDGE_LOOP('',(#21039,#21040,#21041,#21042));
#9037=EDGE_LOOP('',(#21043,#21044,#21045,#21046));
#9038=EDGE_LOOP('',(#21047,#21048,#21049,#21050));
#9039=EDGE_LOOP('',(#21051,#21052,#21053,#21054));
#9040=EDGE_LOOP('',(#21055,#21056,#21057,#21058));
#9041=EDGE_LOOP('',(#21059,#21060,#21061,#21062));
#9042=EDGE_LOOP('',(#21063,#21064,#21065,#21066));
#9043=EDGE_LOOP('',(#21067,#21068,#21069,#21070));
#9044=EDGE_LOOP('',(#21071,#21072,#21073,#21074));
#9045=EDGE_LOOP('',(#21075,#21076,#21077,#21078));
#9046=EDGE_LOOP('',(#21079,#21080,#21081,#21082));
#9047=EDGE_LOOP('',(#21083,#21084,#21085,#21086));
#9048=EDGE_LOOP('',(#21087,#21088,#21089,#21090));
#9049=EDGE_LOOP('',(#21091,#21092,#21093,#21094));
#9050=EDGE_LOOP('',(#21095,#21096,#21097,#21098));
#9051=EDGE_LOOP('',(#21099,#21100,#21101,#21102));
#9052=EDGE_LOOP('',(#21103,#21104,#21105,#21106));
#9053=EDGE_LOOP('',(#21107,#21108,#21109,#21110));
#9054=EDGE_LOOP('',(#21111,#21112,#21113,#21114));
#9055=EDGE_LOOP('',(#21115,#21116,#21117,#21118));
#9056=EDGE_LOOP('',(#21119,#21120,#21121,#21122));
#9057=EDGE_LOOP('',(#21123,#21124,#21125,#21126));
#9058=EDGE_LOOP('',(#21127,#21128,#21129,#21130));
#9059=EDGE_LOOP('',(#21131,#21132,#21133,#21134));
#9060=EDGE_LOOP('',(#21135,#21136,#21137,#21138));
#9061=EDGE_LOOP('',(#21139,#21140,#21141,#21142));
#9062=EDGE_LOOP('',(#21143,#21144,#21145,#21146));
#9063=EDGE_LOOP('',(#21147,#21148,#21149,#21150));
#9064=EDGE_LOOP('',(#21151,#21152,#21153,#21154));
#9065=EDGE_LOOP('',(#21155,#21156,#21157,#21158));
#9066=EDGE_LOOP('',(#21159,#21160,#21161,#21162));
#9067=EDGE_LOOP('',(#21163,#21164,#21165,#21166));
#9068=EDGE_LOOP('',(#21167,#21168,#21169,#21170));
#9069=EDGE_LOOP('',(#21171,#21172,#21173,#21174));
#9070=EDGE_LOOP('',(#21175,#21176,#21177,#21178));
#9071=EDGE_LOOP('',(#21179,#21180,#21181,#21182));
#9072=EDGE_LOOP('',(#21183,#21184,#21185,#21186));
#9073=EDGE_LOOP('',(#21187,#21188,#21189,#21190));
#9074=EDGE_LOOP('',(#21191,#21192,#21193,#21194));
#9075=EDGE_LOOP('',(#21195,#21196,#21197,#21198));
#9076=EDGE_LOOP('',(#21199,#21200,#21201,#21202));
#9077=EDGE_LOOP('',(#21203,#21204,#21205,#21206));
#9078=EDGE_LOOP('',(#21207,#21208,#21209,#21210));
#9079=EDGE_LOOP('',(#21211,#21212,#21213,#21214));
#9080=EDGE_LOOP('',(#21215,#21216,#21217,#21218));
#9081=EDGE_LOOP('',(#21219,#21220,#21221,#21222));
#9082=EDGE_LOOP('',(#21223,#21224,#21225,#21226));
#9083=EDGE_LOOP('',(#21227,#21228,#21229,#21230));
#9084=EDGE_LOOP('',(#21231,#21232,#21233,#21234));
#9085=EDGE_LOOP('',(#21235,#21236,#21237,#21238));
#9086=EDGE_LOOP('',(#21239,#21240,#21241,#21242));
#9087=EDGE_LOOP('',(#21243,#21244,#21245,#21246));
#9088=EDGE_LOOP('',(#21247,#21248,#21249,#21250));
#9089=EDGE_LOOP('',(#21251,#21252,#21253,#21254));
#9090=EDGE_LOOP('',(#21255,#21256,#21257,#21258));
#9091=EDGE_LOOP('',(#21259,#21260,#21261,#21262));
#9092=EDGE_LOOP('',(#21263,#21264,#21265,#21266));
#9093=EDGE_LOOP('',(#21267,#21268,#21269,#21270));
#9094=EDGE_LOOP('',(#21271,#21272,#21273,#21274));
#9095=EDGE_LOOP('',(#21275,#21276,#21277,#21278));
#9096=EDGE_LOOP('',(#21279,#21280,#21281,#21282));
#9097=EDGE_LOOP('',(#21283,#21284,#21285,#21286));
#9098=EDGE_LOOP('',(#21287,#21288,#21289,#21290));
#9099=EDGE_LOOP('',(#21291,#21292,#21293,#21294));
#9100=EDGE_LOOP('',(#21295,#21296,#21297,#21298));
#9101=EDGE_LOOP('',(#21299,#21300,#21301,#21302));
#9102=EDGE_LOOP('',(#21303,#21304,#21305,#21306));
#9103=EDGE_LOOP('',(#21307,#21308,#21309,#21310));
#9104=EDGE_LOOP('',(#21311,#21312,#21313,#21314));
#9105=EDGE_LOOP('',(#21315,#21316,#21317,#21318));
#9106=EDGE_LOOP('',(#21319,#21320,#21321,#21322));
#9107=EDGE_LOOP('',(#21323,#21324,#21325,#21326));
#9108=EDGE_LOOP('',(#21327,#21328,#21329,#21330));
#9109=EDGE_LOOP('',(#21331,#21332,#21333,#21334));
#9110=EDGE_LOOP('',(#21335,#21336,#21337,#21338));
#9111=EDGE_LOOP('',(#21339,#21340,#21341,#21342));
#9112=EDGE_LOOP('',(#21343,#21344,#21345,#21346));
#9113=EDGE_LOOP('',(#21347,#21348,#21349,#21350));
#9114=EDGE_LOOP('',(#21351,#21352,#21353,#21354));
#9115=EDGE_LOOP('',(#21355,#21356,#21357,#21358));
#9116=EDGE_LOOP('',(#21359,#21360,#21361,#21362));
#9117=EDGE_LOOP('',(#21363,#21364,#21365,#21366));
#9118=EDGE_LOOP('',(#21367,#21368,#21369,#21370));
#9119=EDGE_LOOP('',(#21371,#21372,#21373,#21374));
#9120=EDGE_LOOP('',(#21375,#21376,#21377,#21378));
#9121=EDGE_LOOP('',(#21379,#21380,#21381,#21382));
#9122=EDGE_LOOP('',(#21383,#21384,#21385,#21386));
#9123=EDGE_LOOP('',(#21387,#21388,#21389,#21390));
#9124=EDGE_LOOP('',(#21391,#21392,#21393,#21394));
#9125=EDGE_LOOP('',(#21395,#21396,#21397,#21398));
#9126=EDGE_LOOP('',(#21399,#21400,#21401,#21402));
#9127=EDGE_LOOP('',(#21403,#21404,#21405,#21406));
#9128=EDGE_LOOP('',(#21407,#21408,#21409,#21410));
#9129=EDGE_LOOP('',(#21411,#21412,#21413,#21414));
#9130=EDGE_LOOP('',(#21415,#21416,#21417,#21418));
#9131=EDGE_LOOP('',(#21419,#21420,#21421,#21422));
#9132=EDGE_LOOP('',(#21423,#21424,#21425,#21426));
#9133=EDGE_LOOP('',(#21427,#21428,#21429,#21430));
#9134=EDGE_LOOP('',(#21431,#21432,#21433,#21434));
#9135=EDGE_LOOP('',(#21435,#21436,#21437,#21438));
#9136=EDGE_LOOP('',(#21439,#21440,#21441,#21442));
#9137=EDGE_LOOP('',(#21443,#21444,#21445,#21446));
#9138=EDGE_LOOP('',(#21447,#21448,#21449,#21450));
#9139=EDGE_LOOP('',(#21451,#21452,#21453,#21454));
#9140=EDGE_LOOP('',(#21455,#21456,#21457,#21458));
#9141=EDGE_LOOP('',(#21459,#21460,#21461,#21462));
#9142=EDGE_LOOP('',(#21463,#21464,#21465,#21466));
#9143=EDGE_LOOP('',(#21467,#21468,#21469,#21470));
#9144=EDGE_LOOP('',(#21471,#21472,#21473,#21474));
#9145=EDGE_LOOP('',(#21475,#21476,#21477,#21478));
#9146=EDGE_LOOP('',(#21479,#21480,#21481,#21482));
#9147=EDGE_LOOP('',(#21483,#21484,#21485,#21486));
#9148=EDGE_LOOP('',(#21487,#21488,#21489,#21490));
#9149=EDGE_LOOP('',(#21491,#21492,#21493,#21494));
#9150=EDGE_LOOP('',(#21495,#21496,#21497,#21498));
#9151=EDGE_LOOP('',(#21499,#21500,#21501,#21502));
#9152=EDGE_LOOP('',(#21503,#21504,#21505,#21506));
#9153=EDGE_LOOP('',(#21507,#21508,#21509,#21510));
#9154=EDGE_LOOP('',(#21511,#21512,#21513,#21514));
#9155=EDGE_LOOP('',(#21515,#21516,#21517,#21518));
#9156=EDGE_LOOP('',(#21519,#21520,#21521,#21522));
#9157=EDGE_LOOP('',(#21523,#21524,#21525,#21526));
#9158=EDGE_LOOP('',(#21527,#21528,#21529,#21530));
#9159=EDGE_LOOP('',(#21531,#21532,#21533,#21534));
#9160=EDGE_LOOP('',(#21535,#21536,#21537,#21538,#21539,#21540,#21541,#21542,
#21543,#21544,#21545,#21546,#21547,#21548,#21549,#21550,#21551,#21552,#21553,
#21554,#21555,#21556,#21557,#21558,#21559,#21560,#21561,#21562,#21563,#21564,
#21565,#21566,#21567,#21568,#21569,#21570,#21571,#21572,#21573,#21574,#21575,
#21576,#21577,#21578,#21579,#21580,#21581,#21582,#21583,#21584,#21585,#21586,
#21587,#21588,#21589,#21590,#21591,#21592,#21593,#21594,#21595,#21596,#21597,
#21598,#21599,#21600,#21601,#21602,#21603,#21604,#21605,#21606,#21607,#21608,
#21609,#21610,#21611,#21612,#21613,#21614,#21615,#21616,#21617,#21618,#21619,
#21620,#21621,#21622,#21623,#21624,#21625,#21626,#21627,#21628,#21629,#21630,
#21631,#21632,#21633,#21634,#21635,#21636,#21637,#21638,#21639,#21640,#21641,
#21642,#21643,#21644,#21645,#21646,#21647,#21648,#21649,#21650,#21651,#21652,
#21653,#21654,#21655));
#9161=EDGE_LOOP('',(#21656,#21657,#21658,#21659,#21660,#21661,#21662,#21663));
#9162=EDGE_LOOP('',(#21664,#21665,#21666,#21667));
#9163=EDGE_LOOP('',(#21668,#21669,#21670,#21671));
#9164=EDGE_LOOP('',(#21672,#21673,#21674,#21675));
#9165=EDGE_LOOP('',(#21676,#21677,#21678,#21679));
#9166=EDGE_LOOP('',(#21680,#21681,#21682,#21683));
#9167=EDGE_LOOP('',(#21684,#21685,#21686,#21687));
#9168=EDGE_LOOP('',(#21688,#21689,#21690,#21691));
#9169=EDGE_LOOP('',(#21692,#21693,#21694,#21695));
#9170=EDGE_LOOP('',(#21696,#21697,#21698,#21699));
#9171=EDGE_LOOP('',(#21700,#21701,#21702,#21703));
#9172=EDGE_LOOP('',(#21704,#21705,#21706,#21707));
#9173=EDGE_LOOP('',(#21708,#21709,#21710,#21711));
#9174=EDGE_LOOP('',(#21712,#21713,#21714,#21715));
#9175=EDGE_LOOP('',(#21716,#21717,#21718,#21719));
#9176=EDGE_LOOP('',(#21720,#21721,#21722,#21723));
#9177=EDGE_LOOP('',(#21724,#21725,#21726,#21727));
#9178=EDGE_LOOP('',(#21728,#21729,#21730,#21731));
#9179=EDGE_LOOP('',(#21732,#21733,#21734,#21735));
#9180=EDGE_LOOP('',(#21736,#21737,#21738,#21739));
#9181=EDGE_LOOP('',(#21740,#21741,#21742,#21743));
#9182=EDGE_LOOP('',(#21744,#21745,#21746,#21747));
#9183=EDGE_LOOP('',(#21748,#21749,#21750,#21751));
#9184=EDGE_LOOP('',(#21752,#21753,#21754,#21755));
#9185=EDGE_LOOP('',(#21756,#21757,#21758,#21759));
#9186=EDGE_LOOP('',(#21760,#21761,#21762,#21763));
#9187=EDGE_LOOP('',(#21764,#21765,#21766,#21767));
#9188=EDGE_LOOP('',(#21768,#21769,#21770,#21771));
#9189=EDGE_LOOP('',(#21772,#21773,#21774,#21775));
#9190=EDGE_LOOP('',(#21776,#21777,#21778,#21779));
#9191=EDGE_LOOP('',(#21780,#21781,#21782,#21783));
#9192=EDGE_LOOP('',(#21784,#21785,#21786,#21787));
#9193=EDGE_LOOP('',(#21788,#21789,#21790,#21791));
#9194=EDGE_LOOP('',(#21792,#21793,#21794,#21795));
#9195=EDGE_LOOP('',(#21796,#21797,#21798,#21799));
#9196=EDGE_LOOP('',(#21800,#21801,#21802,#21803));
#9197=EDGE_LOOP('',(#21804,#21805,#21806,#21807));
#9198=EDGE_LOOP('',(#21808,#21809,#21810,#21811));
#9199=EDGE_LOOP('',(#21812,#21813,#21814,#21815));
#9200=EDGE_LOOP('',(#21816,#21817,#21818,#21819));
#9201=EDGE_LOOP('',(#21820,#21821,#21822,#21823));
#9202=EDGE_LOOP('',(#21824,#21825,#21826,#21827));
#9203=EDGE_LOOP('',(#21828,#21829,#21830,#21831));
#9204=EDGE_LOOP('',(#21832,#21833,#21834,#21835));
#9205=EDGE_LOOP('',(#21836,#21837,#21838,#21839));
#9206=EDGE_LOOP('',(#21840,#21841,#21842,#21843));
#9207=EDGE_LOOP('',(#21844,#21845,#21846,#21847));
#9208=EDGE_LOOP('',(#21848,#21849,#21850,#21851));
#9209=EDGE_LOOP('',(#21852,#21853,#21854,#21855));
#9210=EDGE_LOOP('',(#21856,#21857,#21858,#21859));
#9211=EDGE_LOOP('',(#21860,#21861,#21862,#21863));
#9212=EDGE_LOOP('',(#21864,#21865,#21866,#21867));
#9213=EDGE_LOOP('',(#21868,#21869,#21870,#21871));
#9214=EDGE_LOOP('',(#21872,#21873,#21874,#21875));
#9215=EDGE_LOOP('',(#21876,#21877,#21878,#21879));
#9216=EDGE_LOOP('',(#21880,#21881,#21882,#21883));
#9217=EDGE_LOOP('',(#21884,#21885,#21886,#21887));
#9218=EDGE_LOOP('',(#21888,#21889,#21890,#21891));
#9219=EDGE_LOOP('',(#21892,#21893,#21894,#21895));
#9220=EDGE_LOOP('',(#21896,#21897,#21898,#21899));
#9221=EDGE_LOOP('',(#21900,#21901,#21902,#21903));
#9222=EDGE_LOOP('',(#21904,#21905,#21906,#21907));
#9223=EDGE_LOOP('',(#21908,#21909,#21910,#21911));
#9224=EDGE_LOOP('',(#21912,#21913,#21914,#21915));
#9225=EDGE_LOOP('',(#21916,#21917,#21918,#21919));
#9226=EDGE_LOOP('',(#21920,#21921,#21922,#21923));
#9227=EDGE_LOOP('',(#21924,#21925,#21926,#21927));
#9228=EDGE_LOOP('',(#21928,#21929,#21930,#21931));
#9229=EDGE_LOOP('',(#21932,#21933,#21934,#21935));
#9230=EDGE_LOOP('',(#21936,#21937,#21938,#21939));
#9231=EDGE_LOOP('',(#21940,#21941,#21942,#21943));
#9232=EDGE_LOOP('',(#21944,#21945,#21946,#21947));
#9233=EDGE_LOOP('',(#21948,#21949,#21950,#21951));
#9234=EDGE_LOOP('',(#21952,#21953,#21954,#21955));
#9235=EDGE_LOOP('',(#21956,#21957,#21958,#21959));
#9236=EDGE_LOOP('',(#21960,#21961,#21962,#21963));
#9237=EDGE_LOOP('',(#21964,#21965,#21966,#21967));
#9238=EDGE_LOOP('',(#21968,#21969,#21970,#21971));
#9239=EDGE_LOOP('',(#21972,#21973,#21974,#21975));
#9240=EDGE_LOOP('',(#21976,#21977,#21978,#21979));
#9241=EDGE_LOOP('',(#21980,#21981,#21982,#21983));
#9242=EDGE_LOOP('',(#21984,#21985,#21986,#21987));
#9243=EDGE_LOOP('',(#21988,#21989,#21990,#21991));
#9244=EDGE_LOOP('',(#21992,#21993,#21994,#21995));
#9245=EDGE_LOOP('',(#21996,#21997,#21998,#21999));
#9246=EDGE_LOOP('',(#22000,#22001,#22002,#22003));
#9247=EDGE_LOOP('',(#22004,#22005,#22006,#22007));
#9248=EDGE_LOOP('',(#22008,#22009,#22010,#22011));
#9249=EDGE_LOOP('',(#22012,#22013,#22014,#22015));
#9250=EDGE_LOOP('',(#22016,#22017,#22018,#22019));
#9251=EDGE_LOOP('',(#22020,#22021,#22022,#22023));
#9252=EDGE_LOOP('',(#22024,#22025,#22026,#22027));
#9253=EDGE_LOOP('',(#22028,#22029,#22030,#22031));
#9254=EDGE_LOOP('',(#22032,#22033,#22034,#22035));
#9255=EDGE_LOOP('',(#22036,#22037,#22038,#22039));
#9256=EDGE_LOOP('',(#22040,#22041,#22042,#22043));
#9257=EDGE_LOOP('',(#22044,#22045,#22046,#22047));
#9258=EDGE_LOOP('',(#22048,#22049,#22050,#22051));
#9259=EDGE_LOOP('',(#22052,#22053,#22054,#22055));
#9260=EDGE_LOOP('',(#22056,#22057,#22058,#22059));
#9261=EDGE_LOOP('',(#22060,#22061,#22062,#22063));
#9262=EDGE_LOOP('',(#22064,#22065,#22066,#22067));
#9263=EDGE_LOOP('',(#22068,#22069,#22070,#22071));
#9264=EDGE_LOOP('',(#22072,#22073,#22074,#22075));
#9265=EDGE_LOOP('',(#22076,#22077,#22078,#22079));
#9266=EDGE_LOOP('',(#22080,#22081,#22082,#22083));
#9267=EDGE_LOOP('',(#22084,#22085,#22086,#22087));
#9268=EDGE_LOOP('',(#22088,#22089,#22090,#22091));
#9269=EDGE_LOOP('',(#22092,#22093,#22094,#22095));
#9270=EDGE_LOOP('',(#22096,#22097,#22098,#22099));
#9271=EDGE_LOOP('',(#22100,#22101,#22102,#22103));
#9272=EDGE_LOOP('',(#22104,#22105,#22106,#22107));
#9273=EDGE_LOOP('',(#22108,#22109,#22110,#22111));
#9274=EDGE_LOOP('',(#22112,#22113,#22114,#22115));
#9275=EDGE_LOOP('',(#22116,#22117,#22118,#22119));
#9276=EDGE_LOOP('',(#22120,#22121,#22122,#22123));
#9277=EDGE_LOOP('',(#22124,#22125,#22126,#22127));
#9278=EDGE_LOOP('',(#22128,#22129,#22130,#22131));
#9279=EDGE_LOOP('',(#22132,#22133,#22134,#22135));
#9280=EDGE_LOOP('',(#22136,#22137,#22138,#22139));
#9281=EDGE_LOOP('',(#22140,#22141,#22142,#22143));
#9282=EDGE_LOOP('',(#22144,#22145,#22146,#22147,#22148,#22149,#22150,#22151));
#9283=EDGE_LOOP('',(#22152,#22153,#22154,#22155));
#9284=EDGE_LOOP('',(#22156,#22157,#22158,#22159));
#9285=EDGE_LOOP('',(#22160,#22161,#22162,#22163));
#9286=EDGE_LOOP('',(#22164,#22165,#22166,#22167));
#9287=EDGE_LOOP('',(#22168,#22169,#22170,#22171));
#9288=EDGE_LOOP('',(#22172,#22173,#22174,#22175));
#9289=EDGE_LOOP('',(#22176,#22177,#22178,#22179));
#9290=EDGE_LOOP('',(#22180,#22181,#22182,#22183));
#9291=EDGE_LOOP('',(#22184,#22185,#22186,#22187));
#9292=EDGE_LOOP('',(#22188,#22189,#22190,#22191));
#9293=EDGE_LOOP('',(#22192,#22193,#22194,#22195));
#9294=EDGE_LOOP('',(#22196,#22197,#22198,#22199));
#9295=EDGE_LOOP('',(#22200,#22201,#22202,#22203));
#9296=EDGE_LOOP('',(#22204,#22205,#22206,#22207));
#9297=EDGE_LOOP('',(#22208,#22209,#22210,#22211));
#9298=EDGE_LOOP('',(#22212,#22213,#22214,#22215));
#9299=EDGE_LOOP('',(#22216,#22217,#22218,#22219));
#9300=EDGE_LOOP('',(#22220,#22221,#22222,#22223));
#9301=EDGE_LOOP('',(#22224,#22225,#22226,#22227));
#9302=EDGE_LOOP('',(#22228,#22229,#22230,#22231));
#9303=EDGE_LOOP('',(#22232,#22233,#22234,#22235));
#9304=EDGE_LOOP('',(#22236,#22237,#22238,#22239));
#9305=EDGE_LOOP('',(#22240,#22241,#22242,#22243));
#9306=EDGE_LOOP('',(#22244,#22245,#22246,#22247));
#9307=EDGE_LOOP('',(#22248,#22249,#22250,#22251));
#9308=EDGE_LOOP('',(#22252,#22253,#22254,#22255));
#9309=EDGE_LOOP('',(#22256,#22257,#22258,#22259));
#9310=EDGE_LOOP('',(#22260,#22261,#22262,#22263));
#9311=EDGE_LOOP('',(#22264,#22265,#22266,#22267));
#9312=EDGE_LOOP('',(#22268,#22269,#22270,#22271));
#9313=EDGE_LOOP('',(#22272,#22273,#22274,#22275));
#9314=EDGE_LOOP('',(#22276,#22277,#22278,#22279));
#9315=EDGE_LOOP('',(#22280,#22281,#22282,#22283));
#9316=EDGE_LOOP('',(#22284,#22285,#22286,#22287));
#9317=EDGE_LOOP('',(#22288,#22289,#22290,#22291));
#9318=EDGE_LOOP('',(#22292,#22293,#22294,#22295));
#9319=EDGE_LOOP('',(#22296,#22297,#22298,#22299));
#9320=EDGE_LOOP('',(#22300,#22301,#22302,#22303));
#9321=EDGE_LOOP('',(#22304,#22305,#22306,#22307));
#9322=EDGE_LOOP('',(#22308,#22309,#22310,#22311));
#9323=EDGE_LOOP('',(#22312,#22313,#22314,#22315));
#9324=EDGE_LOOP('',(#22316,#22317,#22318,#22319));
#9325=EDGE_LOOP('',(#22320,#22321,#22322,#22323));
#9326=EDGE_LOOP('',(#22324,#22325,#22326,#22327));
#9327=EDGE_LOOP('',(#22328,#22329,#22330,#22331));
#9328=EDGE_LOOP('',(#22332,#22333,#22334,#22335));
#9329=EDGE_LOOP('',(#22336,#22337,#22338,#22339));
#9330=EDGE_LOOP('',(#22340,#22341,#22342,#22343));
#9331=EDGE_LOOP('',(#22344,#22345,#22346,#22347));
#9332=EDGE_LOOP('',(#22348,#22349,#22350,#22351));
#9333=EDGE_LOOP('',(#22352,#22353,#22354,#22355));
#9334=EDGE_LOOP('',(#22356,#22357,#22358,#22359));
#9335=EDGE_LOOP('',(#22360,#22361,#22362,#22363));
#9336=EDGE_LOOP('',(#22364,#22365,#22366,#22367));
#9337=EDGE_LOOP('',(#22368,#22369,#22370,#22371));
#9338=EDGE_LOOP('',(#22372,#22373,#22374,#22375));
#9339=EDGE_LOOP('',(#22376,#22377,#22378,#22379));
#9340=EDGE_LOOP('',(#22380,#22381,#22382,#22383));
#9341=EDGE_LOOP('',(#22384,#22385,#22386,#22387));
#9342=EDGE_LOOP('',(#22388,#22389,#22390,#22391));
#9343=EDGE_LOOP('',(#22392,#22393,#22394,#22395));
#9344=EDGE_LOOP('',(#22396,#22397,#22398,#22399));
#9345=EDGE_LOOP('',(#22400,#22401,#22402,#22403));
#9346=EDGE_LOOP('',(#22404,#22405,#22406,#22407));
#9347=EDGE_LOOP('',(#22408,#22409,#22410,#22411));
#9348=EDGE_LOOP('',(#22412,#22413,#22414,#22415));
#9349=EDGE_LOOP('',(#22416,#22417,#22418,#22419));
#9350=EDGE_LOOP('',(#22420,#22421,#22422,#22423));
#9351=EDGE_LOOP('',(#22424,#22425,#22426,#22427));
#9352=EDGE_LOOP('',(#22428,#22429,#22430,#22431));
#9353=EDGE_LOOP('',(#22432,#22433,#22434,#22435));
#9354=EDGE_LOOP('',(#22436,#22437,#22438,#22439));
#9355=EDGE_LOOP('',(#22440,#22441,#22442,#22443));
#9356=EDGE_LOOP('',(#22444,#22445,#22446,#22447));
#9357=EDGE_LOOP('',(#22448,#22449,#22450,#22451));
#9358=EDGE_LOOP('',(#22452,#22453,#22454,#22455));
#9359=EDGE_LOOP('',(#22456,#22457,#22458,#22459));
#9360=EDGE_LOOP('',(#22460,#22461,#22462,#22463));
#9361=EDGE_LOOP('',(#22464,#22465,#22466,#22467));
#9362=EDGE_LOOP('',(#22468,#22469,#22470,#22471));
#9363=EDGE_LOOP('',(#22472,#22473,#22474,#22475));
#9364=EDGE_LOOP('',(#22476,#22477,#22478,#22479));
#9365=EDGE_LOOP('',(#22480,#22481,#22482,#22483));
#9366=EDGE_LOOP('',(#22484,#22485,#22486,#22487));
#9367=EDGE_LOOP('',(#22488,#22489,#22490,#22491));
#9368=EDGE_LOOP('',(#22492,#22493,#22494,#22495));
#9369=EDGE_LOOP('',(#22496,#22497,#22498,#22499));
#9370=EDGE_LOOP('',(#22500,#22501,#22502,#22503));
#9371=EDGE_LOOP('',(#22504,#22505,#22506,#22507));
#9372=EDGE_LOOP('',(#22508,#22509,#22510,#22511));
#9373=EDGE_LOOP('',(#22512,#22513,#22514,#22515));
#9374=EDGE_LOOP('',(#22516,#22517,#22518,#22519));
#9375=EDGE_LOOP('',(#22520,#22521,#22522,#22523));
#9376=EDGE_LOOP('',(#22524,#22525,#22526,#22527));
#9377=EDGE_LOOP('',(#22528,#22529,#22530,#22531));
#9378=EDGE_LOOP('',(#22532,#22533,#22534,#22535));
#9379=EDGE_LOOP('',(#22536,#22537,#22538,#22539));
#9380=EDGE_LOOP('',(#22540,#22541,#22542,#22543));
#9381=EDGE_LOOP('',(#22544,#22545,#22546,#22547));
#9382=EDGE_LOOP('',(#22548,#22549,#22550,#22551));
#9383=EDGE_LOOP('',(#22552,#22553,#22554,#22555));
#9384=EDGE_LOOP('',(#22556,#22557,#22558,#22559));
#9385=EDGE_LOOP('',(#22560,#22561,#22562,#22563));
#9386=EDGE_LOOP('',(#22564,#22565,#22566,#22567));
#9387=EDGE_LOOP('',(#22568,#22569,#22570,#22571));
#9388=EDGE_LOOP('',(#22572,#22573,#22574,#22575));
#9389=EDGE_LOOP('',(#22576,#22577,#22578,#22579));
#9390=EDGE_LOOP('',(#22580,#22581,#22582,#22583));
#9391=EDGE_LOOP('',(#22584,#22585,#22586,#22587));
#9392=EDGE_LOOP('',(#22588,#22589,#22590,#22591));
#9393=EDGE_LOOP('',(#22592,#22593,#22594,#22595));
#9394=EDGE_LOOP('',(#22596,#22597,#22598,#22599));
#9395=EDGE_LOOP('',(#22600,#22601,#22602,#22603));
#9396=EDGE_LOOP('',(#22604,#22605,#22606,#22607));
#9397=EDGE_LOOP('',(#22608,#22609,#22610,#22611));
#9398=EDGE_LOOP('',(#22612,#22613,#22614,#22615));
#9399=EDGE_LOOP('',(#22616,#22617,#22618,#22619));
#9400=EDGE_LOOP('',(#22620,#22621,#22622,#22623));
#9401=EDGE_LOOP('',(#22624,#22625,#22626,#22627));
#9402=EDGE_LOOP('',(#22628,#22629,#22630,#22631));
#9403=EDGE_LOOP('',(#22632,#22633,#22634,#22635));
#9404=EDGE_LOOP('',(#22636,#22637,#22638,#22639));
#9405=EDGE_LOOP('',(#22640,#22641,#22642,#22643));
#9406=EDGE_LOOP('',(#22644,#22645,#22646,#22647));
#9407=EDGE_LOOP('',(#22648,#22649,#22650,#22651));
#9408=EDGE_LOOP('',(#22652,#22653,#22654,#22655));
#9409=EDGE_LOOP('',(#22656,#22657,#22658,#22659));
#9410=EDGE_LOOP('',(#22660,#22661,#22662,#22663));
#9411=EDGE_LOOP('',(#22664,#22665,#22666,#22667));
#9412=EDGE_LOOP('',(#22668,#22669,#22670,#22671));
#9413=EDGE_LOOP('',(#22672,#22673,#22674,#22675));
#9414=EDGE_LOOP('',(#22676,#22677,#22678,#22679));
#9415=EDGE_LOOP('',(#22680,#22681,#22682,#22683));
#9416=EDGE_LOOP('',(#22684,#22685,#22686,#22687));
#9417=EDGE_LOOP('',(#22688,#22689,#22690,#22691));
#9418=EDGE_LOOP('',(#22692,#22693,#22694,#22695));
#9419=EDGE_LOOP('',(#22696,#22697,#22698,#22699));
#9420=EDGE_LOOP('',(#22700,#22701,#22702,#22703));
#9421=EDGE_LOOP('',(#22704,#22705,#22706,#22707));
#9422=EDGE_LOOP('',(#22708,#22709,#22710,#22711));
#9423=EDGE_LOOP('',(#22712,#22713,#22714,#22715));
#9424=EDGE_LOOP('',(#22716,#22717,#22718,#22719));
#9425=EDGE_LOOP('',(#22720,#22721,#22722,#22723));
#9426=EDGE_LOOP('',(#22724,#22725,#22726,#22727));
#9427=EDGE_LOOP('',(#22728,#22729,#22730,#22731));
#9428=EDGE_LOOP('',(#22732,#22733,#22734,#22735));
#9429=EDGE_LOOP('',(#22736,#22737,#22738,#22739));
#9430=EDGE_LOOP('',(#22740,#22741,#22742,#22743));
#9431=EDGE_LOOP('',(#22744,#22745,#22746,#22747));
#9432=EDGE_LOOP('',(#22748,#22749,#22750,#22751));
#9433=EDGE_LOOP('',(#22752,#22753,#22754,#22755));
#9434=EDGE_LOOP('',(#22756,#22757,#22758,#22759));
#9435=EDGE_LOOP('',(#22760,#22761,#22762,#22763));
#9436=EDGE_LOOP('',(#22764,#22765,#22766,#22767));
#9437=EDGE_LOOP('',(#22768,#22769,#22770,#22771));
#9438=EDGE_LOOP('',(#22772,#22773,#22774,#22775));
#9439=EDGE_LOOP('',(#22776,#22777,#22778,#22779,#22780,#22781,#22782,#22783));
#9440=EDGE_LOOP('',(#22784,#22785,#22786,#22787));
#9441=EDGE_LOOP('',(#22788,#22789,#22790,#22791));
#9442=EDGE_LOOP('',(#22792,#22793,#22794,#22795));
#9443=EDGE_LOOP('',(#22796,#22797,#22798,#22799));
#9444=EDGE_LOOP('',(#22800,#22801,#22802,#22803));
#9445=EDGE_LOOP('',(#22804,#22805,#22806,#22807,#22808,#22809,#22810));
#9446=EDGE_LOOP('',(#22811));
#9447=EDGE_LOOP('',(#22812,#22813,#22814,#22815));
#9448=EDGE_LOOP('',(#22816,#22817,#22818,#22819,#22820,#22821,#22822,#22823,
#22824));
#9449=EDGE_LOOP('',(#22825,#22826));
#9450=EDGE_LOOP('',(#22827,#22828,#22829,#22830));
#9451=EDGE_LOOP('',(#22831,#22832,#22833,#22834));
#9452=EDGE_LOOP('',(#22835));
#9453=EDGE_LOOP('',(#22836));
#9454=EDGE_LOOP('',(#22837,#22838,#22839,#22840));
#9455=EDGE_LOOP('',(#22841));
#9456=EDGE_LOOP('',(#22842));
#9457=EDGE_LOOP('',(#22843,#22844,#22845,#22846));
#9458=EDGE_LOOP('',(#22847));
#9459=EDGE_LOOP('',(#22848));
#9460=EDGE_LOOP('',(#22849,#22850,#22851,#22852));
#9461=EDGE_LOOP('',(#22853));
#9462=EDGE_LOOP('',(#22854));
#9463=EDGE_LOOP('',(#22855,#22856,#22857,#22858));
#9464=EDGE_LOOP('',(#22859));
#9465=EDGE_LOOP('',(#22860));
#9466=EDGE_LOOP('',(#22861,#22862,#22863,#22864));
#9467=EDGE_LOOP('',(#22865,#22866,#22867,#22868));
#9468=EDGE_LOOP('',(#22869,#22870,#22871,#22872));
#9469=EDGE_LOOP('',(#22873));
#9470=EDGE_LOOP('',(#22874,#22875,#22876,#22877));
#9471=EDGE_LOOP('',(#22878));
#9472=EDGE_LOOP('',(#22879));
#9473=EDGE_LOOP('',(#22880,#22881,#22882,#22883));
#9474=EDGE_LOOP('',(#22884));
#9475=EDGE_LOOP('',(#22885));
#9476=EDGE_LOOP('',(#22886,#22887,#22888,#22889));
#9477=EDGE_LOOP('',(#22890,#22891,#22892,#22893));
#9478=EDGE_LOOP('',(#22894,#22895,#22896,#22897));
#9479=EDGE_LOOP('',(#22898));
#9480=EDGE_LOOP('',(#22899));
#9481=EDGE_LOOP('',(#22900,#22901,#22902,#22903));
#9482=EDGE_LOOP('',(#22904));
#9483=EDGE_LOOP('',(#22905));
#9484=EDGE_LOOP('',(#22906,#22907,#22908,#22909));
#9485=EDGE_LOOP('',(#22910));
#9486=EDGE_LOOP('',(#22911));
#9487=EDGE_LOOP('',(#22912,#22913,#22914,#22915));
#9488=EDGE_LOOP('',(#22916,#22917,#22918,#22919));
#9489=EDGE_LOOP('',(#22920,#22921,#22922,#22923));
#9490=EDGE_LOOP('',(#22924));
#9491=EDGE_LOOP('',(#22925));
#9492=EDGE_LOOP('',(#22926,#22927,#22928,#22929,#22930));
#9493=EDGE_LOOP('',(#22931,#22932,#22933,#22934,#22935));
#9494=EDGE_LOOP('',(#22936));
#9495=EDGE_LOOP('',(#22937));
#9496=EDGE_LOOP('',(#22938,#22939,#22940,#22941));
#9497=EDGE_LOOP('',(#22942));
#9498=EDGE_LOOP('',(#22943));
#9499=EDGE_LOOP('',(#22944,#22945,#22946,#22947));
#9500=EDGE_LOOP('',(#22948,#22949,#22950,#22951));
#9501=EDGE_LOOP('',(#22952));
#9502=EDGE_LOOP('',(#22953));
#9503=EDGE_LOOP('',(#22954,#22955,#22956,#22957));
#9504=EDGE_LOOP('',(#22958));
#9505=EDGE_LOOP('',(#22959));
#9506=EDGE_LOOP('',(#22960,#22961,#22962,#22963));
#9507=EDGE_LOOP('',(#22964));
#9508=EDGE_LOOP('',(#22965));
#9509=EDGE_LOOP('',(#22966,#22967,#22968,#22969));
#9510=EDGE_LOOP('',(#22970,#22971,#22972,#22973));
#9511=EDGE_LOOP('',(#22974));
#9512=EDGE_LOOP('',(#22975));
#9513=EDGE_LOOP('',(#22976));
#9514=EDGE_LOOP('',(#22977,#22978,#22979,#22980));
#9515=EDGE_LOOP('',(#22981,#22982,#22983,#22984));
#9516=EDGE_LOOP('',(#22985,#22986,#22987,#22988));
#9517=EDGE_LOOP('',(#22989));
#9518=EDGE_LOOP('',(#22990,#22991,#22992,#22993));
#9519=EDGE_LOOP('',(#22994));
#9520=EDGE_LOOP('',(#22995));
#9521=EDGE_LOOP('',(#22996,#22997,#22998,#22999));
#9522=EDGE_LOOP('',(#23000));
#9523=EDGE_LOOP('',(#23001));
#9524=EDGE_LOOP('',(#23002,#23003,#23004,#23005));
#9525=EDGE_LOOP('',(#23006,#23007,#23008,#23009));
#9526=EDGE_LOOP('',(#23010,#23011,#23012,#23013));
#9527=EDGE_LOOP('',(#23014,#23015,#23016,#23017));
#9528=EDGE_LOOP('',(#23018,#23019,#23020,#23021));
#9529=EDGE_LOOP('',(#23022,#23023,#23024,#23025));
#9530=EDGE_LOOP('',(#23026,#23027,#23028,#23029));
#9531=EDGE_LOOP('',(#23030,#23031,#23032,#23033));
#9532=EDGE_LOOP('',(#23034,#23035,#23036,#23037));
#9533=EDGE_LOOP('',(#23038,#23039,#23040,#23041));
#9534=EDGE_LOOP('',(#23042,#23043,#23044,#23045));
#9535=EDGE_LOOP('',(#23046,#23047,#23048,#23049,#23050,#23051,#23052,#23053));
#9536=EDGE_LOOP('',(#23054,#23055,#23056,#23057));
#9537=EDGE_LOOP('',(#23058,#23059,#23060));
#9538=EDGE_LOOP('',(#23061,#23062,#23063));
#9539=EDGE_LOOP('',(#23064,#23065,#23066,#23067));
#9540=EDGE_LOOP('',(#23068,#23069,#23070));
#9541=EDGE_LOOP('',(#23071,#23072,#23073));
#9542=EDGE_LOOP('',(#23074,#23075,#23076,#23077));
#9543=EDGE_LOOP('',(#23078,#23079,#23080,#23081));
#9544=EDGE_LOOP('',(#23082,#23083,#23084,#23085));
#9545=EDGE_LOOP('',(#23086,#23087,#23088,#23089));
#9546=EDGE_LOOP('',(#23090,#23091,#23092,#23093));
#9547=EDGE_LOOP('',(#23094,#23095,#23096,#23097));
#9548=EDGE_LOOP('',(#23098,#23099,#23100,#23101));
#9549=EDGE_LOOP('',(#23102,#23103,#23104,#23105));
#9550=EDGE_LOOP('',(#23106,#23107,#23108,#23109));
#9551=EDGE_LOOP('',(#23110,#23111,#23112,#23113));
#9552=EDGE_LOOP('',(#23114,#23115,#23116,#23117,#23118,#23119,#23120,#23121));
#9553=EDGE_LOOP('',(#23122,#23123,#23124,#23125));
#9554=EDGE_LOOP('',(#23126,#23127,#23128,#23129));
#9555=EDGE_LOOP('',(#23130,#23131,#23132,#23133));
#9556=EDGE_LOOP('',(#23134,#23135,#23136,#23137,#23138,#23139,#23140,#23141,
#23142,#23143));
#9557=EDGE_LOOP('',(#23144));
#9558=EDGE_LOOP('',(#23145,#23146,#23147));
#9559=EDGE_LOOP('',(#23148,#23149,#23150));
#9560=EDGE_LOOP('',(#23151,#23152,#23153));
#9561=EDGE_LOOP('',(#23154,#23155,#23156));
#9562=EDGE_LOOP('',(#23157,#23158,#23159));
#9563=EDGE_LOOP('',(#23160,#23161,#23162));
#9564=EDGE_LOOP('',(#23163,#23164,#23165,#23166));
#9565=EDGE_LOOP('',(#23167,#23168,#23169,#23170));
#9566=EDGE_LOOP('',(#23171,#23172,#23173,#23174));
#9567=EDGE_LOOP('',(#23175,#23176,#23177,#23178));
#9568=EDGE_LOOP('',(#23179,#23180,#23181,#23182));
#9569=EDGE_LOOP('',(#23183,#23184,#23185,#23186));
#9570=EDGE_LOOP('',(#23187,#23188,#23189,#23190));
#9571=EDGE_LOOP('',(#23191,#23192,#23193,#23194,#23195));
#9572=EDGE_LOOP('',(#23196,#23197,#23198,#23199));
#9573=EDGE_LOOP('',(#23200,#23201,#23202,#23203));
#9574=EDGE_LOOP('',(#23204,#23205,#23206,#23207));
#9575=EDGE_LOOP('',(#23208,#23209,#23210,#23211));
#9576=EDGE_LOOP('',(#23212,#23213,#23214,#23215));
#9577=EDGE_LOOP('',(#23216,#23217,#23218,#23219,#23220,#23221));
#9578=EDGE_LOOP('',(#23222,#23223,#23224,#23225));
#9579=EDGE_LOOP('',(#23226,#23227,#23228,#23229,#23230,#23231));
#9580=EDGE_LOOP('',(#23232,#23233,#23234,#23235));
#9581=EDGE_LOOP('',(#23236,#23237,#23238,#23239,#23240,#23241));
#9582=EDGE_LOOP('',(#23242,#23243,#23244,#23245,#23246,#23247));
#9583=EDGE_LOOP('',(#23248,#23249,#23250,#23251,#23252,#23253));
#9584=EDGE_LOOP('',(#23254,#23255,#23256,#23257));
#9585=EDGE_LOOP('',(#23258,#23259,#23260,#23261));
#9586=EDGE_LOOP('',(#23262,#23263,#23264,#23265));
#9587=EDGE_LOOP('',(#23266,#23267,#23268,#23269,#23270,#23271));
#9588=EDGE_LOOP('',(#23272,#23273));
#9589=EDGE_LOOP('',(#23274,#23275));
#9590=EDGE_LOOP('',(#23276,#23277));
#9591=EDGE_LOOP('',(#23278,#23279));
#9592=EDGE_LOOP('',(#23280,#23281));
#9593=EDGE_LOOP('',(#23282,#23283,#23284));
#9594=EDGE_LOOP('',(#23285));
#9595=EDGE_LOOP('',(#23286,#23287,#23288,#23289));
#9596=EDGE_LOOP('',(#23290,#23291,#23292,#23293,#23294,#23295,#23296,#23297,
#23298,#23299,#23300,#23301,#23302,#23303,#23304,#23305));
#9597=EDGE_LOOP('',(#23306,#23307,#23308,#23309));
#9598=EDGE_LOOP('',(#23310,#23311,#23312,#23313));
#9599=EDGE_LOOP('',(#23314,#23315,#23316,#23317));
#9600=EDGE_LOOP('',(#23318,#23319,#23320,#23321));
#9601=EDGE_LOOP('',(#23322,#23323,#23324,#23325));
#9602=EDGE_LOOP('',(#23326,#23327,#23328,#23329));
#9603=EDGE_LOOP('',(#23330,#23331,#23332,#23333));
#9604=EDGE_LOOP('',(#23334,#23335,#23336,#23337));
#9605=EDGE_LOOP('',(#23338,#23339,#23340,#23341));
#9606=EDGE_LOOP('',(#23342,#23343,#23344,#23345));
#9607=EDGE_LOOP('',(#23346,#23347,#23348,#23349));
#9608=EDGE_LOOP('',(#23350,#23351,#23352,#23353));
#9609=EDGE_LOOP('',(#23354,#23355,#23356,#23357,#23358,#23359,#23360,#23361));
#9610=EDGE_LOOP('',(#23362));
#9611=EDGE_LOOP('',(#23363));
#9612=EDGE_LOOP('',(#23364));
#9613=EDGE_LOOP('',(#23365));
#9614=EDGE_LOOP('',(#23366,#23367,#23368,#23369,#23370,#23371,#23372,#23373));
#9615=EDGE_LOOP('',(#23374,#23375,#23376,#23377));
#9616=EDGE_LOOP('',(#23378,#23379,#23380,#23381));
#9617=EDGE_LOOP('',(#23382,#23383,#23384,#23385));
#9618=EDGE_LOOP('',(#23386,#23387,#23388,#23389));
#9619=EDGE_LOOP('',(#23390,#23391,#23392,#23393));
#9620=EDGE_LOOP('',(#23394,#23395,#23396,#23397));
#9621=EDGE_LOOP('',(#23398,#23399,#23400,#23401));
#9622=EDGE_LOOP('',(#23402,#23403,#23404,#23405));
#9623=EDGE_LOOP('',(#23406,#23407,#23408,#23409));
#9624=EDGE_LOOP('',(#23410,#23411,#23412,#23413));
#9625=EDGE_LOOP('',(#23414,#23415,#23416,#23417));
#9626=EDGE_LOOP('',(#23418,#23419,#23420,#23421,#23422,#23423,#23424,#23425));
#9627=EDGE_LOOP('',(#23426));
#9628=EDGE_LOOP('',(#23427));
#9629=EDGE_LOOP('',(#23428));
#9630=EDGE_LOOP('',(#23429));
#9631=EDGE_LOOP('',(#23430,#23431,#23432,#23433));
#9632=EDGE_LOOP('',(#23434,#23435,#23436,#23437));
#9633=EDGE_LOOP('',(#23438,#23439,#23440,#23441));
#9634=EDGE_LOOP('',(#23442,#23443,#23444,#23445));
#9635=EDGE_LOOP('',(#23446,#23447,#23448,#23449));
#9636=EDGE_LOOP('',(#23450,#23451,#23452,#23453));
#9637=EDGE_LOOP('',(#23454,#23455,#23456,#23457));
#9638=EDGE_LOOP('',(#23458,#23459,#23460,#23461));
#9639=EDGE_LOOP('',(#23462,#23463,#23464,#23465));
#9640=EDGE_LOOP('',(#23466,#23467,#23468,#23469));
#9641=EDGE_LOOP('',(#23470,#23471,#23472,#23473));
#9642=EDGE_LOOP('',(#23474,#23475,#23476,#23477));
#9643=EDGE_LOOP('',(#23478,#23479,#23480,#23481,#23482,#23483,#23484,#23485));
#9644=EDGE_LOOP('',(#23486,#23487,#23488,#23489));
#9645=EDGE_LOOP('',(#23490,#23491,#23492,#23493));
#9646=EDGE_LOOP('',(#23494,#23495,#23496,#23497));
#9647=EDGE_LOOP('',(#23498,#23499,#23500,#23501));
#9648=EDGE_LOOP('',(#23502,#23503,#23504,#23505));
#9649=EDGE_LOOP('',(#23506,#23507,#23508,#23509));
#9650=EDGE_LOOP('',(#23510,#23511,#23512,#23513));
#9651=EDGE_LOOP('',(#23514,#23515,#23516,#23517));
#9652=EDGE_LOOP('',(#23518,#23519,#23520,#23521));
#9653=EDGE_LOOP('',(#23522,#23523,#23524,#23525,#23526));
#9654=EDGE_LOOP('',(#23527,#23528,#23529,#23530,#23531,#23532,#23533,#23534,
#23535,#23536,#23537,#23538,#23539,#23540,#23541,#23542,#23543,#23544,#23545,
#23546,#23547,#23548,#23549,#23550,#23551,#23552,#23553));
#9655=EDGE_LOOP('',(#23554,#23555,#23556,#23557,#23558));
#9656=EDGE_LOOP('',(#23559,#23560,#23561,#23562,#23563,#23564));
#9657=EDGE_LOOP('',(#23565));
#9658=EDGE_LOOP('',(#23566));
#9659=EDGE_LOOP('',(#23567,#23568,#23569,#23570));
#9660=EDGE_LOOP('',(#23571,#23572,#23573,#23574));
#9661=EDGE_LOOP('',(#23575,#23576,#23577));
#9662=EDGE_LOOP('',(#23578,#23579,#23580,#23581));
#9663=EDGE_LOOP('',(#23582,#23583,#23584));
#9664=EDGE_LOOP('',(#23585,#23586,#23587));
#9665=EDGE_LOOP('',(#23588,#23589,#23590,#23591));
#9666=EDGE_LOOP('',(#23592,#23593,#23594,#23595));
#9667=EDGE_LOOP('',(#23596,#23597,#23598));
#9668=EDGE_LOOP('',(#23599,#23600,#23601,#23602));
#9669=EDGE_LOOP('',(#23603,#23604,#23605));
#9670=EDGE_LOOP('',(#23606,#23607,#23608));
#9671=EDGE_LOOP('',(#23609,#23610,#23611,#23612));
#9672=EDGE_LOOP('',(#23613,#23614,#23615,#23616));
#9673=EDGE_LOOP('',(#23617,#23618,#23619,#23620));
#9674=EDGE_LOOP('',(#23621,#23622,#23623,#23624));
#9675=EDGE_LOOP('',(#23625,#23626,#23627,#23628));
#9676=EDGE_LOOP('',(#23629,#23630,#23631,#23632));
#9677=EDGE_LOOP('',(#23633,#23634,#23635,#23636));
#9678=EDGE_LOOP('',(#23637,#23638,#23639,#23640,#23641,#23642,#23643,#23644));
#9679=EDGE_LOOP('',(#23645,#23646,#23647,#23648));
#9680=EDGE_LOOP('',(#23649,#23650,#23651,#23652));
#9681=EDGE_LOOP('',(#23653,#23654,#23655,#23656));
#9682=EDGE_LOOP('',(#23657,#23658,#23659,#23660,#23661,#23662));
#9683=EDGE_LOOP('',(#23663,#23664,#23665,#23666,#23667,#23668));
#9684=EDGE_LOOP('',(#23669));
#9685=EDGE_LOOP('',(#23670,#23671,#23672,#23673,#23674,#23675));
#9686=EDGE_LOOP('',(#23676,#23677,#23678));
#9687=EDGE_LOOP('',(#23679,#23680,#23681,#23682));
#9688=EDGE_LOOP('',(#23683,#23684,#23685,#23686,#23687));
#9689=EDGE_LOOP('',(#23688,#23689,#23690,#23691,#23692));
#9690=EDGE_LOOP('',(#23693,#23694,#23695,#23696,#23697,#23698,#23699,#23700));
#9691=EDGE_LOOP('',(#23701,#23702,#23703,#23704));
#9692=EDGE_LOOP('',(#23705,#23706,#23707,#23708,#23709));
#9693=EDGE_LOOP('',(#23710,#23711,#23712));
#9694=EDGE_LOOP('',(#23713,#23714,#23715));
#9695=EDGE_LOOP('',(#23716,#23717,#23718,#23719,#23720));
#9696=EDGE_LOOP('',(#23721,#23722,#23723,#23724));
#9697=EDGE_LOOP('',(#23725,#23726,#23727,#23728));
#9698=EDGE_LOOP('',(#23729,#23730,#23731,#23732,#23733));
#9699=EDGE_LOOP('',(#23734,#23735,#23736,#23737,#23738));
#9700=EDGE_LOOP('',(#23739,#23740,#23741,#23742,#23743));
#9701=EDGE_LOOP('',(#23744,#23745,#23746,#23747,#23748,#23749,#23750,#23751));
#9702=EDGE_LOOP('',(#23752,#23753,#23754,#23755));
#9703=EDGE_LOOP('',(#23756,#23757,#23758,#23759));
#9704=EDGE_LOOP('',(#23760,#23761,#23762));
#9705=EDGE_LOOP('',(#23763,#23764,#23765,#23766));
#9706=EDGE_LOOP('',(#23767,#23768,#23769));
#9707=EDGE_LOOP('',(#23770,#23771,#23772));
#9708=EDGE_LOOP('',(#23773,#23774,#23775,#23776));
#9709=EDGE_LOOP('',(#23777,#23778,#23779,#23780));
#9710=EDGE_LOOP('',(#23781,#23782,#23783));
#9711=EDGE_LOOP('',(#23784,#23785,#23786,#23787));
#9712=EDGE_LOOP('',(#23788,#23789,#23790));
#9713=EDGE_LOOP('',(#23791,#23792,#23793));
#9714=EDGE_LOOP('',(#23794,#23795,#23796,#23797));
#9715=EDGE_LOOP('',(#23798,#23799,#23800,#23801));
#9716=EDGE_LOOP('',(#23802,#23803,#23804,#23805));
#9717=EDGE_LOOP('',(#23806,#23807,#23808,#23809));
#9718=EDGE_LOOP('',(#23810,#23811,#23812,#23813));
#9719=EDGE_LOOP('',(#23814,#23815,#23816,#23817));
#9720=EDGE_LOOP('',(#23818,#23819,#23820,#23821));
#9721=EDGE_LOOP('',(#23822,#23823,#23824,#23825,#23826,#23827,#23828,#23829));
#9722=EDGE_LOOP('',(#23830,#23831,#23832,#23833));
#9723=EDGE_LOOP('',(#23834,#23835,#23836,#23837));
#9724=EDGE_LOOP('',(#23838,#23839,#23840,#23841));
#9725=EDGE_LOOP('',(#23842,#23843,#23844,#23845));
#9726=EDGE_LOOP('',(#23846,#23847,#23848,#23849,#23850));
#9727=EDGE_LOOP('',(#23851,#23852));
#9728=EDGE_LOOP('',(#23853,#23854));
#9729=EDGE_LOOP('',(#23855,#23856,#23857,#23858,#23859,#23860,#23861,#23862));
#9730=EDGE_LOOP('',(#23863,#23864,#23865,#23866));
#9731=EDGE_LOOP('',(#23867,#23868,#23869,#23870));
#9732=EDGE_LOOP('',(#23871,#23872,#23873,#23874,#23875,#23876,#23877,#23878));
#9733=EDGE_LOOP('',(#23879,#23880,#23881,#23882));
#9734=EDGE_LOOP('',(#23883,#23884,#23885,#23886,#23887,#23888,#23889,#23890));
#9735=EDGE_LOOP('',(#23891,#23892,#23893,#23894,#23895,#23896,#23897,#23898,
#23899,#23900,#23901,#23902,#23903,#23904,#23905,#23906,#23907,#23908));
#9736=EDGE_LOOP('',(#23909));
#9737=EDGE_LOOP('',(#23910,#23911,#23912,#23913));
#9738=EDGE_LOOP('',(#23914,#23915,#23916,#23917));
#9739=EDGE_LOOP('',(#23918,#23919,#23920,#23921));
#9740=EDGE_LOOP('',(#23922,#23923,#23924,#23925));
#9741=EDGE_LOOP('',(#23926,#23927,#23928,#23929));
#9742=EDGE_LOOP('',(#23930,#23931,#23932,#23933));
#9743=EDGE_LOOP('',(#23934,#23935,#23936,#23937));
#9744=EDGE_LOOP('',(#23938,#23939,#23940,#23941));
#9745=EDGE_LOOP('',(#23942,#23943,#23944,#23945));
#9746=EDGE_LOOP('',(#23946,#23947,#23948,#23949));
#9747=EDGE_LOOP('',(#23950,#23951,#23952,#23953));
#9748=EDGE_LOOP('',(#23954,#23955,#23956,#23957));
#9749=EDGE_LOOP('',(#23958,#23959,#23960,#23961));
#9750=EDGE_LOOP('',(#23962,#23963,#23964,#23965));
#9751=EDGE_LOOP('',(#23966,#23967,#23968,#23969));
#9752=EDGE_LOOP('',(#23970,#23971,#23972,#23973));
#9753=EDGE_LOOP('',(#23974,#23975,#23976,#23977));
#9754=EDGE_LOOP('',(#23978,#23979,#23980,#23981));
#9755=EDGE_LOOP('',(#23982,#23983,#23984,#23985));
#9756=EDGE_LOOP('',(#23986,#23987,#23988,#23989));
#9757=EDGE_LOOP('',(#23990,#23991,#23992));
#9758=EDGE_LOOP('',(#23993,#23994,#23995,#23996,#23997));
#9759=EDGE_LOOP('',(#23998,#23999,#24000,#24001));
#9760=EDGE_LOOP('',(#24002,#24003,#24004,#24005));
#9761=EDGE_LOOP('',(#24006,#24007,#24008,#24009));
#9762=EDGE_LOOP('',(#24010,#24011,#24012,#24013));
#9763=EDGE_LOOP('',(#24014,#24015,#24016,#24017));
#9764=EDGE_LOOP('',(#24018,#24019,#24020,#24021));
#9765=EDGE_LOOP('',(#24022,#24023,#24024,#24025));
#9766=EDGE_LOOP('',(#24026,#24027,#24028,#24029));
#9767=EDGE_LOOP('',(#24030,#24031,#24032,#24033));
#9768=EDGE_LOOP('',(#24034,#24035,#24036,#24037));
#9769=EDGE_LOOP('',(#24038,#24039,#24040,#24041));
#9770=EDGE_LOOP('',(#24042,#24043,#24044,#24045));
#9771=EDGE_LOOP('',(#24046,#24047,#24048,#24049));
#9772=EDGE_LOOP('',(#24050,#24051,#24052,#24053));
#9773=EDGE_LOOP('',(#24054,#24055,#24056,#24057));
#9774=EDGE_LOOP('',(#24058,#24059,#24060,#24061));
#9775=EDGE_LOOP('',(#24062,#24063,#24064,#24065));
#9776=EDGE_LOOP('',(#24066,#24067,#24068,#24069));
#9777=EDGE_LOOP('',(#24070,#24071,#24072,#24073,#24074,#24075,#24076,#24077,
#24078,#24079,#24080,#24081,#24082,#24083,#24084,#24085,#24086,#24087,#24088,
#24089,#24090,#24091,#24092,#24093,#24094,#24095,#24096,#24097,#24098,#24099,
#24100,#24101,#24102,#24103,#24104,#24105,#24106,#24107,#24108,#24109,#24110,
#24111,#24112));
#9778=EDGE_LOOP('',(#24113,#24114,#24115,#24116,#24117));
#9779=EDGE_LOOP('',(#24118,#24119,#24120,#24121));
#9780=EDGE_LOOP('',(#24122,#24123,#24124,#24125,#24126,#24127,#24128,#24129,
#24130,#24131,#24132,#24133,#24134,#24135,#24136,#24137,#24138,#24139,#24140,
#24141,#24142,#24143,#24144,#24145,#24146,#24147,#24148,#24149,#24150,#24151,
#24152,#24153,#24154,#24155,#24156,#24157,#24158,#24159,#24160,#24161,#24162,
#24163,#24164,#24165));
#9781=EDGE_LOOP('',(#24166,#24167,#24168,#24169,#24170,#24171,#24172,#24173,
#24174,#24175));
#9782=EDGE_LOOP('',(#24176,#24177,#24178,#24179));
#9783=EDGE_LOOP('',(#24180,#24181,#24182,#24183));
#9784=EDGE_LOOP('',(#24184,#24185,#24186,#24187));
#9785=EDGE_LOOP('',(#24188,#24189,#24190,#24191,#24192,#24193));
#9786=EDGE_LOOP('',(#24194,#24195,#24196,#24197,#24198));
#9787=EDGE_LOOP('',(#24199,#24200,#24201,#24202));
#9788=EDGE_LOOP('',(#24203,#24204,#24205,#24206));
#9789=EDGE_LOOP('',(#24207,#24208,#24209,#24210,#24211));
#9790=EDGE_LOOP('',(#24212));
#9791=EDGE_LOOP('',(#24213));
#9792=EDGE_LOOP('',(#24214,#24215,#24216,#24217,#24218,#24219));
#9793=EDGE_LOOP('',(#24220,#24221,#24222,#24223));
#9794=EDGE_LOOP('',(#24224,#24225,#24226,#24227));
#9795=EDGE_LOOP('',(#24228,#24229,#24230,#24231));
#9796=EDGE_LOOP('',(#24232,#24233,#24234,#24235));
#9797=EDGE_LOOP('',(#24236,#24237,#24238,#24239));
#9798=EDGE_LOOP('',(#24240,#24241,#24242,#24243));
#9799=EDGE_LOOP('',(#24244,#24245,#24246,#24247));
#9800=EDGE_LOOP('',(#24248,#24249,#24250,#24251));
#9801=EDGE_LOOP('',(#24252,#24253,#24254,#24255));
#9802=EDGE_LOOP('',(#24256,#24257,#24258,#24259));
#9803=EDGE_LOOP('',(#24260,#24261,#24262,#24263));
#9804=EDGE_LOOP('',(#24264,#24265,#24266,#24267));
#9805=EDGE_LOOP('',(#24268,#24269,#24270,#24271));
#9806=EDGE_LOOP('',(#24272,#24273,#24274,#24275));
#9807=EDGE_LOOP('',(#24276,#24277,#24278,#24279));
#9808=EDGE_LOOP('',(#24280,#24281,#24282,#24283));
#9809=EDGE_LOOP('',(#24284,#24285,#24286,#24287));
#9810=EDGE_LOOP('',(#24288,#24289,#24290,#24291));
#9811=EDGE_LOOP('',(#24292,#24293,#24294,#24295));
#9812=EDGE_LOOP('',(#24296,#24297,#24298,#24299));
#9813=EDGE_LOOP('',(#24300,#24301,#24302,#24303));
#9814=EDGE_LOOP('',(#24304,#24305,#24306));
#9815=EDGE_LOOP('',(#24307,#24308,#24309,#24310,#24311));
#9816=EDGE_LOOP('',(#24312,#24313,#24314,#24315));
#9817=EDGE_LOOP('',(#24316,#24317,#24318,#24319));
#9818=EDGE_LOOP('',(#24320,#24321,#24322,#24323));
#9819=EDGE_LOOP('',(#24324,#24325,#24326,#24327));
#9820=EDGE_LOOP('',(#24328,#24329,#24330,#24331));
#9821=EDGE_LOOP('',(#24332,#24333,#24334,#24335));
#9822=EDGE_LOOP('',(#24336,#24337,#24338,#24339));
#9823=EDGE_LOOP('',(#24340,#24341,#24342,#24343));
#9824=EDGE_LOOP('',(#24344,#24345,#24346,#24347));
#9825=EDGE_LOOP('',(#24348,#24349,#24350,#24351));
#9826=EDGE_LOOP('',(#24352,#24353,#24354,#24355));
#9827=EDGE_LOOP('',(#24356,#24357,#24358,#24359));
#9828=EDGE_LOOP('',(#24360,#24361,#24362,#24363));
#9829=EDGE_LOOP('',(#24364,#24365,#24366,#24367));
#9830=EDGE_LOOP('',(#24368,#24369,#24370,#24371));
#9831=EDGE_LOOP('',(#24372,#24373,#24374,#24375));
#9832=EDGE_LOOP('',(#24376,#24377,#24378,#24379));
#9833=EDGE_LOOP('',(#24380,#24381,#24382,#24383));
#9834=EDGE_LOOP('',(#24384,#24385,#24386,#24387,#24388,#24389,#24390,#24391,
#24392,#24393,#24394,#24395,#24396,#24397,#24398,#24399,#24400,#24401,#24402,
#24403,#24404,#24405,#24406,#24407,#24408,#24409,#24410,#24411,#24412,#24413,
#24414,#24415,#24416,#24417,#24418,#24419,#24420,#24421,#24422,#24423,#24424,
#24425,#24426));
#9835=EDGE_LOOP('',(#24427,#24428,#24429,#24430,#24431));
#9836=EDGE_LOOP('',(#24432,#24433,#24434,#24435));
#9837=EDGE_LOOP('',(#24436,#24437,#24438,#24439,#24440,#24441,#24442,#24443,
#24444,#24445,#24446,#24447,#24448,#24449,#24450,#24451,#24452,#24453,#24454,
#24455,#24456,#24457,#24458,#24459,#24460,#24461,#24462,#24463,#24464,#24465,
#24466,#24467,#24468,#24469,#24470,#24471,#24472,#24473,#24474,#24475,#24476,
#24477,#24478,#24479));
#9838=EDGE_LOOP('',(#24480,#24481,#24482,#24483));
#9839=EDGE_LOOP('',(#24484,#24485,#24486));
#9840=EDGE_LOOP('',(#24487,#24488,#24489,#24490));
#9841=EDGE_LOOP('',(#24491,#24492,#24493));
#9842=EDGE_LOOP('',(#24494,#24495,#24496,#24497));
#9843=EDGE_LOOP('',(#24498,#24499,#24500));
#9844=EDGE_LOOP('',(#24501,#24502,#24503,#24504));
#9845=EDGE_LOOP('',(#24505,#24506,#24507));
#9846=EDGE_LOOP('',(#24508,#24509,#24510,#24511));
#9847=EDGE_LOOP('',(#24512,#24513,#24514));
#9848=EDGE_LOOP('',(#24515,#24516,#24517,#24518));
#9849=EDGE_LOOP('',(#24519,#24520,#24521));
#9850=EDGE_LOOP('',(#24522,#24523,#24524,#24525));
#9851=EDGE_LOOP('',(#24526,#24527,#24528));
#9852=EDGE_LOOP('',(#24529,#24530,#24531,#24532));
#9853=EDGE_LOOP('',(#24533,#24534,#24535));
#9854=EDGE_LOOP('',(#24536,#24537,#24538,#24539));
#9855=EDGE_LOOP('',(#24540,#24541,#24542));
#9856=EDGE_LOOP('',(#24543,#24544,#24545,#24546));
#9857=EDGE_LOOP('',(#24547,#24548,#24549));
#9858=EDGE_LOOP('',(#24550,#24551,#24552,#24553));
#9859=EDGE_LOOP('',(#24554,#24555,#24556));
#9860=EDGE_LOOP('',(#24557,#24558,#24559,#24560));
#9861=EDGE_LOOP('',(#24561,#24562,#24563));
#9862=EDGE_LOOP('',(#24564,#24565,#24566,#24567));
#9863=EDGE_LOOP('',(#24568,#24569,#24570));
#9864=EDGE_LOOP('',(#24571,#24572,#24573,#24574));
#9865=EDGE_LOOP('',(#24575,#24576,#24577));
#9866=EDGE_LOOP('',(#24578,#24579,#24580,#24581));
#9867=EDGE_LOOP('',(#24582,#24583,#24584));
#9868=EDGE_LOOP('',(#24585,#24586,#24587,#24588));
#9869=EDGE_LOOP('',(#24589,#24590,#24591));
#9870=EDGE_LOOP('',(#24592,#24593,#24594,#24595));
#9871=EDGE_LOOP('',(#24596,#24597,#24598));
#9872=EDGE_LOOP('',(#24599,#24600,#24601,#24602));
#9873=EDGE_LOOP('',(#24603,#24604,#24605));
#9874=EDGE_LOOP('',(#24606,#24607,#24608,#24609));
#9875=EDGE_LOOP('',(#24610,#24611,#24612));
#9876=EDGE_LOOP('',(#24613,#24614,#24615,#24616));
#9877=EDGE_LOOP('',(#24617,#24618,#24619));
#9878=EDGE_LOOP('',(#24620,#24621,#24622,#24623));
#9879=EDGE_LOOP('',(#24624,#24625,#24626));
#9880=EDGE_LOOP('',(#24627,#24628,#24629,#24630));
#9881=EDGE_LOOP('',(#24631,#24632,#24633));
#9882=EDGE_LOOP('',(#24634,#24635,#24636,#24637));
#9883=EDGE_LOOP('',(#24638,#24639,#24640));
#9884=EDGE_LOOP('',(#24641,#24642,#24643,#24644));
#9885=EDGE_LOOP('',(#24645,#24646,#24647));
#9886=EDGE_LOOP('',(#24648,#24649,#24650,#24651));
#9887=EDGE_LOOP('',(#24652,#24653,#24654));
#9888=EDGE_LOOP('',(#24655,#24656,#24657,#24658));
#9889=EDGE_LOOP('',(#24659,#24660,#24661));
#9890=EDGE_LOOP('',(#24662,#24663,#24664,#24665));
#9891=EDGE_LOOP('',(#24666,#24667,#24668));
#9892=EDGE_LOOP('',(#24669,#24670,#24671,#24672));
#9893=EDGE_LOOP('',(#24673,#24674,#24675));
#9894=EDGE_LOOP('',(#24676,#24677,#24678,#24679));
#9895=EDGE_LOOP('',(#24680,#24681,#24682));
#9896=EDGE_LOOP('',(#24683,#24684,#24685,#24686));
#9897=EDGE_LOOP('',(#24687,#24688,#24689));
#9898=EDGE_LOOP('',(#24690,#24691,#24692,#24693));
#9899=EDGE_LOOP('',(#24694,#24695,#24696));
#9900=EDGE_LOOP('',(#24697,#24698,#24699,#24700));
#9901=EDGE_LOOP('',(#24701,#24702,#24703));
#9902=EDGE_LOOP('',(#24704,#24705,#24706,#24707));
#9903=EDGE_LOOP('',(#24708,#24709,#24710));
#9904=EDGE_LOOP('',(#24711,#24712,#24713,#24714));
#9905=EDGE_LOOP('',(#24715,#24716,#24717));
#9906=EDGE_LOOP('',(#24718,#24719,#24720,#24721));
#9907=EDGE_LOOP('',(#24722,#24723,#24724,#24725));
#9908=EDGE_LOOP('',(#24726,#24727,#24728,#24729));
#9909=EDGE_LOOP('',(#24730,#24731,#24732,#24733));
#9910=EDGE_LOOP('',(#24734,#24735,#24736,#24737));
#9911=EDGE_LOOP('',(#24738,#24739,#24740));
#9912=EDGE_LOOP('',(#24741,#24742,#24743,#24744));
#9913=EDGE_LOOP('',(#24745,#24746,#24747));
#9914=EDGE_LOOP('',(#24748,#24749,#24750,#24751));
#9915=EDGE_LOOP('',(#24752,#24753,#24754));
#9916=EDGE_LOOP('',(#24755,#24756,#24757,#24758));
#9917=EDGE_LOOP('',(#24759,#24760,#24761));
#9918=EDGE_LOOP('',(#24762,#24763,#24764,#24765));
#9919=EDGE_LOOP('',(#24766,#24767,#24768));
#9920=EDGE_LOOP('',(#24769,#24770,#24771,#24772));
#9921=EDGE_LOOP('',(#24773,#24774,#24775));
#9922=EDGE_LOOP('',(#24776,#24777,#24778,#24779));
#9923=EDGE_LOOP('',(#24780,#24781,#24782));
#9924=EDGE_LOOP('',(#24783,#24784,#24785,#24786));
#9925=EDGE_LOOP('',(#24787,#24788,#24789));
#9926=EDGE_LOOP('',(#24790,#24791,#24792,#24793));
#9927=EDGE_LOOP('',(#24794,#24795,#24796));
#9928=EDGE_LOOP('',(#24797,#24798,#24799,#24800));
#9929=EDGE_LOOP('',(#24801,#24802,#24803));
#9930=EDGE_LOOP('',(#24804,#24805,#24806,#24807));
#9931=EDGE_LOOP('',(#24808,#24809,#24810));
#9932=EDGE_LOOP('',(#24811,#24812,#24813,#24814));
#9933=EDGE_LOOP('',(#24815,#24816,#24817));
#9934=EDGE_LOOP('',(#24818,#24819,#24820,#24821));
#9935=EDGE_LOOP('',(#24822,#24823,#24824));
#9936=EDGE_LOOP('',(#24825,#24826,#24827,#24828));
#9937=EDGE_LOOP('',(#24829,#24830,#24831));
#9938=EDGE_LOOP('',(#24832,#24833,#24834,#24835));
#9939=EDGE_LOOP('',(#24836,#24837,#24838));
#9940=EDGE_LOOP('',(#24839,#24840,#24841,#24842));
#9941=EDGE_LOOP('',(#24843,#24844,#24845));
#9942=EDGE_LOOP('',(#24846,#24847,#24848,#24849));
#9943=EDGE_LOOP('',(#24850,#24851,#24852));
#9944=EDGE_LOOP('',(#24853,#24854,#24855,#24856));
#9945=EDGE_LOOP('',(#24857,#24858,#24859));
#9946=EDGE_LOOP('',(#24860,#24861,#24862,#24863));
#9947=EDGE_LOOP('',(#24864,#24865,#24866));
#9948=EDGE_LOOP('',(#24867,#24868,#24869,#24870));
#9949=EDGE_LOOP('',(#24871,#24872,#24873));
#9950=EDGE_LOOP('',(#24874,#24875,#24876,#24877));
#9951=EDGE_LOOP('',(#24878,#24879,#24880));
#9952=EDGE_LOOP('',(#24881,#24882,#24883,#24884));
#9953=EDGE_LOOP('',(#24885,#24886,#24887));
#9954=EDGE_LOOP('',(#24888,#24889,#24890,#24891));
#9955=EDGE_LOOP('',(#24892,#24893,#24894));
#9956=EDGE_LOOP('',(#24895,#24896,#24897,#24898));
#9957=EDGE_LOOP('',(#24899,#24900,#24901));
#9958=EDGE_LOOP('',(#24902,#24903,#24904,#24905));
#9959=EDGE_LOOP('',(#24906,#24907,#24908));
#9960=EDGE_LOOP('',(#24909,#24910,#24911,#24912));
#9961=EDGE_LOOP('',(#24913,#24914,#24915));
#9962=EDGE_LOOP('',(#24916,#24917,#24918,#24919));
#9963=EDGE_LOOP('',(#24920,#24921,#24922));
#9964=EDGE_LOOP('',(#24923,#24924,#24925,#24926));
#9965=EDGE_LOOP('',(#24927,#24928,#24929));
#9966=EDGE_LOOP('',(#24930,#24931,#24932,#24933));
#9967=EDGE_LOOP('',(#24934,#24935,#24936));
#9968=EDGE_LOOP('',(#24937,#24938,#24939,#24940));
#9969=EDGE_LOOP('',(#24941,#24942,#24943));
#9970=EDGE_LOOP('',(#24944,#24945,#24946,#24947));
#9971=EDGE_LOOP('',(#24948,#24949,#24950));
#9972=EDGE_LOOP('',(#24951,#24952,#24953,#24954));
#9973=EDGE_LOOP('',(#24955,#24956,#24957));
#9974=EDGE_LOOP('',(#24958,#24959,#24960,#24961));
#9975=EDGE_LOOP('',(#24962,#24963,#24964));
#9976=EDGE_LOOP('',(#24965,#24966,#24967,#24968));
#9977=EDGE_LOOP('',(#24969,#24970,#24971));
#9978=EDGE_LOOP('',(#24972,#24973,#24974,#24975));
#9979=EDGE_LOOP('',(#24976,#24977,#24978));
#9980=EDGE_LOOP('',(#24979,#24980,#24981,#24982));
#9981=EDGE_LOOP('',(#24983,#24984,#24985));
#9982=EDGE_LOOP('',(#24986,#24987,#24988,#24989));
#9983=EDGE_LOOP('',(#24990,#24991,#24992,#24993));
#9984=EDGE_LOOP('',(#24994,#24995,#24996,#24997));
#9985=EDGE_LOOP('',(#24998,#24999,#25000,#25001));
#9986=EDGE_LOOP('',(#25002,#25003,#25004,#25005));
#9987=EDGE_LOOP('',(#25006,#25007,#25008,#25009));
#9988=EDGE_LOOP('',(#25010,#25011,#25012,#25013,#25014,#25015));
#9989=EDGE_LOOP('',(#25016));
#9990=EDGE_LOOP('',(#25017,#25018,#25019,#25020,#25021,#25022));
#9991=EDGE_LOOP('',(#25023,#25024,#25025,#25026));
#9992=EDGE_LOOP('',(#25027));
#9993=EDGE_LOOP('',(#25028,#25029,#25030,#25031,#25032));
#9994=EDGE_LOOP('',(#25033,#25034,#25035,#25036,#25037,#25038,#25039,#25040,
#25041,#25042,#25043,#25044));
#9995=EDGE_LOOP('',(#25045,#25046,#25047,#25048));
#9996=EDGE_LOOP('',(#25049,#25050,#25051,#25052));
#9997=EDGE_LOOP('',(#25053,#25054,#25055,#25056));
#9998=EDGE_LOOP('',(#25057,#25058,#25059,#25060));
#9999=EDGE_LOOP('',(#25061,#25062,#25063,#25064));
#10000=EDGE_LOOP('',(#25065,#25066,#25067,#25068));
#10001=EDGE_LOOP('',(#25069,#25070,#25071,#25072));
#10002=EDGE_LOOP('',(#25073,#25074,#25075,#25076));
#10003=EDGE_LOOP('',(#25077,#25078,#25079,#25080));
#10004=EDGE_LOOP('',(#25081,#25082,#25083,#25084));
#10005=EDGE_LOOP('',(#25085,#25086,#25087,#25088));
#10006=EDGE_LOOP('',(#25089,#25090,#25091,#25092));
#10007=EDGE_LOOP('',(#25093,#25094,#25095,#25096));
#10008=EDGE_LOOP('',(#25097,#25098,#25099,#25100));
#10009=EDGE_LOOP('',(#25101,#25102,#25103,#25104));
#10010=EDGE_LOOP('',(#25105,#25106,#25107,#25108));
#10011=EDGE_LOOP('',(#25109,#25110,#25111,#25112));
#10012=EDGE_LOOP('',(#25113,#25114,#25115,#25116));
#10013=EDGE_LOOP('',(#25117,#25118,#25119,#25120));
#10014=EDGE_LOOP('',(#25121,#25122,#25123,#25124));
#10015=EDGE_LOOP('',(#25125,#25126,#25127,#25128));
#10016=EDGE_LOOP('',(#25129,#25130,#25131,#25132));
#10017=EDGE_LOOP('',(#25133,#25134,#25135,#25136));
#10018=EDGE_LOOP('',(#25137,#25138,#25139,#25140));
#10019=EDGE_LOOP('',(#25141,#25142,#25143,#25144));
#10020=EDGE_LOOP('',(#25145,#25146,#25147,#25148));
#10021=EDGE_LOOP('',(#25149,#25150,#25151,#25152));
#10022=EDGE_LOOP('',(#25153,#25154,#25155,#25156));
#10023=EDGE_LOOP('',(#25157,#25158,#25159,#25160));
#10024=EDGE_LOOP('',(#25161,#25162,#25163,#25164));
#10025=EDGE_LOOP('',(#25165,#25166,#25167,#25168));
#10026=EDGE_LOOP('',(#25169,#25170,#25171,#25172));
#10027=EDGE_LOOP('',(#25173,#25174,#25175,#25176));
#10028=EDGE_LOOP('',(#25177,#25178,#25179,#25180));
#10029=EDGE_LOOP('',(#25181,#25182,#25183,#25184));
#10030=EDGE_LOOP('',(#25185,#25186,#25187,#25188));
#10031=EDGE_LOOP('',(#25189));
#10032=EDGE_LOOP('',(#25190,#25191,#25192,#25193,#25194,#25195));
#10033=EDGE_LOOP('',(#25196,#25197,#25198));
#10034=EDGE_LOOP('',(#25199,#25200,#25201,#25202));
#10035=EDGE_LOOP('',(#25203,#25204,#25205));
#10036=EDGE_LOOP('',(#25206,#25207,#25208,#25209));
#10037=EDGE_LOOP('',(#25210,#25211,#25212,#25213));
#10038=EDGE_LOOP('',(#25214,#25215,#25216));
#10039=EDGE_LOOP('',(#25217,#25218,#25219,#25220));
#10040=EDGE_LOOP('',(#25221,#25222,#25223));
#10041=EDGE_LOOP('',(#25224,#25225,#25226,#25227));
#10042=EDGE_LOOP('',(#25228,#25229,#25230,#25231));
#10043=EDGE_LOOP('',(#25232,#25233,#25234));
#10044=EDGE_LOOP('',(#25235,#25236,#25237,#25238));
#10045=EDGE_LOOP('',(#25239,#25240,#25241));
#10046=EDGE_LOOP('',(#25242,#25243,#25244,#25245));
#10047=EDGE_LOOP('',(#25246,#25247,#25248,#25249));
#10048=EDGE_LOOP('',(#25250,#25251,#25252,#25253));
#10049=EDGE_LOOP('',(#25254,#25255,#25256,#25257));
#10050=EDGE_LOOP('',(#25258,#25259,#25260,#25261));
#10051=EDGE_LOOP('',(#25262,#25263,#25264,#25265));
#10052=EDGE_LOOP('',(#25266,#25267,#25268,#25269));
#10053=EDGE_LOOP('',(#25270,#25271,#25272,#25273));
#10054=EDGE_LOOP('',(#25274,#25275,#25276,#25277,#25278,#25279));
#10055=EDGE_LOOP('',(#25280,#25281,#25282,#25283,#25284,#25285));
#10056=EDGE_LOOP('',(#25286,#25287,#25288,#25289));
#10057=EDGE_LOOP('',(#25290,#25291,#25292,#25293));
#10058=EDGE_LOOP('',(#25294,#25295,#25296,#25297));
#10059=EDGE_LOOP('',(#25298,#25299,#25300,#25301));
#10060=EDGE_LOOP('',(#25302,#25303,#25304,#25305));
#10061=EDGE_LOOP('',(#25306,#25307,#25308,#25309));
#10062=EDGE_LOOP('',(#25310,#25311,#25312,#25313));
#10063=EDGE_LOOP('',(#25314,#25315,#25316,#25317));
#10064=EDGE_LOOP('',(#25318,#25319,#25320,#25321));
#10065=EDGE_LOOP('',(#25322,#25323,#25324,#25325));
#10066=EDGE_LOOP('',(#25326,#25327,#25328,#25329));
#10067=EDGE_LOOP('',(#25330,#25331,#25332,#25333));
#10068=EDGE_LOOP('',(#25334,#25335,#25336,#25337,#25338,#25339));
#10069=EDGE_LOOP('',(#25340,#25341,#25342,#25343,#25344,#25345,#25346,#25347,
#25348,#25349,#25350,#25351));
#10070=EDGE_LOOP('',(#25352));
#10071=EDGE_LOOP('',(#25353,#25354,#25355,#25356));
#10072=EDGE_LOOP('',(#25357,#25358,#25359,#25360));
#10073=EDGE_LOOP('',(#25361,#25362,#25363,#25364));
#10074=EDGE_LOOP('',(#25365));
#10075=EDGE_LOOP('',(#25366,#25367,#25368,#25369));
#10076=EDGE_LOOP('',(#25370,#25371,#25372,#25373));
#10077=EDGE_LOOP('',(#25374,#25375,#25376,#25377));
#10078=EDGE_LOOP('',(#25378,#25379,#25380,#25381));
#10079=EDGE_LOOP('',(#25382,#25383,#25384,#25385));
#10080=EDGE_LOOP('',(#25386,#25387,#25388,#25389));
#10081=EDGE_LOOP('',(#25390,#25391,#25392,#25393));
#10082=EDGE_LOOP('',(#25394,#25395,#25396,#25397));
#10083=EDGE_LOOP('',(#25398,#25399,#25400,#25401));
#10084=EDGE_LOOP('',(#25402,#25403,#25404,#25405));
#10085=EDGE_LOOP('',(#25406,#25407,#25408,#25409));
#10086=EDGE_LOOP('',(#25410,#25411,#25412,#25413));
#10087=EDGE_LOOP('',(#25414,#25415,#25416,#25417));
#10088=EDGE_LOOP('',(#25418,#25419,#25420,#25421));
#10089=EDGE_LOOP('',(#25422,#25423,#25424,#25425,#25426));
#10090=EDGE_LOOP('',(#25427,#25428,#25429,#25430));
#10091=EDGE_LOOP('',(#25431,#25432,#25433,#25434));
#10092=EDGE_LOOP('',(#25435,#25436,#25437,#25438));
#10093=EDGE_LOOP('',(#25439,#25440,#25441,#25442));
#10094=EDGE_LOOP('',(#25443,#25444,#25445,#25446));
#10095=EDGE_LOOP('',(#25447,#25448,#25449,#25450));
#10096=EDGE_LOOP('',(#25451,#25452,#25453,#25454));
#10097=EDGE_LOOP('',(#25455,#25456,#25457,#25458));
#10098=EDGE_LOOP('',(#25459,#25460,#25461,#25462));
#10099=EDGE_LOOP('',(#25463,#25464,#25465,#25466));
#10100=EDGE_LOOP('',(#25467,#25468,#25469,#25470));
#10101=EDGE_LOOP('',(#25471,#25472,#25473,#25474));
#10102=EDGE_LOOP('',(#25475,#25476,#25477,#25478,#25479,#25480,#25481,#25482,
#25483,#25484,#25485,#25486,#25487,#25488,#25489,#25490,#25491,#25492,#25493,
#25494,#25495,#25496,#25497,#25498,#25499,#25500,#25501,#25502,#25503));
#10103=EDGE_LOOP('',(#25504,#25505,#25506,#25507,#25508));
#10104=EDGE_LOOP('',(#25509,#25510,#25511,#25512));
#10105=EDGE_LOOP('',(#25513,#25514,#25515,#25516,#25517,#25518,#25519,#25520,
#25521,#25522,#25523,#25524,#25525,#25526,#25527,#25528,#25529,#25530,#25531,
#25532,#25533,#25534,#25535,#25536,#25537,#25538,#25539,#25540));
#10106=EDGE_LOOP('',(#25541,#25542,#25543,#25544));
#10107=EDGE_LOOP('',(#25545,#25546,#25547,#25548));
#10108=EDGE_LOOP('',(#25549,#25550,#25551,#25552));
#10109=EDGE_LOOP('',(#25553,#25554,#25555,#25556));
#10110=EDGE_LOOP('',(#25557,#25558,#25559,#25560));
#10111=EDGE_LOOP('',(#25561,#25562,#25563,#25564));
#10112=EDGE_LOOP('',(#25565,#25566,#25567,#25568,#25569,#25570));
#10113=EDGE_LOOP('',(#25571));
#10114=EDGE_LOOP('',(#25572,#25573,#25574,#25575,#25576,#25577));
#10115=EDGE_LOOP('',(#25578,#25579,#25580));
#10116=EDGE_LOOP('',(#25581));
#10117=EDGE_LOOP('',(#25582,#25583,#25584,#25585,#25586));
#10118=EDGE_LOOP('',(#25587,#25588,#25589,#25590,#25591,#25592,#25593,#25594,
#25595));
#10119=CIRCLE('',#27465,92.);
#10120=CIRCLE('',#27466,2.);
#10121=CIRCLE('',#27467,90.);
#10122=CIRCLE('',#27468,92.);
#10123=CIRCLE('',#27469,91.7320508075689);
#10124=CIRCLE('',#27471,92.);
#10125=CIRCLE('',#27472,92.);
#10126=CIRCLE('',#27473,92.);
#10127=CIRCLE('',#27474,92.);
#10128=CIRCLE('',#27476,5.05);
#10129=CIRCLE('',#27477,5.05);
#10130=CIRCLE('',#27478,5.05);
#10131=CIRCLE('',#27479,5.05);
#10132=CIRCLE('',#27480,13.);
#10133=CIRCLE('',#27482,2.);
#10134=CIRCLE('',#27483,90.);
#10135=CIRCLE('',#27484,92.);
#10136=CIRCLE('',#27485,92.);
#10137=CIRCLE('',#27487,5.05);
#10138=CIRCLE('',#27488,5.05);
#10139=CIRCLE('',#27489,5.05);
#10140=CIRCLE('',#27490,5.05);
#10141=CIRCLE('',#27491,5.05);
#10142=CIRCLE('',#27492,5.05);
#10143=CIRCLE('',#27493,5.05);
#10144=CIRCLE('',#27494,5.05);
#10145=CIRCLE('',#27495,72.2);
#10146=CIRCLE('',#27497,2.);
#10147=CIRCLE('',#27498,1.99999999999999);
#10148=CIRCLE('',#27499,1.99999999999999);
#10149=CIRCLE('',#27500,4.00000000000001);
#10150=CIRCLE('',#27501,2.00000000000001);
#10151=CIRCLE('',#27503,1.99999999999999);
#10152=CIRCLE('',#27504,1.99999999999999);
#10153=CIRCLE('',#27505,4.00000000000002);
#10154=CIRCLE('',#27506,2.00000000000002);
#10155=CIRCLE('',#27508,1.99999999999999);
#10156=CIRCLE('',#27509,1.99999999999999);
#10157=CIRCLE('',#27510,4.00000000000002);
#10158=CIRCLE('',#27511,2.00000000000002);
#10159=CIRCLE('',#27513,1.99999999999999);
#10160=CIRCLE('',#27514,4.00000000000002);
#10161=CIRCLE('',#27515,2.00000000000002);
#10162=CIRCLE('',#27517,4.00000000000002);
#10163=CIRCLE('',#27520,4.00000000000002);
#10164=CIRCLE('',#27523,7.);
#10165=CIRCLE('',#27524,7.);
#10166=CIRCLE('',#27526,1.99999999999999);
#10167=CIRCLE('',#27527,2.);
#10168=CIRCLE('',#27528,1.99999999999999);
#10169=CIRCLE('',#27529,2.00000000000002);
#10170=CIRCLE('',#27530,4.00000000000002);
#10171=CIRCLE('',#27532,2.);
#10172=CIRCLE('',#27533,2.);
#10173=CIRCLE('',#27534,2.00000000000002);
#10174=CIRCLE('',#27536,2.);
#10175=CIRCLE('',#27537,2.);
#10176=CIRCLE('',#27538,2.00000000000002);
#10177=CIRCLE('',#27540,2.);
#10178=CIRCLE('',#27541,2.00000000000001);
#10179=CIRCLE('',#27542,4.00000000000001);
#10180=CIRCLE('',#27547,6.00000000000001);
#10181=CIRCLE('',#27548,6.00000000000001);
#10182=CIRCLE('',#27549,6.00000000000001);
#10183=CIRCLE('',#27550,6.00000000000001);
#10184=CIRCLE('',#27551,7.);
#10185=CIRCLE('',#27552,7.);
#10186=CIRCLE('',#27554,1.99999999999998);
#10187=CIRCLE('',#27555,2.);
#10188=CIRCLE('',#27556,2.);
#10189=CIRCLE('',#27557,1.00000000000001);
#10190=CIRCLE('',#27558,3.00000000000001);
#10191=CIRCLE('',#27560,2.);
#10192=CIRCLE('',#27561,2.);
#10193=CIRCLE('',#27562,0.999999999999996);
#10194=CIRCLE('',#27563,3.);
#10195=CIRCLE('',#27565,2.);
#10196=CIRCLE('',#27566,2.);
#10197=CIRCLE('',#27567,0.999999999999989);
#10198=CIRCLE('',#27568,2.99999999999999);
#10199=CIRCLE('',#27570,2.);
#10200=CIRCLE('',#27571,0.999999999999998);
#10201=CIRCLE('',#27572,3.);
#10202=CIRCLE('',#27574,3.);
#10203=CIRCLE('',#27577,3.00000000000001);
#10204=CIRCLE('',#27580,6.9);
#10205=CIRCLE('',#27582,1.99999999999998);
#10206=CIRCLE('',#27583,2.);
#10207=CIRCLE('',#27584,2.);
#10208=CIRCLE('',#27585,0.999999999999993);
#10209=CIRCLE('',#27586,2.99999999999999);
#10210=CIRCLE('',#27588,2.);
#10211=CIRCLE('',#27589,2.);
#10212=CIRCLE('',#27590,1.);
#10213=CIRCLE('',#27591,3.);
#10214=CIRCLE('',#27593,2.);
#10215=CIRCLE('',#27594,2.);
#10216=CIRCLE('',#27595,1.00000000000001);
#10217=CIRCLE('',#27596,3.00000000000001);
#10218=CIRCLE('',#27598,2.);
#10219=CIRCLE('',#27599,0.999999999999989);
#10220=CIRCLE('',#27600,2.99999999999999);
#10221=CIRCLE('',#27602,3.);
#10222=CIRCLE('',#27605,2.99999999999999);
#10223=CIRCLE('',#27608,6.9);
#10224=CIRCLE('',#27610,2.);
#10225=CIRCLE('',#27611,70.2);
#10226=CIRCLE('',#27613,70.2);
#10227=CIRCLE('',#27614,70.2);
#10228=CIRCLE('',#27615,70.2);
#10229=CIRCLE('',#27617,22.05);
#10230=CIRCLE('',#27618,2.);
#10231=CIRCLE('',#27619,20.05);
#10232=CIRCLE('',#27621,55.);
#10233=CIRCLE('',#27623,20.05);
#10234=CIRCLE('',#27626,57.);
#10235=CIRCLE('',#27630,57.);
#10236=CIRCLE('',#27633,2.00000000000001);
#10237=CIRCLE('',#27634,16.75);
#10238=CIRCLE('',#27635,16.75);
#10239=CIRCLE('',#27636,1.99999999999999);
#10240=CIRCLE('',#27637,18.75);
#10241=CIRCLE('',#27638,2.);
#10242=CIRCLE('',#27640,2.);
#10243=CIRCLE('',#27641,18.75);
#10244=CIRCLE('',#27642,16.75);
#10245=CIRCLE('',#27644,5.99999999999997);
#10246=CIRCLE('',#27645,5.99999999999997);
#10247=CIRCLE('',#27648,16.75);
#10248=CIRCLE('',#27650,2.);
#10249=CIRCLE('',#27652,1.99999999999999);
#10250=CIRCLE('',#27653,2.);
#10251=CIRCLE('',#27655,2.);
#10252=CIRCLE('',#27656,5.99999999999996);
#10253=CIRCLE('',#27657,3.99999999999996);
#10254=CIRCLE('',#27660,5.99999999999999);
#10255=CIRCLE('',#27661,3.99999999999999);
#10256=CIRCLE('',#27663,5.99999999999996);
#10257=CIRCLE('',#27667,1.99999999999999);
#10258=CIRCLE('',#27668,1.99999999999999);
#10259=CIRCLE('',#27670,2.);
#10260=CIRCLE('',#27671,3.99999999999996);
#10261=CIRCLE('',#27673,2.);
#10262=CIRCLE('',#27675,2.00000000000001);
#10263=CIRCLE('',#27676,3.99999999999997);
#10264=CIRCLE('',#27678,1.99999999999999);
#10265=CIRCLE('',#27680,2.);
#10266=CIRCLE('',#27681,3.99999999999998);
#10267=CIRCLE('',#27682,5.99999999999998);
#10268=CIRCLE('',#27684,2.);
#10269=CIRCLE('',#27686,3.99999999999999);
#10270=CIRCLE('',#27687,5.99999999999999);
#10271=CIRCLE('',#27689,18.75);
#10272=CIRCLE('',#27691,3.);
#10273=CIRCLE('',#27692,2.99999999999999);
#10274=CIRCLE('',#27693,2.99999999999999);
#10275=CIRCLE('',#27694,3.00000000000001);
#10276=CIRCLE('',#27695,16.75);
#10277=CIRCLE('',#27697,1.99999999999999);
#10278=CIRCLE('',#27698,16.75);
#10279=CIRCLE('',#27699,16.75);
#10280=CIRCLE('',#27700,2.00000000000001);
#10281=CIRCLE('',#27701,2.);
#10282=CIRCLE('',#27703,1.99999999999999);
#10283=CIRCLE('',#27704,18.75);
#10284=CIRCLE('',#27705,16.75);
#10285=CIRCLE('',#27708,16.75);
#10286=CIRCLE('',#27712,6.9);
#10287=CIRCLE('',#27715,6.9);
#10288=CIRCLE('',#27718,16.75);
#10289=CIRCLE('',#27725,5.05);
#10290=CIRCLE('',#27728,5.05);
#10291=CIRCLE('',#27731,5.05);
#10292=CIRCLE('',#27734,5.05);
#10293=CIRCLE('',#27737,5.05);
#10294=CIRCLE('',#27740,5.05);
#10295=CIRCLE('',#27743,5.05);
#10296=CIRCLE('',#27746,5.05);
#10297=CIRCLE('',#27749,5.05);
#10298=CIRCLE('',#27752,5.05);
#10299=CIRCLE('',#27755,5.05);
#10300=CIRCLE('',#27758,5.05);
#10301=CIRCLE('',#27762,13.);
#10302=CIRCLE('',#27782,5.99999999999998);
#10303=CIRCLE('',#27788,56.5);
#10304=CIRCLE('',#27789,56.5);
#10305=CIRCLE('',#27797,56.5);
#10306=CIRCLE('',#27799,1.5);
#10307=CIRCLE('',#27803,56.5);
#10308=CIRCLE('',#27811,56.5);
#10309=CIRCLE('',#27818,92.);
#10310=CIRCLE('',#27819,1.5);
#10311=CIRCLE('',#27820,91.5606601717798);
#10312=CIRCLE('',#27822,91.4393398282202);
#10313=CIRCLE('',#27824,92.);
#10314=CIRCLE('',#27826,1.5);
#10315=CIRCLE('',#27827,90.3786796564403);
#10316=CIRCLE('',#27829,5.5);
#10317=CIRCLE('',#27830,5.5);
#10318=CIRCLE('',#27831,5.5);
#10319=CIRCLE('',#27832,5.5);
#10320=CIRCLE('',#27833,5.5);
#10321=CIRCLE('',#27834,5.5);
#10322=CIRCLE('',#27835,5.5);
#10323=CIRCLE('',#27836,5.5);
#10324=CIRCLE('',#27837,56.5);
#10325=CIRCLE('',#27838,1.5);
#10326=CIRCLE('',#27839,56.5);
#10327=CIRCLE('',#27840,56.5);
#10328=CIRCLE('',#27841,56.5);
#10329=CIRCLE('',#27847,90.5);
#10330=CIRCLE('',#27848,1.5);
#10331=CIRCLE('',#27850,76.55);
#10332=CIRCLE('',#27851,5.5);
#10333=CIRCLE('',#27852,5.5);
#10334=CIRCLE('',#27853,76.55);
#10335=CIRCLE('',#27854,5.5);
#10336=CIRCLE('',#27855,5.5);
#10337=CIRCLE('',#27856,76.55);
#10338=CIRCLE('',#27857,5.5);
#10339=CIRCLE('',#27858,5.5);
#10340=CIRCLE('',#27859,76.55);
#10341=CIRCLE('',#27860,5.5);
#10342=CIRCLE('',#27861,5.5);
#10343=CIRCLE('',#27862,76.55);
#10344=CIRCLE('',#27863,5.5);
#10345=CIRCLE('',#27864,5.5);
#10346=CIRCLE('',#27865,76.55);
#10347=CIRCLE('',#27866,5.5);
#10348=CIRCLE('',#27867,5.5);
#10349=CIRCLE('',#27868,76.55);
#10350=CIRCLE('',#27869,76.55);
#10351=CIRCLE('',#27870,5.5);
#10352=CIRCLE('',#27871,5.5);
#10353=CIRCLE('',#27872,76.55);
#10354=CIRCLE('',#27873,5.5);
#10355=CIRCLE('',#27874,5.5);
#10356=CIRCLE('',#27876,55.9393398282202);
#10357=CIRCLE('',#27877,1.5);
#10358=CIRCLE('',#27878,54.8786796564404);
#10359=CIRCLE('',#27880,56.0606601717798);
#10360=CIRCLE('',#27884,1.5);
#10361=CIRCLE('',#27886,1.5);
#10362=CIRCLE('',#27890,56.5);
#10363=CIRCLE('',#27891,1.5);
#10364=CIRCLE('',#27896,55.5);
#10365=CIRCLE('',#27897,57.);
#10366=CIRCLE('',#27901,70.2);
#10367=CIRCLE('',#27903,70.2);
#10368=CIRCLE('',#27904,70.2);
#10369=CIRCLE('',#27905,1.5);
#10370=CIRCLE('',#27906,71.95);
#10371=CIRCLE('',#27908,70.2);
#10372=CIRCLE('',#27909,70.2);
#10373=CIRCLE('',#27911,1.5);
#10374=CIRCLE('',#27912,75.05);
#10375=CIRCLE('',#27913,75.05);
#10376=CIRCLE('',#27919,75.05);
#10377=CIRCLE('',#27921,1.5);
#10378=CIRCLE('',#27922,1.5);
#10379=CIRCLE('',#27924,1.5);
#10380=CIRCLE('',#27925,1.5);
#10381=CIRCLE('',#27927,1.5);
#10382=CIRCLE('',#27928,1.5);
#10383=CIRCLE('',#27984,57.);
#10384=CIRCLE('',#27991,26.51);
#10385=CIRCLE('',#27992,26.01);
#10386=CIRCLE('',#27994,26.01);
#10387=CIRCLE('',#27996,6.00000000000002);
#10388=CIRCLE('',#27997,6.00000000000002);
#10389=CIRCLE('',#27998,6.00000000000002);
#10390=CIRCLE('',#27999,6.00000000000002);
#10391=CIRCLE('',#28001,26.51);
#10392=CIRCLE('',#28003,27.5);
#10393=CIRCLE('',#28005,7.5);
#10394=CIRCLE('',#28006,7.);
#10395=CIRCLE('',#28008,4.);
#10396=CIRCLE('',#28009,3.99999999999999);
#10397=CIRCLE('',#28010,4.);
#10398=CIRCLE('',#28011,3.99999999999999);
#10399=CIRCLE('',#28012,7.5);
#10400=CIRCLE('',#28013,3.99999999999998);
#10401=CIRCLE('',#28014,3.99999999999999);
#10402=CIRCLE('',#28015,3.99999999999998);
#10403=CIRCLE('',#28016,3.99999999999999);
#10404=CIRCLE('',#28018,7.);
#10405=CIRCLE('',#28020,7.);
#10406=CIRCLE('',#28022,7.);
#10407=CIRCLE('',#28024,2.55);
#10408=CIRCLE('',#28025,3.05);
#10409=CIRCLE('',#28027,3.05);
#10410=CIRCLE('',#28028,3.05);
#10411=CIRCLE('',#28029,3.05);
#10412=CIRCLE('',#28030,7.99999999999999);
#10413=CIRCLE('',#28031,8.00000000000001);
#10414=CIRCLE('',#28032,8.00000000000001);
#10415=CIRCLE('',#28033,7.99999999999998);
#10416=CIRCLE('',#28035,2.55);
#10417=CIRCLE('',#28037,2.55);
#10418=CIRCLE('',#28038,2.55);
#10419=CIRCLE('',#28040,6.00000000000002);
#10420=CIRCLE('',#28042,2.55);
#10421=CIRCLE('',#28044,2.55);
#10422=CIRCLE('',#28046,2.55);
#10423=CIRCLE('',#28048,2.55);
#10424=CIRCLE('',#28049,2.55);
#10425=CIRCLE('',#28051,2.55);
#10426=CIRCLE('',#28053,3.05);
#10427=CIRCLE('',#28055,3.05);
#10428=CIRCLE('',#28056,3.05);
#10429=CIRCLE('',#28057,7.99999999999998);
#10430=CIRCLE('',#28058,8.00000000000001);
#10431=CIRCLE('',#28059,8.00000000000001);
#10432=CIRCLE('',#28060,7.99999999999999);
#10433=CIRCLE('',#28061,3.05);
#10434=CIRCLE('',#28066,7.5);
#10435=CIRCLE('',#28067,7.);
#10436=CIRCLE('',#28069,123.);
#10437=CIRCLE('',#28070,7.5);
#10438=CIRCLE('',#28071,7.5);
#10439=CIRCLE('',#28072,92.1);
#10440=CIRCLE('',#28073,7.50000000000001);
#10441=CIRCLE('',#28075,7.);
#10442=CIRCLE('',#28077,7.);
#10443=CIRCLE('',#28079,7.);
#10444=CIRCLE('',#28081,7.);
#10445=CIRCLE('',#28083,7.);
#10446=CIRCLE('',#28085,6.99999999999999);
#10447=CIRCLE('',#28087,6.99999999999999);
#10448=CIRCLE('',#28089,7.5);
#10449=CIRCLE('',#28091,1.99999999999999);
#10450=CIRCLE('',#28092,2.);
#10451=CIRCLE('',#28093,1.99999999999999);
#10452=CIRCLE('',#28094,2.);
#10453=CIRCLE('',#28095,7.5);
#10454=CIRCLE('',#28098,70.);
#10455=CIRCLE('',#28099,2.);
#10456=CIRCLE('',#28100,68.);
#10457=CIRCLE('',#28102,70.);
#10458=CIRCLE('',#28104,5.5);
#10459=CIRCLE('',#28105,5.5);
#10460=CIRCLE('',#28106,5.5);
#10461=CIRCLE('',#28107,5.5);
#10462=CIRCLE('',#28108,45.);
#10463=CIRCLE('',#28110,2.);
#10464=CIRCLE('',#28111,68.);
#10465=CIRCLE('',#28113,22.5);
#10466=CIRCLE('',#28114,5.5);
#10467=CIRCLE('',#28115,5.5);
#10468=CIRCLE('',#28116,5.5);
#10469=CIRCLE('',#28117,5.5);
#10470=CIRCLE('',#28119,124.428189413237);
#10471=CIRCLE('',#28120,2.);
#10472=CIRCLE('',#28121,123.40620812114);
#10473=CIRCLE('',#28123,119.131441995709);
#10474=CIRCLE('',#28125,125.);
#10475=CIRCLE('',#28127,2.);
#10476=CIRCLE('',#28128,118.866225531784);
#10477=CIRCLE('',#28130,79.7142857142859);
#10478=CIRCLE('',#28131,64.06344373784);
#10479=CIRCLE('',#28132,64.06344373784);
#10480=CIRCLE('',#28133,64.06344373784);
#10481=CIRCLE('',#28134,79.7142857142859);
#10482=CIRCLE('',#28136,63.9364279314891);
#10483=CIRCLE('',#28139,63.9364279314891);
#10484=CIRCLE('',#28142,63.9364279314891);
#10485=CIRCLE('',#28145,1.99999999999998);
#10486=CIRCLE('',#28146,1.99999999999999);
#10487=CIRCLE('',#28147,1.99999999999999);
#10488=CIRCLE('',#28148,4.);
#10489=CIRCLE('',#28150,1.99999999999999);
#10490=CIRCLE('',#28151,1.99999999999999);
#10491=CIRCLE('',#28152,3.99999999999999);
#10492=CIRCLE('',#28154,1.99999999999999);
#10493=CIRCLE('',#28155,1.99999999999999);
#10494=CIRCLE('',#28156,4.);
#10495=CIRCLE('',#28158,1.99999999999999);
#10496=CIRCLE('',#28159,3.99999999999999);
#10497=CIRCLE('',#28165,2.);
#10498=CIRCLE('',#28166,125.);
#10499=CIRCLE('',#28169,47.);
#10500=CIRCLE('',#28170,2.);
#10501=CIRCLE('',#28171,45.);
#10502=CIRCLE('',#28172,47.);
#10503=CIRCLE('',#28173,47.);
#10504=CIRCLE('',#28174,47.);
#10505=CIRCLE('',#28176,6.00000000000002);
#10506=CIRCLE('',#28178,6.00000000000002);
#10507=CIRCLE('',#28181,6.00000000000002);
#10508=CIRCLE('',#28183,45.);
#10509=CIRCLE('',#28185,2.);
#10510=CIRCLE('',#28186,90.1);
#10511=CIRCLE('',#28187,90.1);
#10512=CIRCLE('',#28189,90.1);
#10513=CIRCLE('',#28191,2.);
#10514=CIRCLE('',#28192,47.);
#10515=CIRCLE('',#28195,1.99999999999999);
#10516=CIRCLE('',#28196,2.00000000000001);
#10517=CIRCLE('',#28198,1.99999999999999);
#10518=CIRCLE('',#28199,7.99999999999998);
#10519=CIRCLE('',#28200,5.99999999999998);
#10520=CIRCLE('',#28202,1.99999999999999);
#10521=CIRCLE('',#28204,2.);
#10522=CIRCLE('',#28205,7.99999999999999);
#10523=CIRCLE('',#28206,5.99999999999999);
#10524=CIRCLE('',#28208,2.);
#10525=CIRCLE('',#28210,1.99999999999999);
#10526=CIRCLE('',#28211,8.00000000000001);
#10527=CIRCLE('',#28212,6.00000000000001);
#10528=CIRCLE('',#28214,1.99999999999999);
#10529=CIRCLE('',#28216,8.00000000000001);
#10530=CIRCLE('',#28217,6.00000000000001);
#10531=CIRCLE('',#28219,5.99999999999999);
#10532=CIRCLE('',#28222,5.99999999999998);
#10533=CIRCLE('',#28226,2.);
#10534=CIRCLE('',#28227,2.);
#10535=CIRCLE('',#28229,1.99999999999999);
#10536=CIRCLE('',#28230,8.00000000000001);
#10537=CIRCLE('',#28231,6.00000000000001);
#10538=CIRCLE('',#28233,1.99999999999999);
#10539=CIRCLE('',#28235,2.);
#10540=CIRCLE('',#28236,8.00000000000001);
#10541=CIRCLE('',#28237,6.00000000000001);
#10542=CIRCLE('',#28239,2.);
#10543=CIRCLE('',#28241,1.99999999999999);
#10544=CIRCLE('',#28242,7.99999999999999);
#10545=CIRCLE('',#28244,1.99999999999999);
#10546=CIRCLE('',#28246,7.99999999999998);
#10547=CIRCLE('',#28252,1.99999999999999);
#10548=CIRCLE('',#28253,2.);
#10549=CIRCLE('',#28255,2.);
#10550=CIRCLE('',#28256,6.);
#10551=CIRCLE('',#28257,8.);
#10552=CIRCLE('',#28259,2.);
#10553=CIRCLE('',#28261,2.);
#10554=CIRCLE('',#28262,6.);
#10555=CIRCLE('',#28263,8.);
#10556=CIRCLE('',#28265,2.);
#10557=CIRCLE('',#28267,2.);
#10558=CIRCLE('',#28268,6.);
#10559=CIRCLE('',#28269,8.);
#10560=CIRCLE('',#28271,2.);
#10561=CIRCLE('',#28273,8.);
#10562=CIRCLE('',#28274,6.);
#10563=CIRCLE('',#28277,3.99999999999999);
#10564=CIRCLE('',#28278,3.99999999999998);
#10565=CIRCLE('',#28279,3.99999999999999);
#10566=CIRCLE('',#28280,3.99999999999998);
#10567=CIRCLE('',#28283,40.2777777777778);
#10568=CIRCLE('',#28285,1.99999999999999);
#10569=CIRCLE('',#28286,1.99999999999999);
#10570=CIRCLE('',#28288,2.);
#10571=CIRCLE('',#28289,5.99999999999998);
#10572=CIRCLE('',#28291,2.);
#10573=CIRCLE('',#28293,1.99999999999999);
#10574=CIRCLE('',#28294,6.00000000000001);
#10575=CIRCLE('',#28296,1.99999999999999);
#10576=CIRCLE('',#28298,2.);
#10577=CIRCLE('',#28299,6.00000000000001);
#10578=CIRCLE('',#28301,2.);
#10579=CIRCLE('',#28303,5.99999999999999);
#10580=CIRCLE('',#28305,6.00000000000001);
#10581=CIRCLE('',#28308,5.99999999999998);
#10582=CIRCLE('',#28311,2.);
#10583=CIRCLE('',#28312,1.99999999999999);
#10584=CIRCLE('',#28314,2.);
#10585=CIRCLE('',#28315,5.99999999999999);
#10586=CIRCLE('',#28317,2.);
#10587=CIRCLE('',#28319,1.99999999999999);
#10588=CIRCLE('',#28320,6.00000000000001);
#10589=CIRCLE('',#28322,1.99999999999999);
#10590=CIRCLE('',#28324,2.);
#10591=CIRCLE('',#28326,2.00000000000001);
#10592=CIRCLE('',#28342,27.5);
#10593=CIRCLE('',#28343,26.01);
#10594=CIRCLE('',#28346,26.01);
#10595=CIRCLE('',#28347,22.5);
#10596=CIRCLE('',#28376,70.);
#10597=CIRCLE('',#28378,70.);
#10598=CIRCLE('',#28380,70.);
#10599=CIRCLE('',#28382,70.);
#10600=CIRCLE('',#28384,70.);
#10601=CIRCLE('',#28385,70.);
#10602=CIRCLE('',#28387,70.);
#10603=CIRCLE('',#28389,70.);
#10604=CIRCLE('',#28391,70.);
#10605=CIRCLE('',#28393,70.);
#10606=CIRCLE('',#28395,70.);
#10607=CIRCLE('',#28397,70.);
#10608=CIRCLE('',#28399,70.);
#10609=CIRCLE('',#28401,70.);
#10610=CIRCLE('',#28403,70.);
#10611=CIRCLE('',#28405,70.);
#10612=CIRCLE('',#28407,70.);
#10613=CIRCLE('',#28409,70.);
#10614=CIRCLE('',#28411,70.);
#10615=CIRCLE('',#28413,70.);
#10616=CIRCLE('',#28415,70.);
#10617=CIRCLE('',#28417,70.);
#10618=CIRCLE('',#28419,70.);
#10619=CIRCLE('',#28421,70.);
#10620=CIRCLE('',#28423,70.);
#10621=CIRCLE('',#28425,70.);
#10622=CIRCLE('',#28427,70.);
#10623=CIRCLE('',#28429,70.);
#10624=CIRCLE('',#28431,70.);
#10625=CIRCLE('',#28433,70.);
#10626=CIRCLE('',#28435,70.);
#10627=CIRCLE('',#28437,70.);
#10628=CIRCLE('',#28439,70.);
#10629=CIRCLE('',#28441,70.);
#10630=CIRCLE('',#28443,70.);
#10631=CIRCLE('',#28445,70.);
#10632=CIRCLE('',#28447,70.);
#10633=CIRCLE('',#28449,70.);
#10634=CIRCLE('',#28451,70.);
#10635=CIRCLE('',#28453,70.);
#10636=CIRCLE('',#28455,70.);
#10637=CIRCLE('',#28457,70.);
#10638=CIRCLE('',#28459,70.);
#10639=CIRCLE('',#28461,70.);
#10640=CIRCLE('',#28463,70.);
#10641=CIRCLE('',#28465,70.);
#10642=CIRCLE('',#28467,70.);
#10643=CIRCLE('',#28469,70.);
#10644=CIRCLE('',#28471,70.);
#10645=CIRCLE('',#28473,70.);
#10646=CIRCLE('',#28475,70.);
#10647=CIRCLE('',#28477,70.);
#10648=CIRCLE('',#28479,70.);
#10649=CIRCLE('',#28481,70.);
#10650=CIRCLE('',#28483,70.);
#10651=CIRCLE('',#28485,70.);
#10652=CIRCLE('',#28487,70.);
#10653=CIRCLE('',#28489,70.);
#10654=CIRCLE('',#28491,70.);
#10655=CIRCLE('',#28493,70.);
#10656=CIRCLE('',#28495,70.);
#10657=CIRCLE('',#28497,70.);
#10658=CIRCLE('',#28499,70.);
#10659=CIRCLE('',#28501,70.);
#10660=CIRCLE('',#28503,70.);
#10661=CIRCLE('',#28505,70.);
#10662=CIRCLE('',#28506,70.);
#10663=CIRCLE('',#28508,70.);
#10664=CIRCLE('',#28510,70.);
#10665=CIRCLE('',#28512,70.);
#10666=CIRCLE('',#28514,70.);
#10667=CIRCLE('',#28516,70.);
#10668=CIRCLE('',#28518,70.);
#10669=CIRCLE('',#28520,70.);
#10670=CIRCLE('',#28522,70.);
#10671=CIRCLE('',#28524,70.);
#10672=CIRCLE('',#28526,70.);
#10673=CIRCLE('',#28528,70.);
#10674=CIRCLE('',#28530,70.);
#10675=CIRCLE('',#28532,70.);
#10676=CIRCLE('',#28534,70.);
#10677=CIRCLE('',#28536,70.);
#10678=CIRCLE('',#28538,70.);
#10679=CIRCLE('',#28540,70.);
#10680=CIRCLE('',#28542,70.);
#10681=CIRCLE('',#28544,70.);
#10682=CIRCLE('',#28546,70.);
#10683=CIRCLE('',#28548,70.);
#10684=CIRCLE('',#28550,70.);
#10685=CIRCLE('',#28552,70.);
#10686=CIRCLE('',#28554,70.);
#10687=CIRCLE('',#28556,70.);
#10688=CIRCLE('',#28558,70.);
#10689=CIRCLE('',#28560,70.);
#10690=CIRCLE('',#28562,70.);
#10691=CIRCLE('',#28564,70.);
#10692=CIRCLE('',#28566,70.);
#10693=CIRCLE('',#28568,70.);
#10694=CIRCLE('',#28570,70.);
#10695=CIRCLE('',#28572,70.);
#10696=CIRCLE('',#28574,70.);
#10697=CIRCLE('',#28576,70.);
#10698=CIRCLE('',#28578,70.);
#10699=CIRCLE('',#28580,70.);
#10700=CIRCLE('',#28582,70.);
#10701=CIRCLE('',#28584,70.);
#10702=CIRCLE('',#28586,70.);
#10703=CIRCLE('',#28588,70.);
#10704=CIRCLE('',#28590,70.);
#10705=CIRCLE('',#28592,70.);
#10706=CIRCLE('',#28594,70.);
#10707=CIRCLE('',#28596,70.);
#10708=CIRCLE('',#28598,70.);
#10709=CIRCLE('',#28600,70.);
#10710=CIRCLE('',#28602,70.);
#10711=CIRCLE('',#28604,70.);
#10712=CIRCLE('',#28606,70.);
#10713=CIRCLE('',#28608,70.);
#10714=CIRCLE('',#28610,70.);
#10715=CIRCLE('',#28612,70.);
#10716=CIRCLE('',#28614,70.);
#10717=CIRCLE('',#28616,70.);
#10718=CIRCLE('',#28641,10.01);
#10719=CIRCLE('',#28642,10.01);
#10720=CIRCLE('',#28781,10.01);
#10721=CIRCLE('',#28782,10.01);
#10722=CIRCLE('',#29071,10.);
#10723=CIRCLE('',#29075,10.);
#10724=CIRCLE('',#29079,9.6);
#10725=CIRCLE('',#29081,10.);
#10726=CIRCLE('',#29083,10.);
#10727=CIRCLE('',#29085,12.5);
#10728=CIRCLE('',#29087,12.5);
#10729=CIRCLE('',#29089,15.);
#10730=CIRCLE('',#29091,15.);
#10731=CIRCLE('',#29093,12.5);
#10732=CIRCLE('',#29095,12.5);
#10733=CIRCLE('',#29097,11.95);
#10734=CIRCLE('',#29099,11.95);
#10735=CIRCLE('',#29101,12.5);
#10736=CIRCLE('',#29103,12.5);
#10737=CIRCLE('',#29105,10.);
#10738=CIRCLE('',#29107,10.);
#10739=CIRCLE('',#29109,9.5);
#10740=CIRCLE('',#29113,16.);
#10741=CIRCLE('',#29114,15.8);
#10742=CIRCLE('',#29116,22.6);
#10743=CIRCLE('',#29118,22.8);
#10744=CIRCLE('',#29120,25.55);
#10745=CIRCLE('',#29122,26.);
#10746=CIRCLE('',#29124,26.);
#10747=CIRCLE('',#29126,25.55);
#10748=CIRCLE('',#29128,22.8);
#10749=CIRCLE('',#29130,22.6);
#10750=CIRCLE('',#29132,16.);
#10751=CIRCLE('',#29134,15.8);
#10752=CIRCLE('',#29136,12.95);
#10753=CIRCLE('',#29138,12.5);
#10754=CIRCLE('',#29140,12.5);
#10755=CIRCLE('',#29142,12.95);
#10756=CIRCLE('',#29146,17.5);
#10757=CIRCLE('',#29147,18.);
#10758=CIRCLE('',#29148,18.);
#10759=CIRCLE('',#29150,18.);
#10760=CIRCLE('',#29152,16.);
#10761=CIRCLE('',#29154,10.);
#10762=CIRCLE('',#29155,10.);
#10763=CIRCLE('',#29157,17.);
#10764=CIRCLE('',#29160,16.);
#10765=CIRCLE('',#29162,13.);
#10766=CIRCLE('',#29164,13.);
#10767=CIRCLE('',#29168,13.);
#10768=CIRCLE('',#29169,13.);
#10769=CIRCLE('',#29171,19.5);
#10770=CIRCLE('',#29173,20.);
#10771=CIRCLE('',#29175,20.);
#10772=CIRCLE('',#29179,2.2);
#10773=CIRCLE('',#29181,2.5);
#10774=CIRCLE('',#29183,2.5);
#10775=CIRCLE('',#29185,2.2);
#10776=CIRCLE('',#29189,12.55);
#10777=CIRCLE('',#29190,12.55);
#10778=CIRCLE('',#29192,16.);
#10779=CIRCLE('',#29194,16.);
#10780=CIRCLE('',#29198,1.5);
#10781=CIRCLE('',#29199,72.);
#10782=CIRCLE('',#29204,15.8);
#10783=CIRCLE('',#29205,16.);
#10784=CIRCLE('',#29209,11.95);
#10785=CIRCLE('',#29215,16.);
#10786=CIRCLE('',#29216,15.8);
#10787=CIRCLE('',#29218,11.95);
#10788=CIRCLE('',#29231,22.2);
#10789=CIRCLE('',#29232,22.);
#10790=CIRCLE('',#29239,22.2);
#10791=CIRCLE('',#29240,22.);
#10792=CIRCLE('',#29245,27.5);
#10793=CIRCLE('',#29249,27.5);
#10794=CIRCLE('',#29254,13.4732);
#10795=CIRCLE('',#29255,14.4062095263144);
#10796=CIRCLE('',#29271,16.7);
#10797=CIRCLE('',#29274,16.7);
#10798=CIRCLE('',#29277,16.7);
#10799=CIRCLE('',#29282,16.7);
#10800=CIRCLE('',#29284,16.7);
#10801=CIRCLE('',#29286,16.7);
#10802=CIRCLE('',#29289,16.7);
#10803=CIRCLE('',#29291,16.7);
#10804=CIRCLE('',#29293,16.7);
#10805=CIRCLE('',#29295,16.7);
#10806=CIRCLE('',#29297,16.7);
#10807=CIRCLE('',#29299,16.7);
#10808=CIRCLE('',#29300,16.7);
#10809=CIRCLE('',#29302,16.2);
#10810=CIRCLE('',#29304,16.7);
#10811=CIRCLE('',#29309,4.80000000000002);
#10812=CIRCLE('',#29310,5.00000000000002);
#10813=CIRCLE('',#29313,4.80000000000001);
#10814=CIRCLE('',#29314,5.00000000000001);
#10815=CIRCLE('',#29317,4.80000000000002);
#10816=CIRCLE('',#29318,5.00000000000004);
#10817=CIRCLE('',#29321,4.8);
#10818=CIRCLE('',#29322,5.00000000000001);
#10819=CIRCLE('',#29324,5.00000000000001);
#10820=CIRCLE('',#29327,5.00000000000002);
#10821=CIRCLE('',#29330,2.75);
#10822=CIRCLE('',#29331,2.75);
#10823=CIRCLE('',#29332,2.75);
#10824=CIRCLE('',#29333,2.75);
#10825=CIRCLE('',#29334,3.99999999999998);
#10826=CIRCLE('',#29335,3.99999999999999);
#10827=CIRCLE('',#29336,4.00000000000002);
#10828=CIRCLE('',#29337,4.00000000000002);
#10829=CIRCLE('',#29340,4.8);
#10830=CIRCLE('',#29341,5.00000000000001);
#10831=CIRCLE('',#29344,4.80000000000002);
#10832=CIRCLE('',#29345,5.00000000000004);
#10833=CIRCLE('',#29348,4.80000000000001);
#10834=CIRCLE('',#29351,4.80000000000002);
#10835=CIRCLE('',#29356,2.75);
#10836=CIRCLE('',#29357,2.75);
#10837=CIRCLE('',#29358,2.75);
#10838=CIRCLE('',#29359,2.75);
#10839=CIRCLE('',#29362,3.80000000000002);
#10840=CIRCLE('',#29363,4.00000000000002);
#10841=CIRCLE('',#29366,3.80000000000002);
#10842=CIRCLE('',#29367,4.00000000000002);
#10843=CIRCLE('',#29370,3.79999999999997);
#10844=CIRCLE('',#29371,3.99999999999999);
#10845=CIRCLE('',#29374,3.79999999999997);
#10846=CIRCLE('',#29375,3.99999999999998);
#10847=CIRCLE('',#29392,24.3535533905933);
#10848=CIRCLE('',#29393,24.3535533905933);
#10849=CIRCLE('',#29394,23.5);
#10850=CIRCLE('',#29396,24.6464466094067);
#10851=CIRCLE('',#29397,24.6464466094067);
#10852=CIRCLE('',#29398,24.);
#10853=CIRCLE('',#29399,24.3535533905933);
#10854=CIRCLE('',#29400,24.);
#10855=CIRCLE('',#29401,24.3535533905933);
#10856=CIRCLE('',#29402,24.);
#10857=CIRCLE('',#29404,24.3535533905933);
#10858=CIRCLE('',#29405,24.3535533905933);
#10859=CIRCLE('',#29406,23.5);
#10860=CIRCLE('',#29408,24.6464466094067);
#10861=CIRCLE('',#29409,24.6464466094067);
#10862=CIRCLE('',#29411,10.);
#10863=CIRCLE('',#29413,23.5);
#10864=CIRCLE('',#29415,23.5);
#10865=CIRCLE('',#29438,25.);
#10866=CIRCLE('',#29439,25.);
#10867=CIRCLE('',#29441,25.);
#10868=CIRCLE('',#29442,25.);
#10869=CIRCLE('',#29484,3.4);
#10870=CIRCLE('',#29485,3.4);
#10871=CIRCLE('',#29494,10.);
#10872=CIRCLE('',#29498,4.925);
#10873=CIRCLE('',#29519,4.0705);
#10874=CIRCLE('',#29521,4.0705);
#10875=CIRCLE('',#29541,4.925);
#10876=CIRCLE('',#29542,4.925);
#10877=CIRCLE('',#29543,4.0705);
#10878=CIRCLE('',#29546,7.60300281800529);
#10879=CIRCLE('',#29551,4.925);
#10880=CIRCLE('',#29557,4.5);
#10881=CIRCLE('',#29562,4.925);
#10882=CIRCLE('',#29583,4.0705);
#10883=CIRCLE('',#29585,4.0705);
#10884=CIRCLE('',#29605,4.925);
#10885=CIRCLE('',#29606,4.925);
#10886=CIRCLE('',#29607,4.0705);
#10887=CIRCLE('',#29611,8.);
#10888=CIRCLE('',#29614,8.);
#10889=CIRCLE('',#29617,8.);
#10890=CIRCLE('',#29620,8.);
#10891=CIRCLE('',#29623,8.);
#10892=CIRCLE('',#29626,8.);
#10893=CIRCLE('',#29629,8.);
#10894=CIRCLE('',#29632,8.);
#10895=CIRCLE('',#29635,8.);
#10896=CIRCLE('',#29638,8.);
#10897=CIRCLE('',#29641,8.);
#10898=CIRCLE('',#29644,8.);
#10899=CIRCLE('',#29647,8.);
#10900=CIRCLE('',#29650,8.);
#10901=CIRCLE('',#29653,8.);
#10902=CIRCLE('',#29656,8.);
#10903=CIRCLE('',#29659,8.);
#10904=CIRCLE('',#29662,8.);
#10905=CIRCLE('',#29665,8.);
#10906=CIRCLE('',#29668,8.);
#10907=CIRCLE('',#29671,8.);
#10908=CIRCLE('',#29674,8.);
#10909=CIRCLE('',#29677,8.);
#10910=CIRCLE('',#29680,8.);
#10911=CIRCLE('',#29683,8.);
#10912=CIRCLE('',#29686,8.);
#10913=CIRCLE('',#29689,8.);
#10914=CIRCLE('',#29692,8.);
#10915=CIRCLE('',#29695,8.);
#10916=CIRCLE('',#29698,8.);
#10917=CIRCLE('',#29701,8.);
#10918=CIRCLE('',#29704,8.);
#10919=CIRCLE('',#29707,8.);
#10920=CIRCLE('',#29710,8.);
#10921=CIRCLE('',#29713,8.);
#10922=CIRCLE('',#29714,8.);
#10923=CIRCLE('',#29717,8.);
#10924=CIRCLE('',#29718,8.);
#10925=CIRCLE('',#29721,8.);
#10926=CIRCLE('',#29724,8.);
#10927=CIRCLE('',#29727,8.);
#10928=CIRCLE('',#29730,8.);
#10929=CIRCLE('',#29733,8.);
#10930=CIRCLE('',#29736,8.);
#10931=CIRCLE('',#29739,8.);
#10932=CIRCLE('',#29742,8.);
#10933=CIRCLE('',#29745,8.);
#10934=CIRCLE('',#29748,8.);
#10935=CIRCLE('',#29751,8.);
#10936=CIRCLE('',#29754,8.);
#10937=CIRCLE('',#29757,8.);
#10938=CIRCLE('',#29760,8.);
#10939=CIRCLE('',#29763,8.);
#10940=CIRCLE('',#29766,8.);
#10941=CIRCLE('',#29769,8.);
#10942=CIRCLE('',#29772,8.);
#10943=CIRCLE('',#29775,8.);
#10944=CIRCLE('',#29778,8.);
#10945=CIRCLE('',#29781,8.);
#10946=CIRCLE('',#29784,8.);
#10947=CIRCLE('',#29787,8.);
#10948=CIRCLE('',#29790,8.);
#10949=CIRCLE('',#29793,8.);
#10950=CIRCLE('',#29796,8.);
#10951=CIRCLE('',#29799,8.);
#10952=CIRCLE('',#29802,8.);
#10953=CIRCLE('',#29805,8.);
#10954=CIRCLE('',#29808,8.);
#10955=CIRCLE('',#29811,8.);
#10956=CIRCLE('',#29814,8.);
#10957=CIRCLE('',#29817,8.);
#10958=CIRCLE('',#29820,8.);
#10959=CIRCLE('',#29823,8.);
#10960=CIRCLE('',#29826,8.);
#10961=CIRCLE('',#29835,4.5);
#10962=CIRCLE('',#29838,4.925);
#10963=CIRCLE('',#29840,8.);
#10964=CIRCLE('',#29842,8.);
#10965=CIRCLE('',#29844,7.5);
#10966=CIRCLE('',#29883,6.85);
#10967=CIRCLE('',#29888,6.35);
#10968=CIRCLE('',#29890,6.85);
#10969=CIRCLE('',#29894,2.4505);
#10970=CIRCLE('',#29907,2.4505);
#10971=CIRCLE('',#29909,1.99475);
#10972=CIRCLE('',#29922,2.4505);
#10973=CIRCLE('',#29923,2.4505);
#10974=CIRCLE('',#29924,1.99475);
#10975=CIRCLE('',#29934,2.2);
#10976=CIRCLE('',#29937,2.4505);
#10977=CIRCLE('',#29939,4.75);
#10978=B_SPLINE_CURVE_WITH_KNOTS('',3,(#37380,#37381,#37382,#37383,#37384,
#37385),.UNSPECIFIED.,.F.,.F.,(4,2,4),(0.,0.0698759495705014,0.100813530301716),
 .UNSPECIFIED.);
#10979=B_SPLINE_CURVE_WITH_KNOTS('',3,(#37394,#37395,#37396,#37397,#37398,
#37399,#37400,#37401,#37402,#37403,#37404,#37405,#37406,#37407,#37408,#37409,
#37410,#37411),.UNSPECIFIED.,.F.,.F.,(4,2,2,2,2,2,2,2,4),(0.229981338184207,
0.230186209246776,0.230825449288754,0.23191142362845,0.236130991491961,
0.265789540903692,0.330613311085503,0.427893531851159,0.499880951546163),
 .UNSPECIFIED.);
#10980=B_SPLINE_CURVE_WITH_KNOTS('',3,(#37421,#37422,#37423,#37424,#37425,
#37426,#37427,#37428,#37429,#37430),.UNSPECIFIED.,.F.,.F.,(4,2,2,2,4),(-0.959890977249723,
-0.705434126471362,-0.450977275693002,-0.225488637846501,0.),
 .UNSPECIFIED.);
#10981=B_SPLINE_CURVE_WITH_KNOTS('',3,(#37434,#37435,#37436,#37437,#37438,
#37439,#37440,#37441,#37442,#37443),.UNSPECIFIED.,.F.,.F.,(4,2,2,2,4),(0.,
0.225488637846501,0.450977275693002,0.705434126471363,0.959890977249723),
 .UNSPECIFIED.);
#10982=B_SPLINE_CURVE_WITH_KNOTS('',3,(#37447,#37448,#37449,#37450,#37451,
#37452,#37453,#37454,#37455,#37456),.UNSPECIFIED.,.F.,.F.,(4,2,2,2,4),(0.944884480326527,
1.19934133110489,1.45379818188325,1.67928681972975,1.90477545757625),
 .UNSPECIFIED.);
#10983=B_SPLINE_CURVE_WITH_KNOTS('',3,(#37460,#37461,#37462,#37463,#37464,
#37465,#37466,#37467,#37468,#37469),.UNSPECIFIED.,.F.,.F.,(4,2,2,2,4),(1.9047986617354,
2.1302872995819,2.35577593742841,2.61023278820676,2.86468963898512),
 .UNSPECIFIED.);
#10984=B_SPLINE_CURVE_WITH_KNOTS('',3,(#37473,#37474,#37475,#37476,#37477,
#37478,#37479,#37480,#37481,#37482),.UNSPECIFIED.,.F.,.F.,(4,2,2,2,4),(-0.33267099144991,
-0.240960064975725,-0.149249138501539,-0.0746245692507697,0.),
 .UNSPECIFIED.);
#10985=B_SPLINE_CURVE_WITH_KNOTS('',3,(#37485,#37486,#37487,#37488,#37489,
#37490),.UNSPECIFIED.,.F.,.F.,(4,2,4),(0.668371667822993,0.742996237073762,
0.770694061397097),.UNSPECIFIED.);
#10986=B_SPLINE_CURVE_WITH_KNOTS('',3,(#37942,#37943,#37944,#37945,#37946,
#37947,#37948,#37949,#37950,#37951),.UNSPECIFIED.,.F.,.F.,(4,2,2,2,4),(0.,
0.0753377480935412,0.150675496187082,0.226025649710019,0.301375803232956),
 .UNSPECIFIED.);
#10987=B_SPLINE_CURVE_WITH_KNOTS('',3,(#37955,#37956,#37957,#37958,#37959,
#37960,#37961,#37962,#37963,#37964),.UNSPECIFIED.,.F.,.F.,(4,2,2,2,4),(-0.301375803232957,
-0.226025649710019,-0.150675496187082,-0.0753377480935411,0.),
 .UNSPECIFIED.);
#10988=B_SPLINE_CURVE_WITH_KNOTS('',3,(#37987,#37988,#37989,#37990,#37991,
#37992,#37993,#37994,#37995,#37996,#37997,#37998,#37999,#38000),
 .UNSPECIFIED.,.F.,.F.,(4,2,2,2,2,2,4),(-0.00091047155368565,0.,0.0913567345993141,
0.177776562764162,0.263923329391251,0.328582398254389,0.38525018680505),
 .UNSPECIFIED.);
#10989=B_SPLINE_CURVE_WITH_KNOTS('',3,(#38004,#38005,#38006,#38007,#38008,
#38009,#38010,#38011,#38012,#38013,#38014,#38015,#38016,#38017),
 .UNSPECIFIED.,.F.,.F.,(4,2,2,2,2,2,4),(-0.771410845200401,-0.770500373646599,
-0.679143639043445,-0.592723810874369,-0.506577044243045,-0.441917975376721,
-0.38525018682332),.UNSPECIFIED.);
#10990=B_SPLINE_CURVE_WITH_KNOTS('',3,(#38092,#38093,#38094,#38095,#38096,
#38097,#38098,#38099),.UNSPECIFIED.,.F.,.F.,(4,1,1,1,1,4),(-1.86233569221144,
-1.59628773618123,-1.06419182412082,-0.798143868090616,-0.532095912060411,
0.),.UNSPECIFIED.);
#10991=B_SPLINE_CURVE_WITH_KNOTS('',3,(#38100,#38101,#38102,#38103,#38104,
#38105,#38106,#38107),.UNSPECIFIED.,.F.,.F.,(4,1,1,1,1,4),(0.,0.532095912060411,
0.798143868090616,1.06419182412082,1.59628773618123,1.86233569221144),
 .UNSPECIFIED.);
#10992=B_SPLINE_CURVE_WITH_KNOTS('',3,(#38162,#38163,#38164,#38165,#38166,
#38167,#38168,#38169),.UNSPECIFIED.,.F.,.F.,(4,1,1,1,1,4),(-1.8623356922078,
-1.33023978014843,-1.06419182411875,-0.798143868089059,-0.532095912059373,
-8.87358627225765E-17),.UNSPECIFIED.);
#10993=B_SPLINE_CURVE_WITH_KNOTS('',3,(#38170,#38171,#38172,#38173,#38174,
#38175,#38176,#38177),.UNSPECIFIED.,.F.,.F.,(4,1,1,1,1,4),(8.87358627225765E-17,
0.532095912059373,0.798143868089059,1.06419182411875,1.33023978014843,1.8623356922078),
 .UNSPECIFIED.);
#10994=B_SPLINE_CURVE_WITH_KNOTS('',3,(#38231,#38232,#38233,#38234,#38235,
#38236,#38237,#38238,#38239),.UNSPECIFIED.,.F.,.F.,(4,1,1,1,1,1,4),(-1.86233569221144,
-1.46326375816613,-1.33023978015103,-1.06419182412082,-0.798143868090615,
-0.266047956030205,0.),.UNSPECIFIED.);
#10995=B_SPLINE_CURVE_WITH_KNOTS('',3,(#38369,#38370,#38371,#38372,#38373,
#38374,#38375,#38376,#38377),.UNSPECIFIED.,.F.,.F.,(4,1,1,1,1,1,4),(0.,
0.266047956030205,0.798143868090615,1.06419182412082,1.33023978015103,1.46326375816613,
1.86233569221144),.UNSPECIFIED.);
#10996=B_SPLINE_CURVE_WITH_KNOTS('',3,(#38432,#38433,#38434,#38435,#38436,
#38437,#38438,#38439),.UNSPECIFIED.,.F.,.F.,(4,1,1,1,1,4),(-1.86233569220781,
-1.59628773617812,-1.06419182411875,-0.79814386808906,-0.532095912059373,
-2.59005157847017E-16),.UNSPECIFIED.);
#10997=B_SPLINE_CURVE_WITH_KNOTS('',3,(#38440,#38441,#38442,#38443,#38444,
#38445,#38446,#38447),.UNSPECIFIED.,.F.,.F.,(4,1,1,1,1,4),(2.59005157847017E-16,
0.532095912059373,0.79814386808906,1.06419182411875,1.59628773617812,1.86233569220781),
 .UNSPECIFIED.);
#10998=B_SPLINE_CURVE_WITH_KNOTS('',3,(#38612,#38613,#38614,#38615,#38616,
#38617,#38618,#38619,#38620,#38621,#38622,#38623,#38624,#38625,#38626,#38627,
#38628,#38629,#38630,#38631,#38632,#38633,#38634,#38635,#38636,#38637,#38638,
#38639,#38640,#38641,#38642,#38643,#38644,#38645,#38646,#38647,#38648,#38649,
#38650,#38651,#38652,#38653,#38654,#38655,#38656,#38657,#38658,#38659,#38660,
#38661,#38662,#38663,#38664,#38665,#38666),.UNSPECIFIED.,.F.,.F.,(4,3,3,
3,3,3,3,3,3,3,3,3,3,3,3,3,3,3,4),(0.,0.0454718630240152,0.0931953780618431,
0.144039899826263,0.200168007591155,0.270586701894521,0.345292422602525,
0.401891619293991,0.452964632778209,0.503347839957264,0.552485563146028,
0.605298848841166,0.665634056699999,0.749225542524999,0.811919156893749,
0.864445081091848,0.913828865901365,0.959856605634592,1.),.UNSPECIFIED.);
#10999=B_SPLINE_CURVE_WITH_KNOTS('',3,(#38668,#38669,#38670,#38671),
 .UNSPECIFIED.,.F.,.F.,(4,4),(0.,1.),.UNSPECIFIED.);
#11000=B_SPLINE_CURVE_WITH_KNOTS('',3,(#38673,#38674,#38675,#38676,#38677,
#38678,#38679,#38680,#38681,#38682,#38683,#38684,#38685,#38686,#38687,#38688,
#38689,#38690,#38691,#38692,#38693,#38694,#38695,#38696,#38697,#38698,#38699,
#38700,#38701,#38702,#38703,#38704,#38705,#38706,#38707,#38708,#38709,#38710,
#38711,#38712,#38713,#38714,#38715,#38716,#38717,#38718,#38719,#38720,#38721,
#38722,#38723,#38724,#38725,#38726,#38727),.UNSPECIFIED.,.F.,.F.,(4,3,3,
3,3,3,3,3,3,3,3,3,3,3,3,3,3,3,4),(0.,0.0454743571758764,0.0932006890496627,
0.144048574957221,0.200181673047881,0.270614812390671,0.345307027643352,
0.401906381576288,0.452980318796474,0.503379519506409,0.552517196305072,
0.605331277143381,0.665671120969662,0.749253340727247,0.811940005545435,
0.864461351673187,0.913841478931383,0.959866376897951,1.),.UNSPECIFIED.);
#11001=B_SPLINE_CURVE_WITH_KNOTS('',3,(#38754,#38755,#38756,#38757,#38758,
#38759),.UNSPECIFIED.,.F.,.F.,(4,1,1,4),(-1.75610615531806,-1.00348923161032,
-0.501744615805159,2.22044604925036E-16),.UNSPECIFIED.);
#11002=B_SPLINE_CURVE_WITH_KNOTS('',3,(#38762,#38763,#38764,#38765,#38766,
#38767),.UNSPECIFIED.,.F.,.F.,(4,1,1,4),(-2.22044604925036E-16,0.501744615805159,
1.00348923161032,1.75610615531806),.UNSPECIFIED.);
#11003=B_SPLINE_CURVE_WITH_KNOTS('',3,(#38790,#38791,#38792,#38793,#38794,
#38795,#38796),.UNSPECIFIED.,.F.,.F.,(4,1,1,1,4),(-1.75610615531806,-1.2543615395129,
-0.752616923707738,-0.501744615805159,4.16333634234434E-16),
 .UNSPECIFIED.);
#11004=B_SPLINE_CURVE_WITH_KNOTS('',3,(#38797,#38798,#38799,#38800,#38801,
#38802,#38803,#38804,#38805,#38806,#38807,#38808,#38809,#38810,#38811,#38812,
#38813,#38814,#38815,#38816,#38817,#38818,#38819,#38820,#38821,#38822,#38823,
#38824,#38825,#38826,#38827,#38828,#38829,#38830,#38831,#38832,#38833,#38834,
#38835,#38836,#38837,#38838,#38839,#38840,#38841,#38842,#38843,#38844,#38845,
#38846,#38847,#38848,#38849,#38850,#38851),.UNSPECIFIED.,.F.,.F.,(4,3,3,
3,3,3,3,3,3,3,3,3,3,3,3,3,3,3,4),(0.,0.0454718630244078,0.093195378062645,
0.144039899827185,0.200168007593219,0.270586701897487,0.345292422601172,
0.401891619293172,0.452964632777252,0.503347839955838,0.552485563143815,
0.605298848838466,0.665634056695191,0.749225542521393,0.811919156891045,
0.864445081089156,0.913828865898862,0.959856605632137,1.),.UNSPECIFIED.);
#11005=B_SPLINE_CURVE_WITH_KNOTS('',3,(#38881,#38882,#38883,#38884),
 .UNSPECIFIED.,.F.,.F.,(4,4),(0.,1.),.UNSPECIFIED.);
#11006=B_SPLINE_CURVE_WITH_KNOTS('',3,(#38885,#38886,#38887,#38888,#38889,
#38890,#38891,#38892,#38893,#38894,#38895,#38896,#38897,#38898,#38899,#38900,
#38901,#38902,#38903,#38904,#38905,#38906,#38907,#38908,#38909,#38910,#38911,
#38912,#38913,#38914,#38915,#38916,#38917,#38918,#38919,#38920,#38921,#38922,
#38923,#38924,#38925,#38926,#38927,#38928,#38929,#38930,#38931,#38932,#38933,
#38934,#38935,#38936,#38937,#38938,#38939),.UNSPECIFIED.,.F.,.F.,(4,3,3,
3,3,3,3,3,3,3,3,3,3,3,3,3,3,3,4),(0.,0.0454743571757827,0.0932006890496455,
0.144048574957222,0.200181673048135,0.270614812391146,0.345307027643342,
0.401906381576231,0.452980318796516,0.503379519506306,0.552517196304985,
0.60533127714324,0.665671120969617,0.749253340727213,0.81194000554541,0.86446135167315,
0.913841478931319,0.959866376897937,1.),.UNSPECIFIED.);
#11007=B_SPLINE_CURVE_WITH_KNOTS('',3,(#38970,#38971,#38972,#38973,#38974,
#38975,#38976),.UNSPECIFIED.,.F.,.F.,(4,1,1,1,4),(-4.16333634234434E-16,
0.501744615805159,0.752616923707738,1.2543615395129,1.75610615531806),
 .UNSPECIFIED.);
#11008=B_SPLINE_CURVE_WITH_KNOTS('',3,(#38984,#38985,#38986,#38987,#38988,
#38989,#38990,#38991,#38992,#38993),.UNSPECIFIED.,.F.,.F.,(4,2,2,2,4),(-0.226321012475095,
-0.169664342772315,-0.113007673069535,-0.0565038365347675,0.),
 .UNSPECIFIED.);
#11009=B_SPLINE_CURVE_WITH_KNOTS('',3,(#39024,#39025,#39026,#39027,#39028,
#39029,#39030,#39031,#39032,#39033,#39034,#39035,#39036,#39037,#39038,#39039,
#39040,#39041,#39042,#39043,#39044,#39045,#39046,#39047,#39048,#39049,#39050,
#39051,#39052,#39053,#39054,#39055,#39056,#39057,#39058,#39059,#39060,#39061,
#39062,#39063,#39064,#39065,#39066,#39067,#39068,#39069,#39070,#39071,#39072,
#39073,#39074,#39075,#39076,#39077,#39078),.UNSPECIFIED.,.F.,.F.,(4,3,3,
3,3,3,3,3,3,3,3,3,3,3,3,3,3,3,4),(0.,0.0454718630245446,0.0931953780629266,
0.144039899826871,0.200168007592049,0.270586701894404,0.345292422600176,
0.401891619292783,0.452964632776678,0.503347839955005,0.552485563142855,
0.605298848838406,0.665634056694974,0.749225542521231,0.811919156890923,
0.864445081089191,0.913828865898807,0.959856605631954,1.),.UNSPECIFIED.);
#11010=B_SPLINE_CURVE_WITH_KNOTS('',3,(#39080,#39081,#39082,#39083),
 .UNSPECIFIED.,.F.,.F.,(4,4),(0.,1.),.UNSPECIFIED.);
#11011=B_SPLINE_CURVE_WITH_KNOTS('',3,(#39085,#39086,#39087,#39088,#39089,
#39090,#39091,#39092,#39093,#39094,#39095,#39096,#39097,#39098,#39099,#39100,
#39101,#39102,#39103,#39104,#39105,#39106,#39107,#39108,#39109,#39110,#39111,
#39112,#39113,#39114,#39115,#39116,#39117,#39118,#39119,#39120,#39121,#39122,
#39123,#39124,#39125,#39126,#39127,#39128,#39129,#39130,#39131,#39132,#39133,
#39134,#39135,#39136,#39137,#39138,#39139),.UNSPECIFIED.,.F.,.F.,(4,3,3,
3,3,3,3,3,3,3,3,3,3,3,3,3,3,3,4),(0.,0.0454743571758869,0.0932006890496471,
0.144048574957122,0.200181673047726,0.270614812390508,0.345307027643179,
0.401906381576174,0.452980318796373,0.50337951950626,0.55251719630495,0.605331277143244,
0.665671120969541,0.749253340727156,0.811940005545367,0.864461351673143,
0.913841478931369,0.959866376897944,1.),.UNSPECIFIED.);
#11012=B_SPLINE_CURVE_WITH_KNOTS('',3,(#39166,#39167,#39168,#39169,#39170,
#39171),.UNSPECIFIED.,.F.,.F.,(4,1,1,4),(-1.75610615531806,-1.00348923161032,
-0.501744615805159,2.77555756156289E-17),.UNSPECIFIED.);
#11013=B_SPLINE_CURVE_WITH_KNOTS('',3,(#39174,#39175,#39176,#39177,#39178,
#39179),.UNSPECIFIED.,.F.,.F.,(4,1,1,4),(-2.77555756156289E-17,0.501744615805159,
1.00348923161032,1.75610615531806),.UNSPECIFIED.);
#11014=B_SPLINE_CURVE_WITH_KNOTS('',3,(#39228,#39229,#39230,#39231,#39232,
#39233,#39234,#39235,#39236,#39237,#39238,#39239,#39240,#39241,#39242,#39243,
#39244,#39245,#39246,#39247,#39248,#39249,#39250,#39251,#39252,#39253,#39254,
#39255,#39256,#39257,#39258,#39259,#39260,#39261,#39262,#39263,#39264,#39265,
#39266,#39267,#39268,#39269,#39270,#39271,#39272,#39273,#39274,#39275,#39276,
#39277,#39278,#39279,#39280,#39281,#39282),.UNSPECIFIED.,.F.,.F.,(4,3,3,
3,3,3,3,3,3,3,3,3,3,3,3,3,3,3,4),(0.,0.0454718630245446,0.0931953780629266,
0.144039899826871,0.200168007592049,0.270586701894404,0.345292422600176,
0.401891619292783,0.452964632776678,0.503347839955005,0.552485563142855,
0.605298848838406,0.665634056694974,0.749225542521231,0.811919156890923,
0.864445081089191,0.913828865898807,0.959856605631954,1.),.UNSPECIFIED.);
#11015=B_SPLINE_CURVE_WITH_KNOTS('',3,(#39284,#39285,#39286,#39287),
 .UNSPECIFIED.,.F.,.F.,(4,4),(0.,1.),.UNSPECIFIED.);
#11016=B_SPLINE_CURVE_WITH_KNOTS('',3,(#39289,#39290,#39291,#39292,#39293,
#39294,#39295,#39296,#39297,#39298,#39299,#39300,#39301,#39302,#39303,#39304,
#39305,#39306,#39307,#39308,#39309,#39310,#39311,#39312,#39313,#39314,#39315,
#39316,#39317,#39318,#39319,#39320,#39321,#39322,#39323,#39324,#39325,#39326,
#39327,#39328,#39329,#39330,#39331,#39332,#39333,#39334,#39335,#39336,#39337,
#39338,#39339,#39340,#39341,#39342,#39343),.UNSPECIFIED.,.F.,.F.,(4,3,3,
3,3,3,3,3,3,3,3,3,3,3,3,3,3,3,4),(0.,0.0454743571758869,0.0932006890496471,
0.144048574957122,0.200181673047726,0.270614812390508,0.345307027643179,
0.401906381576174,0.452980318796373,0.50337951950626,0.55251719630495,0.605331277143244,
0.665671120969541,0.749253340727156,0.811940005545367,0.864461351673143,
0.913841478931369,0.959866376897944,1.),.UNSPECIFIED.);
#11017=B_SPLINE_CURVE_WITH_KNOTS('',3,(#39370,#39371,#39372,#39373,#39374,
#39375),.UNSPECIFIED.,.F.,.F.,(4,1,1,4),(-1.75610615531806,-1.00348923161032,
-0.501744615805159,2.77555756156289E-17),.UNSPECIFIED.);
#11018=B_SPLINE_CURVE_WITH_KNOTS('',3,(#39378,#39379,#39380,#39381,#39382,
#39383),.UNSPECIFIED.,.F.,.F.,(4,1,1,4),(-2.77555756156289E-17,0.501744615805159,
1.00348923161032,1.75610615531806),.UNSPECIFIED.);
#11019=B_SPLINE_CURVE_WITH_KNOTS('',3,(#39404,#39405,#39406,#39407,#39408,
#39409),.UNSPECIFIED.,.F.,.F.,(4,1,1,4),(-1.75610615531806,-1.00348923161032,
-0.501744615805159,1.27116549159798E-31),.UNSPECIFIED.);
#11020=B_SPLINE_CURVE_WITH_KNOTS('',3,(#39410,#39411,#39412,#39413,#39414,
#39415,#39416,#39417,#39418,#39419,#39420,#39421,#39422,#39423,#39424,#39425,
#39426,#39427,#39428,#39429,#39430,#39431,#39432,#39433,#39434,#39435,#39436,
#39437,#39438,#39439,#39440,#39441,#39442,#39443,#39444,#39445,#39446,#39447,
#39448,#39449,#39450,#39451,#39452,#39453,#39454,#39455,#39456,#39457,#39458,
#39459,#39460,#39461,#39462,#39463,#39464),.UNSPECIFIED.,.F.,.F.,(4,3,3,
3,3,3,3,3,3,3,3,3,3,3,3,3,3,3,4),(0.,0.0454718630242959,0.0931953780625046,
0.144039899827041,0.200168007592975,0.270586701897097,0.345292422601312,
0.401891619293206,0.452964632777226,0.503347839955808,0.552485563143695,
0.60529884883852,0.665634056695758,0.749225542521819,0.811919156891364,
0.864445081089579,0.913828865899227,0.959856605632539,1.),.UNSPECIFIED.);
#11021=B_SPLINE_CURVE_WITH_KNOTS('',3,(#39494,#39495,#39496,#39497),
 .UNSPECIFIED.,.F.,.F.,(4,4),(0.,1.),.UNSPECIFIED.);
#11022=B_SPLINE_CURVE_WITH_KNOTS('',3,(#39498,#39499,#39500,#39501,#39502,
#39503,#39504,#39505,#39506,#39507,#39508,#39509,#39510,#39511,#39512,#39513,
#39514,#39515,#39516,#39517,#39518,#39519,#39520,#39521,#39522,#39523,#39524,
#39525,#39526,#39527,#39528,#39529,#39530,#39531,#39532,#39533,#39534,#39535,
#39536,#39537,#39538,#39539,#39540,#39541,#39542,#39543,#39544,#39545,#39546,
#39547,#39548,#39549,#39550,#39551,#39552),.UNSPECIFIED.,.F.,.F.,(4,3,3,
3,3,3,3,3,3,3,3,3,3,3,3,3,3,3,4),(0.,0.0454743571758223,0.0932006890496185,
0.144048574957236,0.200181673047968,0.270614812390343,0.34530702764307,
0.401906381576014,0.452980318796357,0.503379519506187,0.552517196304828,
0.605331277143297,0.665671120969503,0.749253340727127,0.811940005545345,
0.864461351673149,0.913841478931467,0.959866376898016,1.),.UNSPECIFIED.);
#11023=B_SPLINE_CURVE_WITH_KNOTS('',3,(#39579,#39580,#39581,#39582,#39583,
#39584),.UNSPECIFIED.,.F.,.F.,(4,1,1,4),(-1.27116549159798E-31,0.501744615805159,
1.00348923161032,1.75610615531806),.UNSPECIFIED.);
#11024=B_SPLINE_CURVE_WITH_KNOTS('',3,(#39592,#39593,#39594,#39595,#39596,
#39597,#39598,#39599,#39600,#39601),.UNSPECIFIED.,.F.,.F.,(4,2,2,2,4),(-0.226321012475095,
-0.169664342772315,-0.113007673069535,-0.0565038365347675,0.),
 .UNSPECIFIED.);
#11025=B_SPLINE_CURVE_WITH_KNOTS('',3,(#39632,#39633,#39634,#39635,#39636,
#39637,#39638,#39639,#39640,#39641,#39642,#39643,#39644,#39645,#39646,#39647,
#39648,#39649,#39650,#39651,#39652,#39653,#39654,#39655,#39656,#39657,#39658,
#39659,#39660,#39661,#39662,#39663,#39664,#39665,#39666,#39667,#39668,#39669,
#39670,#39671,#39672,#39673,#39674,#39675,#39676,#39677,#39678,#39679,#39680,
#39681,#39682,#39683,#39684,#39685,#39686),.UNSPECIFIED.,.F.,.F.,(4,3,3,
3,3,3,3,3,3,3,3,3,3,3,3,3,3,3,4),(0.,0.045471863024028,0.0931953780617352,
0.144039899826522,0.200168007592056,0.270586701896401,0.345292422600315,
0.401891619292387,0.452964632776744,0.503347839957351,0.552485563145081,
0.605298848840994,0.665634056697722,0.749225542523292,0.811919156892469,
0.864445081090302,0.913828865899915,0.959856605633197,1.),.UNSPECIFIED.);
#11026=B_SPLINE_CURVE_WITH_KNOTS('',3,(#39688,#39689,#39690,#39691),
 .UNSPECIFIED.,.F.,.F.,(4,4),(0.,1.),.UNSPECIFIED.);
#11027=B_SPLINE_CURVE_WITH_KNOTS('',3,(#39693,#39694,#39695,#39696,#39697,
#39698,#39699,#39700,#39701,#39702,#39703,#39704,#39705,#39706,#39707,#39708,
#39709,#39710,#39711,#39712,#39713,#39714,#39715,#39716,#39717,#39718,#39719,
#39720,#39721,#39722,#39723,#39724,#39725,#39726,#39727,#39728,#39729,#39730,
#39731,#39732,#39733,#39734,#39735,#39736,#39737,#39738,#39739,#39740,#39741,
#39742,#39743,#39744,#39745,#39746,#39747),.UNSPECIFIED.,.F.,.F.,(4,3,3,
3,3,3,3,3,3,3,3,3,3,3,3,3,3,3,4),(0.,0.0454743571758992,0.0932006890496849,
0.144048574957235,0.200181673047928,0.270614812390673,0.345307027643151,
0.401906381576126,0.452980318796356,0.503379519506263,0.552517196304882,
0.605331277143196,0.665671120969352,0.749253340727014,0.811940005545261,
0.864461351673037,0.913841478931272,0.959866376897846,1.),.UNSPECIFIED.);
#11028=B_SPLINE_CURVE_WITH_KNOTS('',3,(#39778,#39779,#39780,#39781,#39782,
#39783,#39784),.UNSPECIFIED.,.F.,.F.,(4,1,1,1,4),(-1.75610615531805,-1.25436153951289,
-0.752616923707736,-0.501744615805158,1.11022302462516E-16),
 .UNSPECIFIED.);
#11029=B_SPLINE_CURVE_WITH_KNOTS('',3,(#39787,#39788,#39789,#39790,#39791,
#39792,#39793),.UNSPECIFIED.,.F.,.F.,(4,1,1,1,4),(-1.11022302462516E-16,
0.501744615805158,0.752616923707736,1.25436153951289,1.75610615531805),
 .UNSPECIFIED.);
#11030=B_SPLINE_CURVE_WITH_KNOTS('',3,(#39814,#39815,#39816,#39817,#39818,
#39819,#39820),.UNSPECIFIED.,.F.,.F.,(4,1,1,1,4),(-1.75610615531806,-1.2543615395129,
-0.752616923707739,-0.501744615805159,4.10679309198325E-32),
 .UNSPECIFIED.);
#11031=B_SPLINE_CURVE_WITH_KNOTS('',3,(#39821,#39822,#39823,#39824,#39825,
#39826,#39827,#39828,#39829,#39830,#39831,#39832,#39833,#39834,#39835,#39836,
#39837,#39838,#39839,#39840,#39841,#39842,#39843,#39844,#39845,#39846,#39847,
#39848,#39849,#39850,#39851,#39852,#39853,#39854,#39855,#39856,#39857,#39858,
#39859,#39860,#39861,#39862,#39863,#39864,#39865,#39866,#39867,#39868,#39869,
#39870,#39871,#39872,#39873,#39874,#39875),.UNSPECIFIED.,.F.,.F.,(4,3,3,
3,3,3,3,3,3,3,3,3,3,3,3,3,3,3,4),(0.,0.0454718630243362,0.0931953780625649,
0.144039899826463,0.200168007592413,0.27058670189605,0.345292422599966,
0.401891619292168,0.452964632776254,0.503347839954095,0.552485563141883,
0.605298848836136,0.665634056692691,0.749225542519518,0.811919156889639,
0.864445081087949,0.913828865897587,0.959856605630922,1.),.UNSPECIFIED.);
#11032=B_SPLINE_CURVE_WITH_KNOTS('',3,(#39905,#39906,#39907,#39908),
 .UNSPECIFIED.,.F.,.F.,(4,4),(0.,1.),.UNSPECIFIED.);
#11033=B_SPLINE_CURVE_WITH_KNOTS('',3,(#39909,#39910,#39911,#39912,#39913,
#39914,#39915,#39916,#39917,#39918,#39919,#39920,#39921,#39922,#39923,#39924,
#39925,#39926,#39927,#39928,#39929,#39930,#39931,#39932,#39933,#39934,#39935,
#39936,#39937,#39938,#39939,#39940,#39941,#39942,#39943,#39944,#39945,#39946,
#39947,#39948,#39949,#39950,#39951,#39952,#39953,#39954,#39955,#39956,#39957,
#39958,#39959,#39960,#39961,#39962,#39963),.UNSPECIFIED.,.F.,.F.,(4,3,3,
3,3,3,3,3,3,3,3,3,3,3,3,3,3,3,4),(0.,0.0454743571757403,0.0932006890494696,
0.144048574956973,0.200181673047506,0.270614812390275,0.345307027643286,
0.401906381576242,0.452980318796464,0.503379519506601,0.552517196305261,
0.605331277143663,0.665671120969907,0.74925334072743,0.811940005545573,
0.864461351673319,0.91384147893155,0.95986637689812,1.),.UNSPECIFIED.);
#11034=B_SPLINE_CURVE_WITH_KNOTS('',3,(#39994,#39995,#39996,#39997,#39998,
#39999,#40000),.UNSPECIFIED.,.F.,.F.,(4,1,1,1,4),(-4.10679309198325E-32,
0.501744615805159,0.752616923707739,1.2543615395129,1.75610615531806),
 .UNSPECIFIED.);
#11035=B_SPLINE_CURVE_WITH_KNOTS('',3,(#40008,#40009,#40010,#40011,#40012,
#40013,#40014,#40015,#40016,#40017),.UNSPECIFIED.,.F.,.F.,(4,2,2,2,4),(-0.226321012475095,
-0.169664342772315,-0.113007673069535,-0.0565038365347676,0.),
 .UNSPECIFIED.);
#11036=B_SPLINE_CURVE_WITH_KNOTS('',3,(#40075,#40076,#40077,#40078,#40079,
#40080,#40081,#40082,#40083,#40084),.UNSPECIFIED.,.F.,.F.,(4,2,2,2,4),(0.,
0.0565038365347675,0.113007673069535,0.169664342772315,0.226321012475095),
 .UNSPECIFIED.);
#11037=B_SPLINE_CURVE_WITH_KNOTS('',3,(#40090,#40091,#40092,#40093,#40094,
#40095,#40096,#40097,#40098,#40099),.UNSPECIFIED.,.F.,.F.,(4,2,2,2,4),(0.,
0.0565038365347674,0.113007673069535,0.169664342772315,0.226321012475095),
 .UNSPECIFIED.);
#11038=B_SPLINE_CURVE_WITH_KNOTS('',2,(#40171,#40172,#40173),
 .UNSPECIFIED.,.F.,.F.,(3,3),(0.,1.),.UNSPECIFIED.);
#11039=B_SPLINE_CURVE_WITH_KNOTS('',2,(#40175,#40176,#40177),
 .UNSPECIFIED.,.F.,.F.,(3,3),(0.,1.),.UNSPECIFIED.);
#11040=B_SPLINE_CURVE_WITH_KNOTS('',2,(#40179,#40180,#40181),
 .UNSPECIFIED.,.F.,.F.,(3,3),(0.,1.),.UNSPECIFIED.);
#11041=B_SPLINE_CURVE_WITH_KNOTS('',2,(#40185,#40186,#40187),
 .UNSPECIFIED.,.F.,.F.,(3,3),(0.,1.),.UNSPECIFIED.);
#11042=B_SPLINE_CURVE_WITH_KNOTS('',2,(#40189,#40190,#40191),
 .UNSPECIFIED.,.F.,.F.,(3,3),(0.,1.),.UNSPECIFIED.);
#11043=B_SPLINE_CURVE_WITH_KNOTS('',2,(#40193,#40194,#40195),
 .UNSPECIFIED.,.F.,.F.,(3,3),(0.,1.),.UNSPECIFIED.);
#11044=B_SPLINE_CURVE_WITH_KNOTS('',2,(#40197,#40198,#40199),
 .UNSPECIFIED.,.F.,.F.,(3,3),(0.,1.),.UNSPECIFIED.);
#11045=B_SPLINE_CURVE_WITH_KNOTS('',2,(#40201,#40202,#40203),
 .UNSPECIFIED.,.F.,.F.,(3,3),(0.,1.),.UNSPECIFIED.);
#11046=B_SPLINE_CURVE_WITH_KNOTS('',2,(#40205,#40206,#40207),
 .UNSPECIFIED.,.F.,.F.,(3,3),(0.,1.),.UNSPECIFIED.);
#11047=B_SPLINE_CURVE_WITH_KNOTS('',2,(#40209,#40210,#40211),
 .UNSPECIFIED.,.F.,.F.,(3,3),(0.,1.),.UNSPECIFIED.);
#11048=B_SPLINE_CURVE_WITH_KNOTS('',2,(#40213,#40214,#40215),
 .UNSPECIFIED.,.F.,.F.,(3,3),(0.,1.),.UNSPECIFIED.);
#11049=B_SPLINE_CURVE_WITH_KNOTS('',2,(#40217,#40218,#40219),
 .UNSPECIFIED.,.F.,.F.,(3,3),(0.,1.),.UNSPECIFIED.);
#11050=B_SPLINE_CURVE_WITH_KNOTS('',2,(#40221,#40222,#40223),
 .UNSPECIFIED.,.F.,.F.,(3,3),(0.,1.),.UNSPECIFIED.);
#11051=B_SPLINE_CURVE_WITH_KNOTS('',2,(#40225,#40226,#40227),
 .UNSPECIFIED.,.F.,.F.,(3,3),(0.,1.),.UNSPECIFIED.);
#11052=B_SPLINE_CURVE_WITH_KNOTS('',2,(#40229,#40230,#40231),
 .UNSPECIFIED.,.F.,.F.,(3,3),(0.,1.),.UNSPECIFIED.);
#11053=B_SPLINE_CURVE_WITH_KNOTS('',2,(#40233,#40234,#40235),
 .UNSPECIFIED.,.F.,.F.,(3,3),(0.,1.),.UNSPECIFIED.);
#11054=B_SPLINE_CURVE_WITH_KNOTS('',2,(#40237,#40238,#40239),
 .UNSPECIFIED.,.F.,.F.,(3,3),(0.,1.),.UNSPECIFIED.);
#11055=B_SPLINE_CURVE_WITH_KNOTS('',2,(#40241,#40242,#40243),
 .UNSPECIFIED.,.F.,.F.,(3,3),(0.,1.),.UNSPECIFIED.);
#11056=B_SPLINE_CURVE_WITH_KNOTS('',2,(#40245,#40246,#40247),
 .UNSPECIFIED.,.F.,.F.,(3,3),(0.,1.),.UNSPECIFIED.);
#11057=B_SPLINE_CURVE_WITH_KNOTS('',2,(#40249,#40250,#40251),
 .UNSPECIFIED.,.F.,.F.,(3,3),(0.,1.),.UNSPECIFIED.);
#11058=B_SPLINE_CURVE_WITH_KNOTS('',2,(#40253,#40254,#40255),
 .UNSPECIFIED.,.F.,.F.,(3,3),(0.,1.),.UNSPECIFIED.);
#11059=B_SPLINE_CURVE_WITH_KNOTS('',2,(#40259,#40260,#40261),
 .UNSPECIFIED.,.F.,.F.,(3,3),(0.,1.),.UNSPECIFIED.);
#11060=B_SPLINE_CURVE_WITH_KNOTS('',2,(#40263,#40264,#40265),
 .UNSPECIFIED.,.F.,.F.,(3,3),(0.,1.),.UNSPECIFIED.);
#11061=B_SPLINE_CURVE_WITH_KNOTS('',2,(#40267,#40268,#40269),
 .UNSPECIFIED.,.F.,.F.,(3,3),(0.,1.),.UNSPECIFIED.);
#11062=B_SPLINE_CURVE_WITH_KNOTS('',2,(#40271,#40272,#40273),
 .UNSPECIFIED.,.F.,.F.,(3,3),(0.,1.),.UNSPECIFIED.);
#11063=B_SPLINE_CURVE_WITH_KNOTS('',2,(#40275,#40276,#40277),
 .UNSPECIFIED.,.F.,.F.,(3,3),(0.,1.),.UNSPECIFIED.);
#11064=B_SPLINE_CURVE_WITH_KNOTS('',2,(#40279,#40280,#40281),
 .UNSPECIFIED.,.F.,.F.,(3,3),(0.,1.),.UNSPECIFIED.);
#11065=B_SPLINE_CURVE_WITH_KNOTS('',2,(#40283,#40284,#40285),
 .UNSPECIFIED.,.F.,.F.,(3,3),(0.,1.),.UNSPECIFIED.);
#11066=B_SPLINE_CURVE_WITH_KNOTS('',2,(#40287,#40288,#40289),
 .UNSPECIFIED.,.F.,.F.,(3,3),(0.,1.),.UNSPECIFIED.);
#11067=B_SPLINE_CURVE_WITH_KNOTS('',2,(#40291,#40292,#40293),
 .UNSPECIFIED.,.F.,.F.,(3,3),(0.,1.),.UNSPECIFIED.);
#11068=B_SPLINE_CURVE_WITH_KNOTS('',2,(#40295,#40296,#40297),
 .UNSPECIFIED.,.F.,.F.,(3,3),(0.,1.),.UNSPECIFIED.);
#11069=B_SPLINE_CURVE_WITH_KNOTS('',2,(#40299,#40300,#40301),
 .UNSPECIFIED.,.F.,.F.,(3,3),(0.,1.),.UNSPECIFIED.);
#11070=B_SPLINE_CURVE_WITH_KNOTS('',2,(#40302,#40303,#40304),
 .UNSPECIFIED.,.F.,.F.,(3,3),(0.,1.),.UNSPECIFIED.);
#11071=B_SPLINE_CURVE_WITH_KNOTS('',2,(#40321,#40322,#40323),
 .UNSPECIFIED.,.F.,.F.,(3,3),(0.,1.),.UNSPECIFIED.);
#11072=B_SPLINE_CURVE_WITH_KNOTS('',2,(#40325,#40326,#40327),
 .UNSPECIFIED.,.F.,.F.,(3,3),(0.,1.),.UNSPECIFIED.);
#11073=B_SPLINE_CURVE_WITH_KNOTS('',2,(#40359,#40360,#40361),
 .UNSPECIFIED.,.F.,.F.,(3,3),(0.,1.),.UNSPECIFIED.);
#11074=B_SPLINE_CURVE_WITH_KNOTS('',2,(#40363,#40364,#40365),
 .UNSPECIFIED.,.F.,.F.,(3,3),(0.,1.),.UNSPECIFIED.);
#11075=B_SPLINE_CURVE_WITH_KNOTS('',2,(#40367,#40368,#40369),
 .UNSPECIFIED.,.F.,.F.,(3,3),(0.,1.),.UNSPECIFIED.);
#11076=B_SPLINE_CURVE_WITH_KNOTS('',2,(#40371,#40372,#40373),
 .UNSPECIFIED.,.F.,.F.,(3,3),(0.,1.),.UNSPECIFIED.);
#11077=B_SPLINE_CURVE_WITH_KNOTS('',2,(#40375,#40376,#40377),
 .UNSPECIFIED.,.F.,.F.,(3,3),(0.,1.),.UNSPECIFIED.);
#11078=B_SPLINE_CURVE_WITH_KNOTS('',2,(#40379,#40380,#40381),
 .UNSPECIFIED.,.F.,.F.,(3,3),(0.,1.),.UNSPECIFIED.);
#11079=B_SPLINE_CURVE_WITH_KNOTS('',2,(#40383,#40384,#40385),
 .UNSPECIFIED.,.F.,.F.,(3,3),(0.,1.),.UNSPECIFIED.);
#11080=B_SPLINE_CURVE_WITH_KNOTS('',2,(#40387,#40388,#40389),
 .UNSPECIFIED.,.F.,.F.,(3,3),(0.,1.),.UNSPECIFIED.);
#11081=B_SPLINE_CURVE_WITH_KNOTS('',2,(#40391,#40392,#40393),
 .UNSPECIFIED.,.F.,.F.,(3,3),(0.,1.),.UNSPECIFIED.);
#11082=B_SPLINE_CURVE_WITH_KNOTS('',2,(#40395,#40396,#40397),
 .UNSPECIFIED.,.F.,.F.,(3,3),(0.,1.),.UNSPECIFIED.);
#11083=B_SPLINE_CURVE_WITH_KNOTS('',2,(#40399,#40400,#40401),
 .UNSPECIFIED.,.F.,.F.,(3,3),(0.,1.),.UNSPECIFIED.);
#11084=B_SPLINE_CURVE_WITH_KNOTS('',2,(#40409,#40410,#40411),
 .UNSPECIFIED.,.F.,.F.,(3,3),(0.,1.),.UNSPECIFIED.);
#11085=B_SPLINE_CURVE_WITH_KNOTS('',2,(#40413,#40414,#40415),
 .UNSPECIFIED.,.F.,.F.,(3,3),(0.,1.),.UNSPECIFIED.);
#11086=B_SPLINE_CURVE_WITH_KNOTS('',2,(#40417,#40418,#40419),
 .UNSPECIFIED.,.F.,.F.,(3,3),(0.,1.),.UNSPECIFIED.);
#11087=B_SPLINE_CURVE_WITH_KNOTS('',2,(#40421,#40422,#40423),
 .UNSPECIFIED.,.F.,.F.,(3,3),(0.,1.),.UNSPECIFIED.);
#11088=B_SPLINE_CURVE_WITH_KNOTS('',2,(#40425,#40426,#40427),
 .UNSPECIFIED.,.F.,.F.,(3,3),(0.,1.),.UNSPECIFIED.);
#11089=B_SPLINE_CURVE_WITH_KNOTS('',2,(#40429,#40430,#40431),
 .UNSPECIFIED.,.F.,.F.,(3,3),(0.,1.),.UNSPECIFIED.);
#11090=B_SPLINE_CURVE_WITH_KNOTS('',2,(#40433,#40434,#40435),
 .UNSPECIFIED.,.F.,.F.,(3,3),(0.,1.),.UNSPECIFIED.);
#11091=B_SPLINE_CURVE_WITH_KNOTS('',2,(#40457,#40458,#40459),
 .UNSPECIFIED.,.F.,.F.,(3,3),(0.,1.),.UNSPECIFIED.);
#11092=B_SPLINE_CURVE_WITH_KNOTS('',2,(#40461,#40462,#40463),
 .UNSPECIFIED.,.F.,.F.,(3,3),(0.,1.),.UNSPECIFIED.);
#11093=B_SPLINE_CURVE_WITH_KNOTS('',2,(#40465,#40466,#40467),
 .UNSPECIFIED.,.F.,.F.,(3,3),(0.,1.),.UNSPECIFIED.);
#11094=B_SPLINE_CURVE_WITH_KNOTS('',2,(#40469,#40470,#40471),
 .UNSPECIFIED.,.F.,.F.,(3,3),(0.,1.),.UNSPECIFIED.);
#11095=B_SPLINE_CURVE_WITH_KNOTS('',3,(#40481,#40482,#40483,#40484,#40485,
#40486,#40487,#40488,#40489,#40490),.UNSPECIFIED.,.F.,.F.,(4,2,2,2,4),(0.,
0.0565038365347674,0.113007673069535,0.169664342772315,0.226321012475095),
 .UNSPECIFIED.);
#11096=B_SPLINE_CURVE_WITH_KNOTS('',3,(#40501,#40502,#40503,#40504,#40505,
#40506,#40507,#40508,#40509,#40510),.UNSPECIFIED.,.F.,.F.,(4,2,2,2,4),(-0.226321012475095,
-0.169664342772315,-0.113007673069535,-0.0565038365347675,0.),
 .UNSPECIFIED.);
#11097=B_SPLINE_CURVE_WITH_KNOTS('',3,(#40520,#40521,#40522,#40523,#40524,
#40525,#40526,#40527,#40528,#40529),.UNSPECIFIED.,.F.,.F.,(4,2,2,2,4),(0.,
0.0565038365347674,0.113007673069535,0.169664342772315,0.226321012475095),
 .UNSPECIFIED.);
#11098=B_SPLINE_CURVE_WITH_KNOTS('',3,(#40540,#40541,#40542,#40543,#40544,
#40545,#40546,#40547,#40548,#40549,#40550,#40551,#40552,#40553),
 .UNSPECIFIED.,.F.,.F.,(4,2,2,2,2,2,4),(-0.577484191975641,-0.576699234562216,
-0.508563556454706,-0.443999452377128,-0.379354331952853,-0.330847656983477,
-0.288349617279839),.UNSPECIFIED.);
#11099=B_SPLINE_CURVE_WITH_KNOTS('',3,(#40556,#40557,#40558,#40559,#40560,
#40561,#40562,#40563,#40564,#40565,#40566,#40567,#40568,#40569),
 .UNSPECIFIED.,.F.,.F.,(4,2,2,2,2,2,4),(-0.288349617199946,-0.245851577508476,
-0.19734490255298,-0.132699782147205,-0.0681356780881004,0.,0.000784957413179436),
 .UNSPECIFIED.);
#11100=B_SPLINE_CURVE_WITH_KNOTS('',3,(#40574,#40575,#40576,#40577,#40578,
#40579,#40580,#40581,#40582,#40583),.UNSPECIFIED.,.F.,.F.,(4,2,2,2,4),(0.452090436017012,
0.508593613016053,0.565096790015094,0.621605199566296,0.678113609117498),
 .UNSPECIFIED.);
#11101=B_SPLINE_CURVE_WITH_KNOTS('',3,(#40589,#40590,#40591,#40592,#40593,
#40594,#40595,#40596,#40597,#40598),.UNSPECIFIED.,.F.,.F.,(4,2,2,2,4),(0.226067262916527,
0.282575672467729,0.339084082018931,0.395587259017972,0.452090436017013),
 .UNSPECIFIED.);
#11102=B_SPLINE_CURVE_WITH_KNOTS('',3,(#40620,#40621,#40622,#40623),
 .UNSPECIFIED.,.F.,.F.,(4,4),(2.49844264446827,2.64149356559396),
 .UNSPECIFIED.);
#11103=B_SPLINE_CURVE_WITH_KNOTS('',3,(#40624,#40625,#40626,#40627),
 .UNSPECIFIED.,.F.,.F.,(4,4),(2.49844264446365,2.64149356558944),
 .UNSPECIFIED.);
#11104=B_SPLINE_CURVE_WITH_KNOTS('',3,(#40628,#40629,#40630,#40631),
 .UNSPECIFIED.,.F.,.F.,(4,4),(2.49844264445768,2.64149356558346),
 .UNSPECIFIED.);
#11105=B_SPLINE_CURVE_WITH_KNOTS('',3,(#40632,#40633,#40634,#40635),
 .UNSPECIFIED.,.F.,.F.,(4,4),(2.49844264445882,2.64149356558449),
 .UNSPECIFIED.);
#11106=B_SPLINE_CURVE_WITH_KNOTS('',3,(#40636,#40637,#40638,#40639),
 .UNSPECIFIED.,.F.,.F.,(4,4),(2.49844264444559,2.64149356557132),
 .UNSPECIFIED.);
#11107=B_SPLINE_CURVE_WITH_KNOTS('',3,(#40645,#40646,#40647,#40648),
 .UNSPECIFIED.,.F.,.F.,(4,4),(2.49844264448387,2.64149356560953),
 .UNSPECIFIED.);
#11108=B_SPLINE_CURVE_WITH_KNOTS('',3,(#40649,#40650,#40651,#40652),
 .UNSPECIFIED.,.F.,.F.,(4,4),(2.49844264446318,2.64149356558896),
 .UNSPECIFIED.);
#11109=B_SPLINE_CURVE_WITH_KNOTS('',3,(#40653,#40654,#40655,#40656),
 .UNSPECIFIED.,.F.,.F.,(4,4),(2.49844264447263,2.6414935655984),
 .UNSPECIFIED.);
#11110=B_SPLINE_CURVE_WITH_KNOTS('',2,(#40779,#40780,#40781),
 .UNSPECIFIED.,.F.,.F.,(3,3),(0.,1.),.UNSPECIFIED.);
#11111=B_SPLINE_CURVE_WITH_KNOTS('',2,(#40791,#40792,#40793),
 .UNSPECIFIED.,.F.,.F.,(3,3),(0.,1.),.UNSPECIFIED.);
#11112=B_SPLINE_CURVE_WITH_KNOTS('',2,(#40802,#40803,#40804),
 .UNSPECIFIED.,.F.,.F.,(3,3),(0.,1.),.UNSPECIFIED.);
#11113=B_SPLINE_CURVE_WITH_KNOTS('',2,(#40813,#40814,#40815),
 .UNSPECIFIED.,.F.,.F.,(3,3),(0.,1.),.UNSPECIFIED.);
#11114=B_SPLINE_CURVE_WITH_KNOTS('',2,(#40824,#40825,#40826),
 .UNSPECIFIED.,.F.,.F.,(3,3),(0.,1.),.UNSPECIFIED.);
#11115=B_SPLINE_CURVE_WITH_KNOTS('',2,(#40835,#40836,#40837),
 .UNSPECIFIED.,.F.,.F.,(3,3),(0.,1.),.UNSPECIFIED.);
#11116=B_SPLINE_CURVE_WITH_KNOTS('',2,(#40846,#40847,#40848),
 .UNSPECIFIED.,.F.,.F.,(3,3),(0.,1.),.UNSPECIFIED.);
#11117=B_SPLINE_CURVE_WITH_KNOTS('',2,(#40857,#40858,#40859),
 .UNSPECIFIED.,.F.,.F.,(3,3),(0.,1.),.UNSPECIFIED.);
#11118=B_SPLINE_CURVE_WITH_KNOTS('',2,(#40868,#40869,#40870),
 .UNSPECIFIED.,.F.,.F.,(3,3),(0.,1.),.UNSPECIFIED.);
#11119=B_SPLINE_CURVE_WITH_KNOTS('',2,(#40879,#40880,#40881),
 .UNSPECIFIED.,.F.,.F.,(3,3),(0.,1.),.UNSPECIFIED.);
#11120=B_SPLINE_CURVE_WITH_KNOTS('',2,(#40894,#40895,#40896),
 .UNSPECIFIED.,.F.,.F.,(3,3),(0.,1.),.UNSPECIFIED.);
#11121=B_SPLINE_CURVE_WITH_KNOTS('',2,(#40907,#40908,#40909),
 .UNSPECIFIED.,.F.,.F.,(3,3),(0.,1.),.UNSPECIFIED.);
#11122=B_SPLINE_CURVE_WITH_KNOTS('',2,(#40919,#40920,#40921),
 .UNSPECIFIED.,.F.,.F.,(3,3),(0.,1.),.UNSPECIFIED.);
#11123=B_SPLINE_CURVE_WITH_KNOTS('',2,(#40930,#40931,#40932),
 .UNSPECIFIED.,.F.,.F.,(3,3),(0.,1.),.UNSPECIFIED.);
#11124=B_SPLINE_CURVE_WITH_KNOTS('',2,(#40941,#40942,#40943),
 .UNSPECIFIED.,.F.,.F.,(3,3),(0.,1.),.UNSPECIFIED.);
#11125=B_SPLINE_CURVE_WITH_KNOTS('',2,(#40952,#40953,#40954),
 .UNSPECIFIED.,.F.,.F.,(3,3),(0.,1.),.UNSPECIFIED.);
#11126=B_SPLINE_CURVE_WITH_KNOTS('',2,(#40963,#40964,#40965),
 .UNSPECIFIED.,.F.,.F.,(3,3),(0.,1.),.UNSPECIFIED.);
#11127=B_SPLINE_CURVE_WITH_KNOTS('',2,(#40974,#40975,#40976),
 .UNSPECIFIED.,.F.,.F.,(3,3),(0.,1.),.UNSPECIFIED.);
#11128=B_SPLINE_CURVE_WITH_KNOTS('',2,(#40985,#40986,#40987),
 .UNSPECIFIED.,.F.,.F.,(3,3),(0.,1.),.UNSPECIFIED.);
#11129=B_SPLINE_CURVE_WITH_KNOTS('',2,(#40996,#40997,#40998),
 .UNSPECIFIED.,.F.,.F.,(3,3),(0.,1.),.UNSPECIFIED.);
#11130=B_SPLINE_CURVE_WITH_KNOTS('',2,(#41007,#41008,#41009),
 .UNSPECIFIED.,.F.,.F.,(3,3),(0.,1.),.UNSPECIFIED.);
#11131=B_SPLINE_CURVE_WITH_KNOTS('',2,(#41018,#41019,#41020),
 .UNSPECIFIED.,.F.,.F.,(3,3),(0.,1.),.UNSPECIFIED.);
#11132=B_SPLINE_CURVE_WITH_KNOTS('',2,(#41029,#41030,#41031),
 .UNSPECIFIED.,.F.,.F.,(3,3),(0.,1.),.UNSPECIFIED.);
#11133=B_SPLINE_CURVE_WITH_KNOTS('',2,(#41040,#41041,#41042),
 .UNSPECIFIED.,.F.,.F.,(3,3),(0.,1.),.UNSPECIFIED.);
#11134=B_SPLINE_CURVE_WITH_KNOTS('',2,(#41055,#41056,#41057),
 .UNSPECIFIED.,.F.,.F.,(3,3),(0.,1.),.UNSPECIFIED.);
#11135=B_SPLINE_CURVE_WITH_KNOTS('',2,(#41066,#41067,#41068),
 .UNSPECIFIED.,.F.,.F.,(3,3),(0.,1.),.UNSPECIFIED.);
#11136=B_SPLINE_CURVE_WITH_KNOTS('',2,(#41077,#41078,#41079),
 .UNSPECIFIED.,.F.,.F.,(3,3),(0.,1.),.UNSPECIFIED.);
#11137=B_SPLINE_CURVE_WITH_KNOTS('',2,(#41088,#41089,#41090),
 .UNSPECIFIED.,.F.,.F.,(3,3),(0.,1.),.UNSPECIFIED.);
#11138=B_SPLINE_CURVE_WITH_KNOTS('',2,(#41099,#41100,#41101),
 .UNSPECIFIED.,.F.,.F.,(3,3),(0.,1.),.UNSPECIFIED.);
#11139=B_SPLINE_CURVE_WITH_KNOTS('',2,(#41110,#41111,#41112),
 .UNSPECIFIED.,.F.,.F.,(3,3),(0.,1.),.UNSPECIFIED.);
#11140=B_SPLINE_CURVE_WITH_KNOTS('',2,(#41121,#41122,#41123),
 .UNSPECIFIED.,.F.,.F.,(3,3),(0.,1.),.UNSPECIFIED.);
#11141=B_SPLINE_CURVE_WITH_KNOTS('',2,(#41132,#41133,#41134),
 .UNSPECIFIED.,.F.,.F.,(3,3),(0.,1.),.UNSPECIFIED.);
#11142=B_SPLINE_CURVE_WITH_KNOTS('',2,(#41143,#41144,#41145),
 .UNSPECIFIED.,.F.,.F.,(3,3),(0.,1.),.UNSPECIFIED.);
#11143=B_SPLINE_CURVE_WITH_KNOTS('',2,(#41154,#41155,#41156),
 .UNSPECIFIED.,.F.,.F.,(3,3),(0.,1.),.UNSPECIFIED.);
#11144=B_SPLINE_CURVE_WITH_KNOTS('',2,(#41165,#41166,#41167),
 .UNSPECIFIED.,.F.,.F.,(3,3),(0.,1.),.UNSPECIFIED.);
#11145=B_SPLINE_CURVE_WITH_KNOTS('',2,(#41176,#41177,#41178),
 .UNSPECIFIED.,.F.,.F.,(3,3),(0.,1.),.UNSPECIFIED.);
#11146=B_SPLINE_CURVE_WITH_KNOTS('',2,(#41187,#41188,#41189),
 .UNSPECIFIED.,.F.,.F.,(3,3),(0.,1.),.UNSPECIFIED.);
#11147=B_SPLINE_CURVE_WITH_KNOTS('',2,(#41198,#41199,#41200),
 .UNSPECIFIED.,.F.,.F.,(3,3),(0.,1.),.UNSPECIFIED.);
#11148=B_SPLINE_CURVE_WITH_KNOTS('',2,(#41209,#41210,#41211),
 .UNSPECIFIED.,.F.,.F.,(3,3),(0.,1.),.UNSPECIFIED.);
#11149=B_SPLINE_CURVE_WITH_KNOTS('',2,(#41220,#41221,#41222),
 .UNSPECIFIED.,.F.,.F.,(3,3),(0.,1.),.UNSPECIFIED.);
#11150=B_SPLINE_CURVE_WITH_KNOTS('',2,(#41231,#41232,#41233),
 .UNSPECIFIED.,.F.,.F.,(3,3),(0.,1.),.UNSPECIFIED.);
#11151=B_SPLINE_CURVE_WITH_KNOTS('',2,(#41242,#41243,#41244),
 .UNSPECIFIED.,.F.,.F.,(3,3),(0.,1.),.UNSPECIFIED.);
#11152=B_SPLINE_CURVE_WITH_KNOTS('',2,(#41257,#41258,#41259),
 .UNSPECIFIED.,.F.,.F.,(3,3),(0.,1.),.UNSPECIFIED.);
#11153=B_SPLINE_CURVE_WITH_KNOTS('',2,(#41266,#41267,#41268),
 .UNSPECIFIED.,.F.,.F.,(3,3),(0.,1.),.UNSPECIFIED.);
#11154=B_SPLINE_CURVE_WITH_KNOTS('',2,(#41284,#41285,#41286),
 .UNSPECIFIED.,.F.,.F.,(3,3),(0.,1.),.UNSPECIFIED.);
#11155=B_SPLINE_CURVE_WITH_KNOTS('',2,(#41295,#41296,#41297),
 .UNSPECIFIED.,.F.,.F.,(3,3),(0.,1.),.UNSPECIFIED.);
#11156=B_SPLINE_CURVE_WITH_KNOTS('',2,(#41306,#41307,#41308),
 .UNSPECIFIED.,.F.,.F.,(3,3),(0.,1.),.UNSPECIFIED.);
#11157=B_SPLINE_CURVE_WITH_KNOTS('',2,(#41317,#41318,#41319),
 .UNSPECIFIED.,.F.,.F.,(3,3),(0.,1.),.UNSPECIFIED.);
#11158=B_SPLINE_CURVE_WITH_KNOTS('',2,(#41334,#41335,#41336),
 .UNSPECIFIED.,.F.,.F.,(3,3),(0.,1.),.UNSPECIFIED.);
#11159=B_SPLINE_CURVE_WITH_KNOTS('',2,(#41345,#41346,#41347),
 .UNSPECIFIED.,.F.,.F.,(3,3),(0.,1.),.UNSPECIFIED.);
#11160=B_SPLINE_CURVE_WITH_KNOTS('',2,(#41356,#41357,#41358),
 .UNSPECIFIED.,.F.,.F.,(3,3),(0.,1.),.UNSPECIFIED.);
#11161=B_SPLINE_CURVE_WITH_KNOTS('',2,(#41367,#41368,#41369),
 .UNSPECIFIED.,.F.,.F.,(3,3),(0.,1.),.UNSPECIFIED.);
#11162=B_SPLINE_CURVE_WITH_KNOTS('',2,(#41378,#41379,#41380),
 .UNSPECIFIED.,.F.,.F.,(3,3),(0.,1.),.UNSPECIFIED.);
#11163=B_SPLINE_CURVE_WITH_KNOTS('',2,(#41389,#41390,#41391),
 .UNSPECIFIED.,.F.,.F.,(3,3),(0.,1.),.UNSPECIFIED.);
#11164=B_SPLINE_CURVE_WITH_KNOTS('',2,(#41400,#41401,#41402),
 .UNSPECIFIED.,.F.,.F.,(3,3),(0.,1.),.UNSPECIFIED.);
#11165=B_SPLINE_CURVE_WITH_KNOTS('',2,(#41434,#41435,#41436),
 .UNSPECIFIED.,.F.,.F.,(3,3),(0.,1.),.UNSPECIFIED.);
#11166=B_SPLINE_CURVE_WITH_KNOTS('',2,(#41445,#41446,#41447),
 .UNSPECIFIED.,.F.,.F.,(3,3),(0.,1.),.UNSPECIFIED.);
#11167=B_SPLINE_CURVE_WITH_KNOTS('',3,(#41609,#41610,#41611,#41612),
 .UNSPECIFIED.,.F.,.F.,(4,4),(2.9602728791883,3.32291242799128),
 .UNSPECIFIED.);
#11168=B_SPLINE_CURVE_WITH_KNOTS('',3,(#41614,#41615,#41616,#41617),
 .UNSPECIFIED.,.F.,.F.,(4,4),(-3.32291242799128,-3.14159265358979),
 .UNSPECIFIED.);
#11169=B_SPLINE_CURVE_WITH_KNOTS('',3,(#41618,#41619,#41620,#41621),
 .UNSPECIFIED.,.F.,.F.,(4,4),(-3.14159265358979,-2.9602728791883),
 .UNSPECIFIED.);
#11170=B_SPLINE_CURVE_WITH_KNOTS('',3,(#41687,#41688,#41689,#41690),
 .UNSPECIFIED.,.F.,.F.,(4,4),(-0.181319774401493,0.181319774401488),
 .UNSPECIFIED.);
#11171=B_SPLINE_CURVE_WITH_KNOTS('',3,(#41691,#41692,#41693,#41694),
 .UNSPECIFIED.,.F.,.F.,(4,4),(-0.181319774401488,0.181319774401493),
 .UNSPECIFIED.);
#11172=B_SPLINE_CURVE_WITH_KNOTS('',3,(#41699,#41700,#41701,#41702),
 .UNSPECIFIED.,.F.,.F.,(4,4),(6.10186553277809,6.46450508158109),
 .UNSPECIFIED.);
#11173=B_SPLINE_CURVE_WITH_KNOTS('',3,(#41729,#41730,#41731,#41732),
 .UNSPECIFIED.,.F.,.F.,(4,4),(2.9602728791883,3.32291242799128),
 .UNSPECIFIED.);
#11174=B_SPLINE_CURVE_WITH_KNOTS('',3,(#41734,#41735,#41736,#41737),
 .UNSPECIFIED.,.F.,.F.,(4,4),(-3.32291242799128,-3.14159265358979),
 .UNSPECIFIED.);
#11175=B_SPLINE_CURVE_WITH_KNOTS('',3,(#41738,#41739,#41740,#41741),
 .UNSPECIFIED.,.F.,.F.,(4,4),(-3.14159265358979,-2.9602728791883),
 .UNSPECIFIED.);
#11176=B_SPLINE_CURVE_WITH_KNOTS('',3,(#41770,#41771,#41772,#41773),
 .UNSPECIFIED.,.F.,.F.,(4,4),(-6.46450508158109,-6.10186553277809),
 .UNSPECIFIED.);
#11177=B_SPLINE_CURVE_WITH_KNOTS('',3,(#41793,#41794,#41795,#41796),
 .UNSPECIFIED.,.F.,.F.,(4,4),(0.413605043247719,0.437854341815321),
 .UNSPECIFIED.);
#11178=B_SPLINE_CURVE_WITH_KNOTS('',3,(#41800,#41801,#41802,#41803),
 .UNSPECIFIED.,.F.,.F.,(4,4),(1.36755809423905,1.39180739280665),
 .UNSPECIFIED.);
#11179=B_SPLINE_CURVE_WITH_KNOTS('',3,(#41966,#41967,#41968,#41969,#41970,
#41971,#41972,#41973,#41974,#41975,#41976,#41977,#41978,#41979,#41980,#41981,
#41982,#41983),.UNSPECIFIED.,.F.,.F.,(4,2,2,2,2,2,2,2,4),(2.77896888287132,
2.78150698603454,2.79283731888666,2.85278626064221,2.96447510619432,3.07616395174642,
3.29954164285062,3.83796248419292,4.32657905104996),.UNSPECIFIED.);
#11180=B_SPLINE_CURVE_WITH_KNOTS('',3,(#41988,#41989,#41990,#41991,#41992,
#41993,#41994,#41995,#41996,#41997),.UNSPECIFIED.,.F.,.F.,(4,2,2,2,4),(0.700334773405899,
0.978276696075167,1.30411559546238,1.6299544948496,1.90789641751887),
 .UNSPECIFIED.);
#11181=B_SPLINE_CURVE_WITH_KNOTS('',3,(#42000,#42001,#42002,#42003,#42004,
#42005,#42006,#42007,#42008,#42009),.UNSPECIFIED.,.F.,.F.,(4,2,2,2,4),(0.7003347734059,
0.978276696075167,1.30411559546238,1.6299544948496,1.90789641751887),
 .UNSPECIFIED.);
#11182=B_SPLINE_CURVE_WITH_KNOTS('',3,(#42021,#42022,#42023,#42024,#42025,
#42026,#42027,#42028,#42029,#42030),.UNSPECIFIED.,.F.,.F.,(4,2,2,2,4),(0.700334773405899,
0.978276696075167,1.30411559546238,1.6299544948496,1.90789641751887),
 .UNSPECIFIED.);
#11183=B_SPLINE_CURVE_WITH_KNOTS('',3,(#42042,#42043,#42044,#42045,#42046,
#42047,#42048,#42049,#42050,#42051),.UNSPECIFIED.,.F.,.F.,(4,2,2,2,4),(0.7003347734059,
0.978276696075167,1.30411559546238,1.6299544948496,1.90789641751886),
 .UNSPECIFIED.);
#11184=B_SPLINE_CURVE_WITH_KNOTS('',3,(#42057,#42058,#42059,#42060,#42061,
#42062,#42063,#42064,#42065,#42066,#42067,#42068,#42069,#42070,#42071,#42072,
#42073,#42074),.UNSPECIFIED.,.F.,.F.,(4,2,2,2,2,2,2,2,4),(1.12664595716984,
1.61526252402689,2.15368336536918,2.37706105647338,2.48874990202548,2.60043874757758,
2.66038768933314,2.67171802218525,2.67425612534847),.UNSPECIFIED.);
#11185=B_SPLINE_CURVE_WITH_KNOTS('',3,(#42078,#42079,#42080,#42081),
 .UNSPECIFIED.,.F.,.F.,(4,4),(1.36755809423905,1.39180739280665),
 .UNSPECIFIED.);
#11186=B_SPLINE_CURVE_WITH_KNOTS('',3,(#42084,#42085,#42086,#42087),
 .UNSPECIFIED.,.F.,.F.,(4,4),(0.413605043247719,0.437854341815321),
 .UNSPECIFIED.);
#11187=B_SPLINE_CURVE_WITH_KNOTS('',3,(#42092,#42093,#42094,#42095),
 .UNSPECIFIED.,.F.,.F.,(4,4),(1.36755809423905,1.39180739280665),
 .UNSPECIFIED.);
#11188=B_SPLINE_CURVE_WITH_KNOTS('',3,(#42098,#42099,#42100,#42101),
 .UNSPECIFIED.,.F.,.F.,(4,4),(0.41360504324772,0.437854341815321),
 .UNSPECIFIED.);
#11189=B_SPLINE_CURVE_WITH_KNOTS('',3,(#44987,#44988,#44989,#44990,#44991,
#44992,#44993,#44994,#44995,#44996),.UNSPECIFIED.,.F.,.F.,(4,2,2,2,4),(0.,
0.0949942193143224,0.189988438628645,0.284969155661888,0.379949872695131),
 .UNSPECIFIED.);
#11190=B_SPLINE_CURVE_WITH_KNOTS('',3,(#44998,#44999,#45000,#45001,#45002,
#45003,#45004,#45005,#45006,#45007),.UNSPECIFIED.,.F.,.F.,(4,2,2,2,4),(1.13984961808539,
1.23483033511864,1.32981105215188,1.4248052714662,1.51979949078052),
 .UNSPECIFIED.);
#11191=B_SPLINE_CURVE_WITH_KNOTS('',3,(#45011,#45012,#45013,#45014,#45015,
#45016,#45017,#45018,#45019,#45020),.UNSPECIFIED.,.F.,.F.,(4,2,2,2,4),(0.,
0.0949942193143224,0.189988438628645,0.284969155661888,0.379949872695131),
 .UNSPECIFIED.);
#11192=B_SPLINE_CURVE_WITH_KNOTS('',3,(#45021,#45022,#45023,#45024,#45025,
#45026,#45027,#45028,#45029,#45030,#45031,#45032,#45033,#45034,#45035,#45036,
#45037,#45038,#45039,#45040,#45041,#45042,#45043,#45044,#45045,#45046),
 .UNSPECIFIED.,.F.,.F.,(4,2,2,2,2,2,2,2,2,2,2,2,4),(0.379949872695131,0.474930589728375,
0.569911306761618,0.66490552607594,0.759899745390262,0.854893964704585,
0.949888184018907,1.04486890105215,1.13984961808539,1.23483033511864,1.32981105215188,
1.4248052714662,1.51979949078053),.UNSPECIFIED.);
#11193=B_SPLINE_CURVE_WITH_KNOTS('',3,(#45047,#45048,#45049,#45050,#45051,
#45052,#45053,#45054,#45055,#45056,#45057,#45058,#45059,#45060,#45061,#45062,
#45063,#45064),.UNSPECIFIED.,.F.,.F.,(4,2,2,2,2,2,2,2,4),(0.379949872695131,
0.474930589728374,0.569911306761618,0.66490552607594,0.759899745390262,
0.854893964704585,0.949888184018907,1.04486890105215,1.13984961808539),
 .UNSPECIFIED.);
#11194=B_SPLINE_CURVE_WITH_KNOTS('',3,(#45288,#45289,#45290,#45291),
 .UNSPECIFIED.,.F.,.F.,(4,4),(0.,0.0373327877210394),.UNSPECIFIED.);
#11195=B_SPLINE_CURVE_WITH_KNOTS('',3,(#45296,#45297,#45298,#45299),
 .UNSPECIFIED.,.F.,.F.,(4,4),(0.,0.0373327877209389),.UNSPECIFIED.);
#11196=B_SPLINE_CURVE_WITH_KNOTS('',3,(#45317,#45318,#45319,#45320),
 .UNSPECIFIED.,.F.,.F.,(4,4),(0.,0.0373327852068557),.UNSPECIFIED.);
#11197=B_SPLINE_CURVE_WITH_KNOTS('',3,(#45329,#45330,#45331,#45332),
 .UNSPECIFIED.,.F.,.F.,(4,4),(0.,0.0373327877209165),.UNSPECIFIED.);
#11198=B_SPLINE_CURVE_WITH_KNOTS('',3,(#45439,#45440,#45441,#45442,#45443,
#45444),.UNSPECIFIED.,.F.,.F.,(4,1,1,4),(0.217693875784178,0.975255008179982,
1.48029576311052,1.98533651804105),.UNSPECIFIED.);
#11199=B_SPLINE_CURVE_WITH_KNOTS('',3,(#45446,#45447,#45448,#45449,#45450,
#45451),.UNSPECIFIED.,.F.,.F.,(4,1,1,4),(0.217693875784177,0.975255008179981,
1.48029576311052,1.98533651804105),.UNSPECIFIED.);
#11200=B_SPLINE_CURVE_WITH_KNOTS('',3,(#45453,#45454,#45455,#45456,#45457,
#45458),.UNSPECIFIED.,.F.,.F.,(4,1,1,4),(0.217693875784176,0.975255008179981,
1.48029576311052,1.98533651804105),.UNSPECIFIED.);
#11201=B_SPLINE_CURVE_WITH_KNOTS('',3,(#45460,#45461,#45462,#45463,#45464,
#45465),.UNSPECIFIED.,.F.,.F.,(4,1,1,4),(0.217693875784176,0.975255008179981,
1.48029576311052,1.98533651804105),.UNSPECIFIED.);
#11202=B_SPLINE_CURVE_WITH_KNOTS('',3,(#45467,#45468,#45469,#45470,#45471),
 .UNSPECIFIED.,.F.,.F.,(4,1,4),(1.10151519691261,1.48029576311052,1.98533651804105),
 .UNSPECIFIED.);
#11203=B_SPLINE_CURVE_WITH_KNOTS('',3,(#45474,#45475,#45476,#45477,#45478),
 .UNSPECIFIED.,.F.,.F.,(4,1,4),(0.217693875784177,0.975255008179981,1.10151519691261),
 .UNSPECIFIED.);
#11204=B_SPLINE_CURVE_WITH_KNOTS('',3,(#45479,#45480,#45481,#45482,#45483,
#45484),.UNSPECIFIED.,.F.,.F.,(4,1,1,4),(0.217693875784177,0.975255008179981,
1.48029576311052,1.98533651804105),.UNSPECIFIED.);
#11205=B_SPLINE_CURVE_WITH_KNOTS('',3,(#45490,#45491,#45492,#45493,#45494,
#45495),.UNSPECIFIED.,.F.,.F.,(4,2,4),(-0.0848441742917886,-0.0424181029814519,
0.),.UNSPECIFIED.);
#11206=B_SPLINE_CURVE_WITH_KNOTS('',3,(#45496,#45497,#45498,#45499,#45500,
#45501),.UNSPECIFIED.,.F.,.F.,(4,2,4),(-0.0848441721845653,-0.0424257383943444,
0.),.UNSPECIFIED.);
#11207=B_SPLINE_CURVE_WITH_KNOTS('',3,(#45504,#45505,#45506,#45507,#45508,
#45509),.UNSPECIFIED.,.F.,.F.,(4,2,4),(-0.0848441742849619,-0.0424181029793345,
0.),.UNSPECIFIED.);
#11208=B_SPLINE_CURVE_WITH_KNOTS('',3,(#45511,#45512,#45513,#45514,#45515,
#45516),.UNSPECIFIED.,.F.,.F.,(4,2,4),(-0.0848441721710981,-0.04242573838781,
0.),.UNSPECIFIED.);
#11209=B_SPLINE_CURVE_WITH_KNOTS('',3,(#45522,#45523,#45524,#45525,#45526,
#45527),.UNSPECIFIED.,.F.,.F.,(4,2,4),(-0.08484417429082,-0.0424181029808318,
0.),.UNSPECIFIED.);
#11210=B_SPLINE_CURVE_WITH_KNOTS('',3,(#45528,#45529,#45530,#45531,#45532,
#45533),.UNSPECIFIED.,.F.,.F.,(4,2,4),(-0.0848441721741252,-0.0424257383913701,
0.),.UNSPECIFIED.);
#11211=B_SPLINE_CURVE_WITH_KNOTS('',3,(#45536,#45537,#45538,#45539,#45540,
#45541),.UNSPECIFIED.,.F.,.F.,(4,2,4),(-0.0848441742890261,-0.0424181029805331,
0.),.UNSPECIFIED.);
#11212=B_SPLINE_CURVE_WITH_KNOTS('',3,(#45543,#45544,#45545,#45546,#45547,
#45548),.UNSPECIFIED.,.F.,.F.,(4,2,4),(-0.0848441721767493,-0.0424257383933299,
0.),.UNSPECIFIED.);
#11213=B_SPLINE_CURVE_WITH_KNOTS('',3,(#45554,#45555,#45556,#45557,#45558,
#45559),.UNSPECIFIED.,.F.,.F.,(4,2,4),(-0.0848441742833862,-0.0424181029791782,
0.),.UNSPECIFIED.);
#11214=B_SPLINE_CURVE_WITH_KNOTS('',3,(#45560,#45561,#45562,#45563,#45564,
#45565),.UNSPECIFIED.,.F.,.F.,(4,2,4),(-0.0848441721772216,-0.0424257383936094,
0.),.UNSPECIFIED.);
#11215=B_SPLINE_CURVE_WITH_KNOTS('',3,(#45568,#45569,#45570,#45571,#45572,
#45573),.UNSPECIFIED.,.F.,.F.,(4,2,4),(-0.0848441742900362,-0.0424181029807091,
0.),.UNSPECIFIED.);
#11216=B_SPLINE_CURVE_WITH_KNOTS('',3,(#45575,#45576,#45577,#45578,#45579,
#45580),.UNSPECIFIED.,.F.,.F.,(4,2,4),(-0.0848441721839697,-0.0424257383950013,
0.),.UNSPECIFIED.);
#11217=B_SPLINE_CURVE_WITH_KNOTS('',3,(#45606,#45607,#45608,#45609,#45610,
#45611),.UNSPECIFIED.,.F.,.F.,(4,1,1,4),(-1.98100236513816,-1.48029576311052,
-0.975255008179982,-0.222028028687133),.UNSPECIFIED.);
#11218=B_SPLINE_CURVE_WITH_KNOTS('',3,(#45642,#45643,#45644,#45645,#45646,
#45647),.UNSPECIFIED.,.F.,.F.,(4,1,1,4),(-1.98100236513816,-1.48029576311052,
-0.975255008179981,-0.222028028687133),.UNSPECIFIED.);
#11219=B_SPLINE_CURVE_WITH_KNOTS('',3,(#45672,#45673,#45674,#45675,#45676,
#45677),.UNSPECIFIED.,.F.,.F.,(4,1,1,4),(-1.98100236513816,-1.48029576311052,
-0.975255008179981,-0.222028028687133),.UNSPECIFIED.);
#11220=B_SPLINE_CURVE_WITH_KNOTS('',3,(#45714,#45715,#45716,#45717,#45718,
#45719),.UNSPECIFIED.,.F.,.F.,(4,1,1,4),(-1.98100236513816,-1.48029576311052,
-0.975255008179981,-0.222028028687132),.UNSPECIFIED.);
#11221=B_SPLINE_CURVE_WITH_KNOTS('',3,(#45744,#45745,#45746,#45747,#45748,
#45749),.UNSPECIFIED.,.F.,.F.,(4,1,1,4),(-1.98100236513816,-1.48029576311052,
-0.975255008179981,-0.222028028687132),.UNSPECIFIED.);
#11222=B_SPLINE_CURVE_WITH_KNOTS('',3,(#45786,#45787,#45788,#45789,#45790,
#45791),.UNSPECIFIED.,.F.,.F.,(4,1,1,4),(-1.98100236513816,-1.48029576311052,
-0.975255008179981,-0.222028028687132),.UNSPECIFIED.);
#11223=B_SPLINE_CURVE_WITH_KNOTS('',3,(#46321,#46322,#46323,#46324,#46325,
#46326,#46327,#46328,#46329,#46330,#46331,#46332,#46333,#46334,#46335,#46336,
#46337,#46338,#46339,#46340,#46341,#46342,#46343,#46344,#46345,#46346,#46347,
#46348,#46349,#46350),.UNSPECIFIED.,.T.,.F.,(4,1,1,1,2,2,1,2,1,1,1,1,1,
1,1,1,1,2,1,2,2,4),(-3.59083978231636,-3.44656525188405,-3.39847374173995,
-3.30229072145174,-3.20610770116353,-3.07786267055688,-3.01374015525356,
-2.94961763995024,-2.72519034172216,-2.61297669260812,-2.5568698680511,
-2.52881645577259,-2.50076304349408,-2.38854939438004,-2.33244256982302,
-2.276335745266,-2.16412209615196,-2.05190844703792,-1.92366341643128,-1.79541838582463,
-1.66717486055154,-1.53893133527844),.UNSPECIFIED.);
#11224=B_SPLINE_CURVE_WITH_KNOTS('',3,(#46647,#46648,#46649,#46650,#46651,
#46652,#46653,#46654,#46655,#46656,#46657,#46658,#46659,#46660,#46661,#46662,
#46663,#46664,#46665,#46666,#46667,#46668,#46669,#46670,#46671,#46672,#46673,
#46674,#46675,#46676),.UNSPECIFIED.,.T.,.F.,(4,2,2,1,2,1,1,1,1,1,1,1,1,
1,2,1,2,2,1,1,1,4),(1.53893133527844,1.66717486055154,1.79541838582463,
1.92366341643128,2.05190844703792,2.16412209615196,2.276335745266,2.33244256982302,
2.38854939438004,2.50076304349408,2.52881645577259,2.5568698680511,2.61297669260812,
2.72519034172216,2.94961763995024,3.01374015525356,3.07786267055688,3.20610770116353,
3.30229072145174,3.39847374173995,3.44656525188405,3.59083978231636),
 .UNSPECIFIED.);
#11225=B_SPLINE_CURVE_WITH_KNOTS('',3,(#46706,#46707,#46708,#46709,#46710,
#46711,#46712,#46713,#46714,#46715),.UNSPECIFIED.,.F.,.F.,(4,3,3,4),(-4.0932327200247,
-3.99841245657804,-2.99880934243353,-2.06652207565086),.UNSPECIFIED.);
#11226=B_SPLINE_CURVE_WITH_KNOTS('',3,(#46718,#46719,#46720,#46721,#46722,
#46723,#46724,#46725,#46726,#46727),.UNSPECIFIED.,.F.,.F.,(4,3,3,4),(0.,
0.499801557072245,0.999603114144509,1.11488200921585),.UNSPECIFIED.);
#11227=B_SPLINE_CURVE_WITH_KNOTS('',3,(#46732,#46733,#46734,#46735,#46736,
#46737,#46738,#46739,#46740,#46741,#46742,#46743,#46744,#46745,#46746,#46747,
#46748,#46749,#46750,#46751,#46752,#46753),.UNSPECIFIED.,.F.,.F.,(4,3,3,
3,3,3,3,4),(-10.3764180272043,-9.99603114144511,-8.9964280273006,-7.99682491315609,
-6.99722179901157,-5.99761868486707,-4.99801557072256,-4.0932327200247),
 .UNSPECIFIED.);
#11228=B_SPLINE_CURVE_WITH_KNOTS('',3,(#46754,#46755,#46756,#46757,#46758,
#46759,#46760,#46761,#46762,#46763,#46764,#46765,#46766,#46767,#46768,#46769,
#46770,#46771,#46772,#46773,#46774,#46775),.UNSPECIFIED.,.F.,.F.,(4,3,3,
3,3,3,3,4),(1.11488200921585,1.99920622828902,2.99880934243353,3.99841245657804,
4.99801557072255,5.99761868486706,6.99722179901157,7.39806731639545),
 .UNSPECIFIED.);
#11229=B_SPLINE_CURVE_WITH_KNOTS('',3,(#46780,#46781,#46782,#46783,#46784,
#46785,#46786,#46787,#46788,#46789,#46790,#46791,#46792,#46793,#46794,#46795,
#46796,#46797,#46798,#46799,#46800,#46801),.UNSPECIFIED.,.F.,.F.,(4,3,3,
3,3,3,3,4),(-16.6596033343839,-15.9936498263122,-14.9940467121677,-13.9944435980232,
-12.9948404838786,-11.9952373697341,-10.9956342555896,-10.3764180272043),
 .UNSPECIFIED.);
#11230=B_SPLINE_CURVE_WITH_KNOTS('',3,(#46802,#46803,#46804,#46805,#46806,
#46807,#46808,#46809,#46810,#46811,#46812,#46813,#46814,#46815,#46816,#46817,
#46818,#46819,#46820,#46821,#46822,#46823),.UNSPECIFIED.,.F.,.F.,(4,3,3,
3,3,3,3,4),(7.39806731639545,7.99682491315608,8.9964280273006,9.99603114144511,
10.9956342555896,11.9952373697341,12.9948404838786,13.681252623575),
 .UNSPECIFIED.);
#11231=B_SPLINE_CURVE_WITH_KNOTS('',3,(#46828,#46829,#46830,#46831,#46832,
#46833,#46834,#46835,#46836,#46837,#46838,#46839,#46840,#46841,#46842,#46843,
#46844,#46845,#46846,#46847,#46848,#46849),.UNSPECIFIED.,.F.,.F.,(4,3,3,
3,3,3,3,4),(-22.9427886415635,-21.9912685111792,-20.9916653970347,-19.9920622828902,
-18.9924591687457,-17.9928560546012,-16.9932529404567,-16.6596033343839),
 .UNSPECIFIED.);
#11232=B_SPLINE_CURVE_WITH_KNOTS('',3,(#46850,#46851,#46852,#46853,#46854,
#46855,#46856,#46857,#46858,#46859,#46860,#46861,#46862,#46863,#46864,#46865,
#46866,#46867,#46868,#46869,#46870,#46871),.UNSPECIFIED.,.F.,.F.,(4,3,3,
3,3,3,3,4),(13.681252623575,13.9944435980232,14.9940467121677,15.9936498263122,
16.9932529404567,17.9928560546012,18.9924591687457,19.9644379307546),
 .UNSPECIFIED.);
#11233=B_SPLINE_CURVE_WITH_KNOTS('',3,(#46876,#46877,#46878,#46879,#46880,
#46881,#46882,#46883,#46884,#46885,#46886,#46887,#46888,#46889,#46890,#46891,
#46892,#46893,#46894,#46895,#46896,#46897,#46898,#46899,#46900),
 .UNSPECIFIED.,.F.,.F.,(4,3,3,3,3,3,3,3,4),(-29.225973948743,-28.9884903101908,
-27.9888871960463,-26.9892840819018,-25.9896809677573,-24.9900778536128,
-23.9904747394683,-22.9908716253238,-22.9427886415635),.UNSPECIFIED.);
#11234=B_SPLINE_CURVE_WITH_KNOTS('',3,(#46901,#46902,#46903,#46904,#46905,
#46906,#46907,#46908,#46909,#46910,#46911,#46912,#46913,#46914,#46915,#46916,
#46917,#46918,#46919,#46920,#46921,#46922,#46923,#46924,#46925),
 .UNSPECIFIED.,.F.,.F.,(4,3,3,3,3,3,3,3,4),(19.9644379307546,19.9920622828902,
20.9916653970347,21.9912685111792,22.9908716253238,23.9904747394683,24.9900778536128,
25.9896809677573,26.2476232379342),.UNSPECIFIED.);
#11235=B_SPLINE_CURVE_WITH_KNOTS('',3,(#46930,#46931,#46932,#46933,#46934,
#46935,#46936,#46937,#46938,#46939,#46940,#46941,#46942,#46943,#46944,#46945,
#46946,#46947,#46948,#46949,#46950,#46951),.UNSPECIFIED.,.F.,.F.,(4,3,3,
3,3,3,3,4),(-35.5091592559226,-34.9861089950579,-33.9865058809134,-32.9869027667689,
-31.9872996526244,-30.9876965384798,-29.9880934243353,-29.225973948743),
 .UNSPECIFIED.);
#11236=B_SPLINE_CURVE_WITH_KNOTS('',3,(#46952,#46953,#46954,#46955,#46956,
#46957,#46958,#46959,#46960,#46961,#46962,#46963,#46964,#46965,#46966,#46967,
#46968,#46969,#46970,#46971,#46972,#46973),.UNSPECIFIED.,.F.,.F.,(4,3,3,
3,3,3,3,4),(26.2476232379342,26.9892840819018,27.9888871960463,28.9884903101908,
29.9880934243353,30.9876965384798,31.9872996526244,32.5308085451138),
 .UNSPECIFIED.);
#11237=B_SPLINE_CURVE_WITH_KNOTS('',3,(#46978,#46979,#46980,#46981,#46982,
#46983,#46984,#46985,#46986,#46987,#46988,#46989,#46990,#46991,#46992,#46993,
#46994,#46995,#46996,#46997,#46998,#46999),.UNSPECIFIED.,.F.,.F.,(4,3,3,
3,3,3,3,4),(-41.7923445631022,-40.9837276799249,-39.9841245657804,-38.9845214516359,
-37.9849183374914,-36.9853152233469,-35.9857121092024,-35.5091592559226),
 .UNSPECIFIED.);
#11238=B_SPLINE_CURVE_WITH_KNOTS('',3,(#47000,#47001,#47002,#47003,#47004,
#47005,#47006,#47007,#47008,#47009,#47010,#47011,#47012,#47013,#47014,#47015,
#47016,#47017,#47018,#47019,#47020,#47021),.UNSPECIFIED.,.F.,.F.,(4,3,3,
3,3,3,3,4),(32.5308085451138,32.9869027667689,33.9865058809134,34.9861089950579,
35.9857121092024,36.9853152233469,37.9849183374914,38.8139938522934),
 .UNSPECIFIED.);
#11239=B_SPLINE_CURVE_WITH_KNOTS('',3,(#47026,#47027,#47028,#47029,#47030,
#47031,#47032,#47033,#47034,#47035,#47036,#47037,#47038,#47039,#47040,#47041,
#47042,#47043,#47044,#47045,#47046,#47047,#47048,#47049,#47050),
 .UNSPECIFIED.,.F.,.F.,(4,3,3,3,3,3,3,3,4),(-48.0755298702818,-47.9809494789365,
-46.981346364792,-45.9817432506475,-44.982140136503,-43.9825370223585,-42.982933908214,
-41.9833307940695,-41.7923445631022),.UNSPECIFIED.);
#11240=B_SPLINE_CURVE_WITH_KNOTS('',3,(#47051,#47052,#47053,#47054,#47055,
#47056,#47057,#47058,#47059,#47060,#47061,#47062,#47063,#47064,#47065,#47066,
#47067,#47068,#47069,#47070,#47071,#47072,#47073,#47074,#47075),
 .UNSPECIFIED.,.F.,.F.,(4,3,3,3,3,3,3,3,4),(38.8139938522934,38.9845214516359,
39.9841245657804,40.983727679925,41.9833307940695,42.982933908214,43.9825370223585,
44.982140136503,45.097179159473),.UNSPECIFIED.);
#11241=B_SPLINE_CURVE_WITH_KNOTS('',3,(#47080,#47081,#47082,#47083,#47084,
#47085,#47086,#47087,#47088,#47089,#47090,#47091,#47092,#47093,#47094,#47095,
#47096,#47097,#47098,#47099,#47100,#47101),.UNSPECIFIED.,.F.,.F.,(4,3,3,
3,3,3,3,4),(-54.3587151774614,-53.9785681638036,-52.9789650496591,-51.9793619355146,
-50.9797588213701,-49.9801557072255,-48.980552593081,-48.0755298702818),
 .UNSPECIFIED.);
#11242=B_SPLINE_CURVE_WITH_KNOTS('',3,(#47102,#47103,#47104,#47105,#47106,
#47107,#47108,#47109,#47110,#47111,#47112,#47113,#47114,#47115,#47116,#47117,
#47118,#47119,#47120,#47121,#47122,#47123),.UNSPECIFIED.,.F.,.F.,(4,3,3,
3,3,3,3,4),(45.097179159473,45.9817432506475,46.981346364792,47.9809494789365,
48.980552593081,49.9801557072255,50.97975882137,51.3803644666526),
 .UNSPECIFIED.);
#11243=B_SPLINE_CURVE_WITH_KNOTS('',3,(#47128,#47129,#47130,#47131,#47132,
#47133,#47134,#47135,#47136,#47137,#47138,#47139,#47140,#47141,#47142,#47143,
#47144,#47145,#47146,#47147,#47148,#47149),.UNSPECIFIED.,.F.,.F.,(4,3,3,
3,3,3,3,4),(-60.641900484641,-59.9761868486707,-58.9765837345262,-57.9769806203817,
-56.9773775062371,-55.9777743920926,-54.9781712779481,-54.3587151774614),
 .UNSPECIFIED.);
#11244=B_SPLINE_CURVE_WITH_KNOTS('',3,(#47150,#47151,#47152,#47153,#47154,
#47155,#47156,#47157,#47158,#47159,#47160,#47161,#47162,#47163,#47164,#47165,
#47166,#47167,#47168,#47169,#47170,#47171),.UNSPECIFIED.,.F.,.F.,(4,3,3,
3,3,3,3,4),(51.3803644666526,51.9793619355146,52.9789650496591,53.9785681638036,
54.9781712779481,55.9777743920926,56.9773775062371,57.6635497738322),
 .UNSPECIFIED.);
#11245=B_SPLINE_CURVE_WITH_KNOTS('',3,(#47176,#47177,#47178,#47179,#47180,
#47181,#47182,#47183,#47184,#47185,#47186,#47187,#47188,#47189,#47190,#47191,
#47192,#47193,#47194,#47195,#47196,#47197),.UNSPECIFIED.,.F.,.F.,(4,3,3,
3,3,3,3,4),(-66.9250857918206,-65.9738055335377,-64.9742024193932,-63.9745993052487,
-62.9749961911042,-61.9753930769597,-60.9757899628152,-60.641900484641),
 .UNSPECIFIED.);
#11246=B_SPLINE_CURVE_WITH_KNOTS('',3,(#47198,#47199,#47200,#47201,#47202,
#47203,#47204,#47205,#47206,#47207,#47208,#47209,#47210,#47211,#47212,#47213,
#47214,#47215,#47216,#47217,#47218,#47219),.UNSPECIFIED.,.F.,.F.,(4,3,3,
3,3,3,3,4),(57.6635497738322,57.9769806203816,58.9765837345261,59.9761868486707,
60.9757899628152,61.9753930769597,62.9749961911042,63.9467350810118),
 .UNSPECIFIED.);
#11247=B_SPLINE_CURVE_WITH_KNOTS('',3,(#47224,#47225,#47226,#47227,#47228,
#47229,#47230,#47231,#47232,#47233,#47234,#47235,#47236,#47237,#47238,#47239,
#47240,#47241,#47242,#47243,#47244,#47245,#47246,#47247,#47248),
 .UNSPECIFIED.,.F.,.F.,(4,3,3,3,3,3,3,3,4),(-73.2082710990002,-72.9710273325493,
-71.9714242184048,-70.9718211042603,-69.9722179901158,-68.9726148759713,
-67.9730117618268,-66.9734086476822,-66.9250857918206),.UNSPECIFIED.);
#11248=B_SPLINE_CURVE_WITH_KNOTS('',3,(#47249,#47250,#47251,#47252,#47253,
#47254,#47255,#47256,#47257,#47258,#47259,#47260,#47261,#47262,#47263,#47264,
#47265,#47266,#47267,#47268,#47269,#47270,#47271,#47272,#47273),
 .UNSPECIFIED.,.F.,.F.,(4,3,3,3,3,3,3,3,4),(63.9467350810118,63.9745993052487,
64.9742024193932,65.9738055335377,66.9734086476822,67.9730117618267,68.9726148759712,
69.9722179901158,70.2299203881913),.UNSPECIFIED.);
#11249=B_SPLINE_CURVE_WITH_KNOTS('',3,(#47278,#47279,#47280,#47281,#47282,
#47283,#47284,#47285,#47286,#47287,#47288,#47289,#47290,#47291,#47292,#47293,
#47294,#47295,#47296,#47297,#47298,#47299),.UNSPECIFIED.,.F.,.F.,(4,3,3,
3,3,3,3,4),(-79.4914564061798,-78.9686460174164,-77.9690429032719,-76.9694397891273,
-75.9698366749828,-74.9702335608383,-73.9706304466938,-73.2082710990002),
 .UNSPECIFIED.);
#11250=B_SPLINE_CURVE_WITH_KNOTS('',3,(#47300,#47301,#47302,#47303,#47304,
#47305,#47306,#47307,#47308,#47309,#47310,#47311,#47312,#47313,#47314,#47315,
#47316,#47317,#47318,#47319,#47320,#47321),.UNSPECIFIED.,.F.,.F.,(4,3,3,
3,3,3,3,4),(70.2299203881913,70.9718211042603,71.9714242184048,72.9710273325493,
73.9706304466938,74.9702335608383,75.9698366749828,76.5131056953709),
 .UNSPECIFIED.);
#11251=B_SPLINE_CURVE_WITH_KNOTS('',3,(#47326,#47327,#47328,#47329,#47330,
#47331,#47332,#47333,#47334,#47335,#47336,#47337,#47338,#47339,#47340,#47341,
#47342,#47343,#47344,#47345,#47346,#47347),.UNSPECIFIED.,.F.,.F.,(4,3,3,
3,3,3,3,4),(-85.7746417133594,-84.9662647022835,-83.9666615881389,-82.9670584739944,
-81.9674553598499,-80.9678522457054,-79.9682491315609,-79.4914564061798),
 .UNSPECIFIED.);
#11252=B_SPLINE_CURVE_WITH_KNOTS('',3,(#47348,#47349,#47350,#47351,#47352,
#47353,#47354,#47355,#47356,#47357,#47358,#47359,#47360,#47361,#47362,#47363,
#47364,#47365,#47366,#47367,#47368,#47369),.UNSPECIFIED.,.F.,.F.,(4,3,3,
3,3,3,3,4),(76.5131056953709,76.9694397891273,77.9690429032718,78.9686460174164,
79.9682491315609,80.9678522457054,81.9674553598499,82.7962910025505),
 .UNSPECIFIED.);
#11253=B_SPLINE_CURVE_WITH_KNOTS('',3,(#47374,#47375,#47376,#47377,#47378,
#47379,#47380,#47381,#47382,#47383,#47384,#47385,#47386,#47387,#47388,#47389,
#47390,#47391,#47392,#47393,#47394,#47395,#47396,#47397,#47398),
 .UNSPECIFIED.,.F.,.F.,(4,3,3,3,3,3,3,3,4),(-92.057827020539,-91.963486501295,
-90.9638833871505,-89.964280273006,-88.9646771588615,-87.965074044717,-86.9654709305725,
-85.965867816428,-85.7746417133594),.UNSPECIFIED.);
#11254=B_SPLINE_CURVE_WITH_KNOTS('',3,(#47399,#47400,#47401,#47402,#47403,
#47404,#47405,#47406,#47407,#47408,#47409,#47410,#47411,#47412,#47413,#47414,
#47415,#47416,#47417,#47418,#47419,#47420,#47421,#47422,#47423),
 .UNSPECIFIED.,.F.,.F.,(4,3,3,3,3,3,3,3,4),(82.7962910025505,82.9670584739944,
83.9666615881389,84.9662647022834,85.9658678164279,86.9654709305725,87.965074044717,
88.9646771588615,89.0794763097301),.UNSPECIFIED.);
#11255=B_SPLINE_CURVE_WITH_KNOTS('',3,(#47428,#47429,#47430,#47431,#47432,
#47433,#47434,#47435,#47436,#47437,#47438,#47439,#47440,#47441,#47442,#47443,
#47444,#47445,#47446,#47447,#47448,#47449),.UNSPECIFIED.,.F.,.F.,(4,3,3,
3,3,3,3,4),(-98.3410123277186,-97.9611051861621,-96.9615020720176,-95.961898957873,
-94.9622958437285,-93.962692729584,-92.9630896154395,-92.057827020539),
 .UNSPECIFIED.);
#11256=B_SPLINE_CURVE_WITH_KNOTS('',3,(#47450,#47451,#47452,#47453,#47454,
#47455,#47456,#47457,#47458,#47459,#47460,#47461,#47462,#47463,#47464,#47465,
#47466,#47467,#47468,#47469,#47470,#47471),.UNSPECIFIED.,.F.,.F.,(4,3,3,
3,3,3,3,4),(89.0794763097301,89.964280273006,90.9638833871505,91.963486501295,
92.9630896154395,93.962692729584,94.9622958437285,95.3626616169097),
 .UNSPECIFIED.);
#11257=B_SPLINE_CURVE_WITH_KNOTS('',3,(#47476,#47477,#47478,#47479,#47480,
#47481,#47482,#47483,#47484,#47485,#47486,#47487,#47488,#47489,#47490,#47491,
#47492,#47493,#47494,#47495,#47496,#47497),.UNSPECIFIED.,.F.,.F.,(4,3,3,
3,3,3,3,4),(-104.624197634898,-103.958723871029,-102.959120756885,-101.95951764274,
-100.959914528596,-99.9603114144511,-98.9607083003066,-98.3410123277186),
 .UNSPECIFIED.);
#11258=B_SPLINE_CURVE_WITH_KNOTS('',3,(#47498,#47499,#47500,#47501,#47502,
#47503,#47504,#47505,#47506,#47507,#47508,#47509,#47510,#47511,#47512,#47513,
#47514,#47515,#47516,#47517,#47518,#47519),.UNSPECIFIED.,.F.,.F.,(4,3,3,
3,3,3,3,4),(95.3626616169097,95.961898957873,96.9615020720176,97.9611051861621,
98.9607083003066,99.9603114144511,100.959914528596,101.645846924089),
 .UNSPECIFIED.);
#11259=B_SPLINE_CURVE_WITH_KNOTS('',3,(#47524,#47525,#47526,#47527,#47528,
#47529,#47530,#47531,#47532,#47533,#47534,#47535,#47536,#47537,#47538,#47539,
#47540,#47541,#47542,#47543,#47544,#47545),.UNSPECIFIED.,.F.,.F.,(4,3,3,
3,3,3,3,4),(-110.907382942078,-109.956342555896,-108.956739441752,-107.957136327607,
-106.957533213463,-105.957930099318,-104.958326985174,-104.624197634898),
 .UNSPECIFIED.);
#11260=B_SPLINE_CURVE_WITH_KNOTS('',3,(#47546,#47547,#47548,#47549,#47550,
#47551,#47552,#47553,#47554,#47555,#47556,#47557,#47558,#47559,#47560,#47561,
#47562,#47563,#47564,#47565,#47566,#47567),.UNSPECIFIED.,.F.,.F.,(4,3,3,
3,3,3,3,4),(101.645846924089,101.95951764274,102.959120756885,103.958723871029,
104.958326985174,105.957930099318,106.957533213463,107.929032231269),
 .UNSPECIFIED.);
#11261=B_SPLINE_CURVE_WITH_KNOTS('',3,(#47572,#47573,#47574,#47575,#47576,
#47577,#47578,#47579,#47580,#47581,#47582,#47583,#47584,#47585,#47586,#47587,
#47588,#47589,#47590,#47591,#47592,#47593,#47594,#47595,#47596),
 .UNSPECIFIED.,.F.,.F.,(4,3,3,3,3,3,3,3,4),(-117.190568249257,-116.953564354908,
-115.953961240763,-114.954358126619,-113.954755012474,-112.95515189833,
-111.955548784185,-110.955945670041,-110.907382942078),.UNSPECIFIED.);
#11262=B_SPLINE_CURVE_WITH_KNOTS('',3,(#47597,#47598,#47599,#47600,#47601,
#47602,#47603,#47604,#47605,#47606,#47607,#47608,#47609,#47610,#47611,#47612,
#47613,#47614,#47615,#47616,#47617,#47618,#47619,#47620,#47621),
 .UNSPECIFIED.,.F.,.F.,(4,3,3,3,3,3,3,3,4),(107.929032231269,107.957136327607,
108.956739441752,109.956342555896,110.955945670041,111.955548784185,112.95515189833,
113.954755012474,114.212217538448),.UNSPECIFIED.);
#11263=B_SPLINE_CURVE_WITH_KNOTS('',3,(#47626,#47627,#47628,#47629,#47630,
#47631,#47632,#47633,#47634,#47635,#47636,#47637,#47638,#47639,#47640,#47641,
#47642,#47643,#47644,#47645,#47646,#47647),.UNSPECIFIED.,.F.,.F.,(4,3,3,
3,3,3,3,4),(-123.473753556437,-122.951183039775,-121.95157992563,-120.951976811486,
-119.952373697341,-118.952770583197,-117.953167469052,-117.190568249257),
 .UNSPECIFIED.);
#11264=B_SPLINE_CURVE_WITH_KNOTS('',3,(#47648,#47649,#47650,#47651,#47652,
#47653,#47654,#47655,#47656,#47657,#47658,#47659,#47660,#47661,#47662,#47663,
#47664,#47665,#47666,#47667,#47668,#47669),.UNSPECIFIED.,.F.,.F.,(4,3,3,
3,3,3,3,4),(114.212217538448,114.954358126619,115.953961240763,116.953564354908,
117.953167469052,118.952770583197,119.952373697341,120.495402845628),
 .UNSPECIFIED.);
#11265=B_SPLINE_CURVE_WITH_KNOTS('',3,(#47675,#47676,#47677,#47678),
 .UNSPECIFIED.,.F.,.F.,(4,4),(135.088484104361,135.498200854482),
 .UNSPECIFIED.);
#11266=B_SPLINE_CURVE_WITH_KNOTS('',3,(#47684,#47685,#47686,#47687,#47688,
#47689,#47690,#47691,#47692,#47693),.UNSPECIFIED.,.F.,.F.,(4,1,1,1,1,1,
1,4),(128.805298797182,129.567898016976,130.567501131121,131.567104245265,
132.56670735941,133.566310473554,134.565913587699,135.088484104361),
 .UNSPECIFIED.);
#11267=B_SPLINE_CURVE_WITH_KNOTS('',3,(#47696,#47697,#47698,#47699,#47700,
#47701,#47702,#47703,#47704,#47705),.UNSPECIFIED.,.F.,.F.,(4,1,1,1,1,1,
1,4),(128.805298797182,129.261872763039,130.261475877184,131.261078991328,
132.260682105473,133.260285219617,133.760086776689,134.259888333762),
 .UNSPECIFIED.);
#11268=B_SPLINE_CURVE_WITH_KNOTS('',3,(#47710,#47711,#47712,#47713,#47714,
#47715,#47716,#47717,#47718,#47719,#47720),.UNSPECIFIED.,.F.,.F.,(4,1,1,
1,1,1,1,1,4),(122.522113490002,122.570676217965,123.570279332109,124.569882446254,
125.569485560398,126.569088674543,127.568691788687,128.568294902832,128.805298797182),
 .UNSPECIFIED.);
#11269=B_SPLINE_CURVE_WITH_KNOTS('',3,(#47721,#47722,#47723,#47724,#47725,
#47726,#47727,#47728,#47729,#47730),.UNSPECIFIED.,.F.,.F.,(4,1,1,1,1,1,
1,4),(122.522113490002,123.264254078172,124.263857192317,125.263460306461,
126.263063420606,127.26266653475,128.262269648895,128.805298797182),
 .UNSPECIFIED.);
#11270=B_SPLINE_CURVE_WITH_KNOTS('',3,(#47735,#47736,#47737,#47738,#47739,
#47740,#47741,#47742,#47743,#47744),.UNSPECIFIED.,.F.,.F.,(4,1,1,1,1,1,
1,4),(116.238928182822,116.573057533098,117.572660647242,118.572263761387,
119.571866875531,120.571469989676,121.57107310382,122.522113490002),
 .UNSPECIFIED.);
#11271=B_SPLINE_CURVE_WITH_KNOTS('',3,(#47745,#47746,#47747,#47748,#47749,
#47750,#47751,#47752,#47753,#47754,#47755),.UNSPECIFIED.,.F.,.F.,(4,1,1,
1,1,1,1,1,4),(116.238928182822,116.26703227916,117.266635393305,118.26623850745,
119.265841621594,120.265444735739,121.265047849883,122.264650964028,122.522113490002),
 .UNSPECIFIED.);
#11272=B_SPLINE_CURVE_WITH_KNOTS('',3,(#47760,#47761,#47762,#47763,#47764,
#47765,#47766,#47767,#47768,#47769),.UNSPECIFIED.,.F.,.F.,(4,1,1,1,1,1,
1,4),(109.955742875643,110.575438848231,111.575041962375,112.57464507652,
113.574248190664,114.573851304809,115.573454418953,116.238928182822),
 .UNSPECIFIED.);
#11273=B_SPLINE_CURVE_WITH_KNOTS('',3,(#47770,#47771,#47772,#47773,#47774,
#47775,#47776,#47777,#47778,#47779),.UNSPECIFIED.,.F.,.F.,(4,1,1,1,1,1,
1,4),(109.955742875643,110.269413594293,111.269016708438,112.268619822582,
113.268222936727,114.267826050871,115.267429165016,116.238928182822),
 .UNSPECIFIED.);
#11274=B_SPLINE_CURVE_WITH_KNOTS('',3,(#47784,#47785,#47786,#47787,#47788,
#47789,#47790,#47791,#47792,#47793),.UNSPECIFIED.,.F.,.F.,(4,1,1,1,1,1,
1,4),(103.672557568463,104.577820163364,105.577423277508,106.577026391653,
107.576629505797,108.576232619942,109.575835734086,109.955742875643),
 .UNSPECIFIED.);
#11275=B_SPLINE_CURVE_WITH_KNOTS('',3,(#47794,#47795,#47796,#47797,#47798,
#47799,#47800,#47801,#47802,#47803),.UNSPECIFIED.,.F.,.F.,(4,1,1,1,1,1,
1,4),(103.672557568463,104.271794909426,105.271398023571,106.271001137715,
107.27060425186,108.270207366004,109.269810480149,109.955742875643),
 .UNSPECIFIED.);
#11276=B_SPLINE_CURVE_WITH_KNOTS('',3,(#47808,#47809,#47810,#47811,#47812,
#47813,#47814,#47815,#47816,#47817,#47818),.UNSPECIFIED.,.F.,.F.,(4,1,1,
1,1,1,1,1,4),(97.3893722612836,97.5805983643521,98.5802014784966,99.5798045926411,
100.579407706786,101.57901082093,102.578613935075,103.578217049219,103.672557568463),
 .UNSPECIFIED.);
#11277=B_SPLINE_CURVE_WITH_KNOTS('',3,(#47819,#47820,#47821,#47822,#47823,
#47824,#47825,#47826,#47827,#47828),.UNSPECIFIED.,.F.,.F.,(4,1,1,1,1,1,
1,4),(97.3893722612836,98.2741762245593,99.2737793387038,100.273382452848,
101.272985566993,102.272588681137,103.272191795282,103.672557568463),
 .UNSPECIFIED.);
#11278=B_SPLINE_CURVE_WITH_KNOTS('',3,(#47833,#47834,#47835,#47836,#47837,
#47838,#47839,#47840,#47841,#47842),.UNSPECIFIED.,.F.,.F.,(4,1,1,1,1,1,
1,4),(91.106186954104,91.582979679485,92.5825827936296,93.5821859077741,
94.5817890219186,95.5813921360631,96.5809952502076,97.3893722612836),
 .UNSPECIFIED.);
#11279=B_SPLINE_CURVE_WITH_KNOTS('',3,(#47843,#47844,#47845,#47846,#47847,
#47848,#47849,#47850,#47851,#47852,#47853),.UNSPECIFIED.,.F.,.F.,(4,1,1,
1,1,1,1,1,4),(91.106186954104,91.2769544255477,92.2765575396922,93.2761606538367,
94.2757637679812,95.2753668821258,96.2749699962703,97.2745731104148,97.3893722612836),
 .UNSPECIFIED.);
#11280=B_SPLINE_CURVE_WITH_KNOTS('',3,(#47858,#47859,#47860,#47861,#47862,
#47863,#47864,#47865,#47866,#47867),.UNSPECIFIED.,.F.,.F.,(4,1,1,1,1,1,
1,4),(84.8230016469244,85.585360994618,86.5849641087625,87.584567222907,
88.5841703370515,89.583773451196,90.5833765653405,91.106186954104),
 .UNSPECIFIED.);
#11281=B_SPLINE_CURVE_WITH_KNOTS('',3,(#47868,#47869,#47870,#47871,#47872,
#47873,#47874,#47875,#47876,#47877),.UNSPECIFIED.,.F.,.F.,(4,1,1,1,1,1,
1,4),(84.8230016469244,85.2793357406806,86.2789388548251,87.2785419689697,
88.2781450831142,89.2777481972587,90.2773513114032,91.106186954104),
 .UNSPECIFIED.);
#11282=B_SPLINE_CURVE_WITH_KNOTS('',3,(#47882,#47883,#47884,#47885,#47886,
#47887,#47888,#47889,#47890,#47891,#47892),.UNSPECIFIED.,.F.,.F.,(4,1,1,
1,1,1,1,1,4),(78.5398163397448,78.5881391956064,79.5877423097509,80.5873454238954,
81.5869485380399,82.5865516521845,83.586154766329,84.5857578804735,84.8230016469244),
 .UNSPECIFIED.);
#11283=B_SPLINE_CURVE_WITH_KNOTS('',3,(#47893,#47894,#47895,#47896,#47897,
#47898,#47899,#47900,#47901,#47902),.UNSPECIFIED.,.F.,.F.,(4,1,1,1,1,1,
1,4),(78.5398163397448,79.2817170558136,80.2813201699581,81.2809232841026,
82.2805263982471,83.2801295123916,84.2797326265361,84.8230016469244),
 .UNSPECIFIED.);
#11284=B_SPLINE_CURVE_WITH_KNOTS('',3,(#47907,#47908,#47909,#47910,#47911,
#47912,#47913,#47914,#47915,#47916),.UNSPECIFIED.,.F.,.F.,(4,1,1,1,1,1,
1,4),(72.2566310325652,72.5905205107393,73.5901236248838,74.5897267390284,
75.5893298531729,76.5889329673174,77.5885360814619,78.5398163397448),
 .UNSPECIFIED.);
#11285=B_SPLINE_CURVE_WITH_KNOTS('',3,(#47917,#47918,#47919,#47920,#47921,
#47922,#47923,#47924,#47925,#47926,#47927),.UNSPECIFIED.,.F.,.F.,(4,1,1,
1,1,1,1,1,4),(72.2566310325652,72.284495256802,73.2840983709465,74.283701485091,
75.2833045992355,76.28290771338,77.2825108275245,78.2821139416691,78.5398163397448),
 .UNSPECIFIED.);
#11286=B_SPLINE_CURVE_WITH_KNOTS('',3,(#47932,#47933,#47934,#47935,#47936,
#47937,#47938,#47939,#47940,#47941),.UNSPECIFIED.,.F.,.F.,(4,1,1,1,1,1,
1,4),(65.9734457253856,66.5929018258723,67.5925049400168,68.5921080541613,
69.5917111683058,70.5913142824503,71.5909173965948,72.2566310325652),
 .UNSPECIFIED.);
#11287=B_SPLINE_CURVE_WITH_KNOTS('',3,(#47942,#47943,#47944,#47945,#47946,
#47947,#47948,#47949,#47950,#47951),.UNSPECIFIED.,.F.,.F.,(4,1,1,1,1,1,
1,4),(65.9734457253856,66.2868765719349,67.2864796860794,68.286082800224,
69.2856859143685,70.285289028513,71.2848921426575,72.2566310325652),
 .UNSPECIFIED.);
#11288=B_SPLINE_CURVE_WITH_KNOTS('',3,(#47956,#47957,#47958,#47959,#47960,
#47961,#47962,#47963,#47964,#47965),.UNSPECIFIED.,.F.,.F.,(4,1,1,1,1,1,
1,4),(59.690260418206,60.5952831410052,61.5948862551497,62.5944893692942,
63.5940924834387,64.5936955975832,65.5932987117278,65.9734457253856),
 .UNSPECIFIED.);
#11289=B_SPLINE_CURVE_WITH_KNOTS('',3,(#47966,#47967,#47968,#47969,#47970,
#47971,#47972,#47973,#47974,#47975),.UNSPECIFIED.,.F.,.F.,(4,1,1,1,1,1,
1,4),(59.690260418206,60.2892578870679,61.2888610012124,62.2884641153569,
63.2880672295014,64.2876703436459,65.2872734577904,65.9734457253856),
 .UNSPECIFIED.);
#11290=B_SPLINE_CURVE_WITH_KNOTS('',3,(#47980,#47981,#47982,#47983,#47984,
#47985,#47986,#47987,#47988,#47989,#47990),.UNSPECIFIED.,.F.,.F.,(4,1,1,
1,1,1,1,1,4),(53.4070751110264,53.5980613419936,54.5976644561381,55.5972675702826,
56.5968706844272,57.5964737985717,58.5960769127162,59.5956800268607,59.690260418206),
 .UNSPECIFIED.);
#11291=B_SPLINE_CURVE_WITH_KNOTS('',3,(#47991,#47992,#47993,#47994,#47995,
#47996,#47997,#47998,#47999,#48000),.UNSPECIFIED.,.F.,.F.,(4,1,1,1,1,1,
1,4),(53.4070751110264,54.2916392022008,55.2912423163453,56.2908454304898,
57.2904485446343,58.2900516587789,59.2896547729234,59.690260418206),
 .UNSPECIFIED.);
#11292=B_SPLINE_CURVE_WITH_KNOTS('',3,(#48005,#48006,#48007,#48008,#48009,
#48010,#48011,#48012,#48013,#48014),.UNSPECIFIED.,.F.,.F.,(4,1,1,1,1,1,
1,4),(47.1238898038469,47.6004426571266,48.6000457712711,49.5996488854156,
50.5992519995601,51.5988551137046,52.5984582278491,53.4070751110264),
 .UNSPECIFIED.);
#11293=B_SPLINE_CURVE_WITH_KNOTS('',3,(#48015,#48016,#48017,#48018,#48019,
#48020,#48021,#48022,#48023,#48024,#48025),.UNSPECIFIED.,.F.,.F.,(4,1,1,
1,1,1,1,1,4),(47.1238898038468,47.2944174031892,48.2940205173337,49.2936236314783,
50.2932267456228,51.2928298597673,52.2924329739118,53.2920360880563,53.4070751110264),
 .UNSPECIFIED.);
#11294=B_SPLINE_CURVE_WITH_KNOTS('',3,(#48030,#48031,#48032,#48033,#48034,
#48035,#48036,#48037,#48038,#48039),.UNSPECIFIED.,.F.,.F.,(4,1,1,1,1,1,
1,4),(40.8407044966673,41.6028239722595,42.602427086404,43.6020302005485,
44.601633314693,45.6012364288375,46.600839542982,47.1238898038469),
 .UNSPECIFIED.);
#11295=B_SPLINE_CURVE_WITH_KNOTS('',3,(#48040,#48041,#48042,#48043,#48044,
#48045,#48046,#48047,#48048,#48049),.UNSPECIFIED.,.F.,.F.,(4,1,1,1,1,1,
1,4),(40.8407044966672,41.2967987183222,42.2964018324667,43.2960049466112,
44.2956080607557,45.2952111749002,46.2948142890447,47.1238898038468),
 .UNSPECIFIED.);
#11296=B_SPLINE_CURVE_WITH_KNOTS('',3,(#48054,#48055,#48056,#48057,#48058,
#48059,#48060,#48061,#48062,#48063,#48064),.UNSPECIFIED.,.F.,.F.,(4,1,1,
1,1,1,1,1,4),(34.5575191894877,34.6056021732479,35.6052052873924,36.6048084015369,
37.6044115156814,38.604014629826,39.6036177439705,40.603220858115,40.8407044966673),
 .UNSPECIFIED.);
#11297=B_SPLINE_CURVE_WITH_KNOTS('',3,(#48065,#48066,#48067,#48068,#48069,
#48070,#48071,#48072,#48073,#48074),.UNSPECIFIED.,.F.,.F.,(4,1,1,1,1,1,
1,4),(34.5575191894876,35.2991800334551,36.2987831475996,37.2983862617441,
38.2979893758886,39.2975924900331,40.2971956041777,40.8407044966672),
 .UNSPECIFIED.);
#11298=B_SPLINE_CURVE_WITH_KNOTS('',3,(#48079,#48080,#48081,#48082,#48083,
#48084,#48085,#48086,#48087,#48088),.UNSPECIFIED.,.F.,.F.,(4,1,1,1,1,1,
1,4),(28.2743338823081,28.6079834883808,29.6075866025254,30.6071897166699,
31.6067928308144,32.6063959449589,33.6059990591034,34.5575191894877),
 .UNSPECIFIED.);
#11299=B_SPLINE_CURVE_WITH_KNOTS('',3,(#48089,#48090,#48091,#48092,#48093,
#48094,#48095,#48096,#48097,#48098,#48099),.UNSPECIFIED.,.F.,.F.,(4,1,1,
1,1,1,1,1,4),(28.274333882308,28.3019582344435,29.301561348588,30.3011644627325,
31.3007675768771,32.3003706910216,33.2999738051661,34.2995769193106,34.5575191894876),
 .UNSPECIFIED.);
#11300=B_SPLINE_CURVE_WITH_KNOTS('',3,(#48104,#48105,#48106,#48107,#48108,
#48109,#48110,#48111,#48112,#48113),.UNSPECIFIED.,.F.,.F.,(4,1,1,1,1,1,
1,4),(21.9911485751285,22.6103648035138,23.6099679176583,24.6095710318028,
25.6091741459473,26.6087772600918,27.6083803742363,28.2743338823081),
 .UNSPECIFIED.);
#11301=B_SPLINE_CURVE_WITH_KNOTS('',3,(#48114,#48115,#48116,#48117,#48118,
#48119,#48120,#48121,#48122,#48123),.UNSPECIFIED.,.F.,.F.,(4,1,1,1,1,1,
1,4),(21.9911485751285,22.3043395495765,23.303942663721,24.3035457778655,
25.30314889201,26.3027520061545,27.302355120299,28.274333882308),
 .UNSPECIFIED.);
#11302=B_SPLINE_CURVE_WITH_KNOTS('',3,(#48128,#48129,#48130,#48131,#48132,
#48133,#48134,#48135,#48136,#48137),.UNSPECIFIED.,.F.,.F.,(4,1,1,1,1,1,
1,4),(15.7079632679489,16.6127461186467,17.6123492327912,18.6119523469357,
19.6115554610803,20.6111585752248,21.6107616893693,21.9911485751285),
 .UNSPECIFIED.);
#11303=B_SPLINE_CURVE_WITH_KNOTS('',3,(#48138,#48139,#48140,#48141,#48142,
#48143,#48144,#48145,#48146,#48147),.UNSPECIFIED.,.F.,.F.,(4,1,1,1,1,1,
1,4),(15.7079632679489,16.3067208647094,17.3063239788539,18.3059270929984,
19.3055302071429,20.3051333212874,21.3047364354319,21.9911485751285),
 .UNSPECIFIED.);
#11304=B_SPLINE_CURVE_WITH_KNOTS('',3,(#48673,#48674,#48675,#48676,#48677,
#48678,#48679,#48680,#48681,#48682,#48683,#48684,#48685,#48686,#48687,#48688,
#48689,#48690,#48691,#48692,#48693,#48694,#48695,#48696,#48697,#48698,#48699,
#48700,#48701,#48702,#48703,#48704,#48705,#48706,#48707,#48708,#48709,#48710,
#48711,#48712,#48713,#48714,#48715,#48716,#48717,#48718,#48719,#48720,#48721,
#48722,#48723,#48724,#48725,#48726,#48727,#48728,#48729,#48730,#48731,#48732,
#48733,#48734,#48735,#48736,#48737,#48738,#48739,#48740,#48741,#48742,#48743,
#48744,#48745,#48746,#48747,#48748,#48749,#48750,#48751,#48752,#48753,#48754,
#48755,#48756,#48757,#48758,#48759,#48760,#48761,#48762,#48763,#48764,#48765,
#48766,#48767,#48768,#48769,#48770,#48771,#48772,#48773,#48774,#48775),
 .UNSPECIFIED.,.F.,.F.,(4,3,3,3,3,3,3,3,3,3,3,3,3,3,3,3,3,3,3,3,3,3,3,3,
3,3,3,3,3,3,3,3,3,3,4),(-0.933975894023114,-0.900886022956469,-0.857613677956334,
-0.830917467558831,-0.811990732117496,-0.805266958984206,-0.762537705919167,
-0.721029781628806,-0.68471034787474,-0.677426067872528,-0.635390348422708,
-0.593572252555102,-0.552797767315397,-0.522216903385619,-0.510030154625355,
-0.502729037187648,-0.496839898567668,-0.456766765593561,-0.430474311596282,
-0.389892426332242,-0.34937929636466,-0.329910151917754,-0.324685557329147,
-0.285203392664255,-0.245885205074442,-0.210138932487817,-0.18387156592684,
-0.169358115925774,-0.161848011397128,-0.156162121436153,-0.117121591077115,
-0.0788937454479904,-0.0394468727239952,-0.00242854395559244,0.),
 .UNSPECIFIED.);
#11305=B_SPLINE_CURVE_WITH_KNOTS('',3,(#48776,#48777,#48778,#48779,#48780,
#48781,#48782,#48783,#48784,#48785,#48786,#48787,#48788),.UNSPECIFIED.,
 .F.,.F.,(4,3,3,3,4),(120.495402845628,120.951976811486,121.95157992563,
122.951183039775,123.883470306557),.UNSPECIFIED.);
#11306=B_SPLINE_CURVE_WITH_KNOTS('',3,(#48790,#48791,#48792,#48793,#48794,
#48795,#48796,#48797,#48798,#48799,#48800,#48801,#48802,#48803,#48804,#48805,
#48806,#48807,#48808,#48809,#48810,#48811,#48812,#48813,#48814,#48815,#48816,
#48817,#48818,#48819,#48820,#48821,#48822,#48823,#48824,#48825,#48826,#48827,
#48828,#48829,#48830,#48831,#48832,#48833,#48834,#48835,#48836,#48837,#48838,
#48839,#48840,#48841,#48842,#48843,#48844,#48845,#48846,#48847,#48848,#48849,
#48850,#48851,#48852,#48853,#48854,#48855,#48856,#48857,#48858,#48859,#48860,
#48861,#48862,#48863,#48864,#48865,#48866,#48867,#48868,#48869,#48870,#48871,
#48872,#48873,#48874,#48875,#48876,#48877,#48878,#48879,#48880,#48881,#48882,
#48883,#48884,#48885,#48886,#48887,#48888,#48889,#48890,#48891,#48892),
 .UNSPECIFIED.,.F.,.F.,(4,3,3,3,3,3,3,3,3,3,3,3,3,3,3,3,3,3,3,3,3,3,3,3,
3,3,3,3,3,3,3,3,3,3,4),(-0.937740963081769,-0.909984679133564,-0.872833882725954,
-0.847996397065448,-0.833928218367593,-0.824785785263065,-0.78663373762343,
-0.747733784440234,-0.730715054922586,-0.721961762671648,-0.713934774220468,
-0.674204019543976,-0.633909683375831,-0.593656192357265,-0.564100672307414,
-0.551648204867746,-0.54396197545851,-0.502501117350991,-0.475434112157862,
-0.435310758308129,-0.394542023824858,-0.374961735244211,-0.367483120962523,
-0.326359080771091,-0.284254421333978,-0.242709754795601,-0.212371035446151,
-0.198407867967393,-0.190923667635028,-0.185034664212022,-0.142232442426345,
-0.0988549974710058,-0.0555174255396185,-0.0127493435743661,0.),
 .UNSPECIFIED.);
#11307=B_SPLINE_CURVE_WITH_KNOTS('',3,(#48893,#48894,#48895,#48896,#48897,
#48898,#48899,#48900,#48901),.UNSPECIFIED.,.F.,.F.,(4,1,1,1,1,1,4),(10.3764180272042,
11.3087052939868,12.3083084081313,13.3079115222759,14.3075146364204,15.3071177505649,
15.7079632679489),.UNSPECIFIED.);
#11308=B_SPLINE_CURVE_WITH_KNOTS('',3,(#48907,#48908,#48909,#48910,#48911,
#48912,#48913,#48914,#48915,#48916,#48917,#48918,#48919,#48920,#48921,#48922,
#48923,#48924,#48925,#48926,#48927,#48928,#48929,#48930,#48931,#48932,#48933,
#48934,#48935,#48936,#48937,#48938,#48939,#48940,#48941,#48942,#48943,#48944,
#48945,#48946,#48947,#48948,#48949,#48950,#48951,#48952,#48953,#48954,#48955,
#48956,#48957,#48958,#48959,#48960,#48961,#48962,#48963,#48964,#48965,#48966,
#48967,#48968,#48969,#48970,#48971,#48972,#48973,#48974,#48975,#48976,#48977,
#48978,#48979,#48980,#48981,#48982,#48983,#48984,#48985,#48986,#48987,#48988,
#48989,#48990,#48991,#48992,#48993,#48994,#48995,#48996,#48997,#48998,#48999,
#49000,#49001,#49002,#49003,#49004,#49005,#49006,#49007,#49008,#49009),
 .UNSPECIFIED.,.F.,.F.,(4,3,3,3,3,3,3,3,3,3,3,3,3,3,3,3,3,3,3,3,3,3,3,3,
3,3,3,3,3,3,3,3,3,3,4),(-0.933975894023115,-0.90088602295648,-0.857613686561679,
-0.830917475626341,-0.811990735770248,-0.805266957540168,-0.762537700650808,
-0.72102977701899,-0.684710343841149,-0.67742606502949,-0.635390295376529,
-0.593572109506116,-0.552797660028653,-0.522216822920556,-0.510030127654026,
-0.502728981266388,-0.496839893719554,-0.456766643291822,-0.430474311596264,
-0.389892498153584,-0.349379548247307,-0.329910675083222,-0.324686090829592,
-0.285204009769594,-0.24588601906745,-0.210138932487834,-0.183871565926854,
-0.169358141411446,-0.161848180179082,-0.156162148451424,-0.117121611338568,
-0.0788936961114827,-0.0394468480557413,-0.00242847333026767,0.),
 .UNSPECIFIED.);
#11309=B_SPLINE_CURVE_WITH_KNOTS('',3,(#49012,#49013,#49014,#49015,#49016,
#49017,#49018,#49019,#49020),.UNSPECIFIED.,.F.,.F.,(4,1,1,1,1,1,4),(11.6147305479242,
12.1145321049964,12.6143336620687,13.6139367762132,14.6135398903577,15.6131430045022,
15.7079632679489),.UNSPECIFIED.);
#11310=B_SPLINE_CURVE_WITH_KNOTS('',3,(#49546,#49547,#49548,#49549,#49550,
#49551,#49552,#49553,#49554,#49555,#49556,#49557,#49558,#49559,#49560,#49561,
#49562,#49563,#49564,#49565,#49566,#49567,#49568,#49569,#49570,#49571,#49572,
#49573,#49574,#49575,#49576,#49577,#49578,#49579,#49580,#49581,#49582,#49583,
#49584,#49585,#49586,#49587,#49588,#49589,#49590,#49591,#49592,#49593,#49594,
#49595,#49596,#49597,#49598,#49599,#49600,#49601,#49602,#49603,#49604,#49605,
#49606,#49607,#49608,#49609,#49610,#49611,#49612,#49613,#49614,#49615,#49616,
#49617,#49618,#49619,#49620,#49621,#49622,#49623,#49624,#49625,#49626,#49627,
#49628,#49629,#49630,#49631,#49632,#49633,#49634,#49635,#49636,#49637,#49638,
#49639,#49640,#49641,#49642,#49643,#49644,#49645,#49646,#49647,#49648),
 .UNSPECIFIED.,.F.,.F.,(4,3,3,3,3,3,3,3,3,3,3,3,3,3,3,3,3,3,3,3,3,3,3,3,
3,3,3,3,3,3,3,3,3,3,4),(-0.93774096308164,-0.909984679133421,-0.872833901724178,
-0.847996414876281,-0.833928216062254,-0.824785782258315,-0.786633754260955,
-0.747733798998064,-0.730715068570549,-0.721961765812645,-0.713934771789967,
-0.674204030030189,-0.633909683853084,-0.593656117964,-0.564100616512456,
-0.551648127597297,-0.543961983767159,-0.502501076596855,-0.475434112157824,
-0.43531058957835,-0.394541812627602,-0.374961344140611,-0.367483133322358,
-0.326358922649391,-0.284254298812646,-0.24270975479558,-0.212371035446133,
-0.198407868112275,-0.190923678285126,-0.185034666341196,-0.142232895600103,
-0.0988556198980695,-0.0555180472647553,-0.0127497906429885,0.),
 .UNSPECIFIED.);
#11311=B_SPLINE_CURVE_WITH_KNOTS('',3,(#49649,#49650,#49651,#49652,#49653,
#49654,#49655,#49656,#49657,#49658,#49659,#49660,#49661),.UNSPECIFIED.,
 .F.,.F.,(4,3,3,3,4),(-125.949992382208,-125.450190825136,-124.950389268064,
-123.950786153919,-123.473753556437),.UNSPECIFIED.);
#11312=B_SPLINE_CURVE_WITH_KNOTS('',3,(#49733,#49734,#49735,#49736,#49737,
#49738,#49739,#49740,#49741,#49742),.UNSPECIFIED.,.F.,.F.,(4,3,3,4),(-4.0932327200247,
-3.99841245657804,-2.99880934243353,-2.06652207565086),.UNSPECIFIED.);
#11313=B_SPLINE_CURVE_WITH_KNOTS('',3,(#49745,#49746,#49747,#49748,#49749,
#49750,#49751,#49752,#49753,#49754),.UNSPECIFIED.,.F.,.F.,(4,3,3,4),(0.,
0.499801557072245,0.999603114144509,1.11488200921585),.UNSPECIFIED.);
#11314=B_SPLINE_CURVE_WITH_KNOTS('',3,(#49759,#49760,#49761,#49762,#49763,
#49764,#49765,#49766,#49767,#49768,#49769,#49770,#49771,#49772,#49773,#49774,
#49775,#49776,#49777,#49778,#49779,#49780),.UNSPECIFIED.,.F.,.F.,(4,3,3,
3,3,3,3,4),(-10.3764180272043,-9.99603114144511,-8.9964280273006,-7.99682491315609,
-6.99722179901157,-5.99761868486707,-4.99801557072256,-4.0932327200247),
 .UNSPECIFIED.);
#11315=B_SPLINE_CURVE_WITH_KNOTS('',3,(#49781,#49782,#49783,#49784,#49785,
#49786,#49787,#49788,#49789,#49790,#49791,#49792,#49793,#49794,#49795,#49796,
#49797,#49798,#49799,#49800,#49801,#49802),.UNSPECIFIED.,.F.,.F.,(4,3,3,
3,3,3,3,4),(1.11488200921585,1.99920622828902,2.99880934243353,3.99841245657804,
4.99801557072255,5.99761868486706,6.99722179901157,7.39806731639545),
 .UNSPECIFIED.);
#11316=B_SPLINE_CURVE_WITH_KNOTS('',3,(#49807,#49808,#49809,#49810,#49811,
#49812,#49813,#49814,#49815,#49816,#49817,#49818,#49819,#49820,#49821,#49822,
#49823,#49824,#49825,#49826,#49827,#49828),.UNSPECIFIED.,.F.,.F.,(4,3,3,
3,3,3,3,4),(-16.6596033343839,-15.9936498263122,-14.9940467121677,-13.9944435980232,
-12.9948404838786,-11.9952373697341,-10.9956342555896,-10.3764180272043),
 .UNSPECIFIED.);
#11317=B_SPLINE_CURVE_WITH_KNOTS('',3,(#49829,#49830,#49831,#49832,#49833,
#49834,#49835,#49836,#49837,#49838,#49839,#49840,#49841,#49842,#49843,#49844,
#49845,#49846,#49847,#49848,#49849,#49850),.UNSPECIFIED.,.F.,.F.,(4,3,3,
3,3,3,3,4),(7.39806731639545,7.99682491315608,8.9964280273006,9.99603114144511,
10.9956342555896,11.9952373697341,12.9948404838786,13.681252623575),
 .UNSPECIFIED.);
#11318=B_SPLINE_CURVE_WITH_KNOTS('',3,(#49855,#49856,#49857,#49858,#49859,
#49860,#49861,#49862,#49863,#49864,#49865,#49866,#49867,#49868,#49869,#49870,
#49871,#49872,#49873,#49874,#49875,#49876),.UNSPECIFIED.,.F.,.F.,(4,3,3,
3,3,3,3,4),(-22.9427886415635,-21.9912685111792,-20.9916653970347,-19.9920622828902,
-18.9924591687457,-17.9928560546012,-16.9932529404567,-16.6596033343839),
 .UNSPECIFIED.);
#11319=B_SPLINE_CURVE_WITH_KNOTS('',3,(#49877,#49878,#49879,#49880,#49881,
#49882,#49883,#49884,#49885,#49886,#49887,#49888,#49889,#49890,#49891,#49892,
#49893,#49894,#49895,#49896,#49897,#49898),.UNSPECIFIED.,.F.,.F.,(4,3,3,
3,3,3,3,4),(13.681252623575,13.9944435980232,14.9940467121677,15.9936498263122,
16.9932529404567,17.9928560546012,18.9924591687457,19.9644379307546),
 .UNSPECIFIED.);
#11320=B_SPLINE_CURVE_WITH_KNOTS('',3,(#49903,#49904,#49905,#49906,#49907,
#49908,#49909,#49910,#49911,#49912,#49913,#49914,#49915,#49916,#49917,#49918,
#49919,#49920,#49921,#49922,#49923,#49924,#49925,#49926,#49927),
 .UNSPECIFIED.,.F.,.F.,(4,3,3,3,3,3,3,3,4),(-29.225973948743,-28.9884903101908,
-27.9888871960463,-26.9892840819018,-25.9896809677573,-24.9900778536128,
-23.9904747394683,-22.9908716253238,-22.9427886415635),.UNSPECIFIED.);
#11321=B_SPLINE_CURVE_WITH_KNOTS('',3,(#49928,#49929,#49930,#49931,#49932,
#49933,#49934,#49935,#49936,#49937,#49938,#49939,#49940,#49941,#49942,#49943,
#49944,#49945,#49946,#49947,#49948,#49949,#49950,#49951,#49952),
 .UNSPECIFIED.,.F.,.F.,(4,3,3,3,3,3,3,3,4),(19.9644379307546,19.9920622828902,
20.9916653970347,21.9912685111792,22.9908716253238,23.9904747394683,24.9900778536128,
25.9896809677573,26.2476232379342),.UNSPECIFIED.);
#11322=B_SPLINE_CURVE_WITH_KNOTS('',3,(#49957,#49958,#49959,#49960,#49961,
#49962,#49963,#49964,#49965,#49966,#49967,#49968,#49969,#49970,#49971,#49972,
#49973,#49974,#49975,#49976,#49977,#49978),.UNSPECIFIED.,.F.,.F.,(4,3,3,
3,3,3,3,4),(-35.5091592559226,-34.9861089950579,-33.9865058809134,-32.9869027667689,
-31.9872996526244,-30.9876965384798,-29.9880934243353,-29.225973948743),
 .UNSPECIFIED.);
#11323=B_SPLINE_CURVE_WITH_KNOTS('',3,(#49979,#49980,#49981,#49982,#49983,
#49984,#49985,#49986,#49987,#49988,#49989,#49990,#49991,#49992,#49993,#49994,
#49995,#49996,#49997,#49998,#49999,#50000),.UNSPECIFIED.,.F.,.F.,(4,3,3,
3,3,3,3,4),(26.2476232379342,26.9892840819018,27.9888871960463,28.9884903101908,
29.9880934243353,30.9876965384798,31.9872996526244,32.5308085451138),
 .UNSPECIFIED.);
#11324=B_SPLINE_CURVE_WITH_KNOTS('',3,(#50005,#50006,#50007,#50008,#50009,
#50010,#50011,#50012,#50013,#50014,#50015,#50016,#50017,#50018,#50019,#50020,
#50021,#50022,#50023,#50024,#50025,#50026),.UNSPECIFIED.,.F.,.F.,(4,3,3,
3,3,3,3,4),(-41.7923445631022,-40.9837276799249,-39.9841245657804,-38.9845214516359,
-37.9849183374914,-36.9853152233469,-35.9857121092024,-35.5091592559226),
 .UNSPECIFIED.);
#11325=B_SPLINE_CURVE_WITH_KNOTS('',3,(#50027,#50028,#50029,#50030,#50031,
#50032,#50033,#50034,#50035,#50036,#50037,#50038,#50039,#50040,#50041,#50042,
#50043,#50044,#50045,#50046,#50047,#50048),.UNSPECIFIED.,.F.,.F.,(4,3,3,
3,3,3,3,4),(32.5308085451138,32.9869027667689,33.9865058809134,34.9861089950579,
35.9857121092024,36.9853152233469,37.9849183374914,38.8139938522934),
 .UNSPECIFIED.);
#11326=B_SPLINE_CURVE_WITH_KNOTS('',3,(#50053,#50054,#50055,#50056,#50057,
#50058,#50059,#50060,#50061,#50062,#50063,#50064,#50065,#50066,#50067,#50068,
#50069,#50070,#50071,#50072,#50073,#50074,#50075,#50076,#50077),
 .UNSPECIFIED.,.F.,.F.,(4,3,3,3,3,3,3,3,4),(-48.0755298702818,-47.9809494789365,
-46.981346364792,-45.9817432506475,-44.982140136503,-43.9825370223585,-42.982933908214,
-41.9833307940695,-41.7923445631022),.UNSPECIFIED.);
#11327=B_SPLINE_CURVE_WITH_KNOTS('',3,(#50078,#50079,#50080,#50081,#50082,
#50083,#50084,#50085,#50086,#50087,#50088,#50089,#50090,#50091,#50092,#50093,
#50094,#50095,#50096,#50097,#50098,#50099,#50100,#50101,#50102),
 .UNSPECIFIED.,.F.,.F.,(4,3,3,3,3,3,3,3,4),(38.8139938522934,38.9845214516359,
39.9841245657804,40.983727679925,41.9833307940695,42.982933908214,43.9825370223585,
44.982140136503,45.097179159473),.UNSPECIFIED.);
#11328=B_SPLINE_CURVE_WITH_KNOTS('',3,(#50107,#50108,#50109,#50110,#50111,
#50112,#50113,#50114,#50115,#50116,#50117,#50118,#50119,#50120,#50121,#50122,
#50123,#50124,#50125,#50126,#50127,#50128),.UNSPECIFIED.,.F.,.F.,(4,3,3,
3,3,3,3,4),(-54.3587151774614,-53.9785681638036,-52.9789650496591,-51.9793619355146,
-50.9797588213701,-49.9801557072255,-48.980552593081,-48.0755298702818),
 .UNSPECIFIED.);
#11329=B_SPLINE_CURVE_WITH_KNOTS('',3,(#50129,#50130,#50131,#50132,#50133,
#50134,#50135,#50136,#50137,#50138,#50139,#50140,#50141,#50142,#50143,#50144,
#50145,#50146,#50147,#50148,#50149,#50150),.UNSPECIFIED.,.F.,.F.,(4,3,3,
3,3,3,3,4),(45.097179159473,45.9817432506475,46.981346364792,47.9809494789365,
48.980552593081,49.9801557072255,50.97975882137,51.3803644666526),
 .UNSPECIFIED.);
#11330=B_SPLINE_CURVE_WITH_KNOTS('',3,(#50155,#50156,#50157,#50158,#50159,
#50160,#50161,#50162,#50163,#50164,#50165,#50166,#50167,#50168,#50169,#50170,
#50171,#50172,#50173,#50174,#50175,#50176),.UNSPECIFIED.,.F.,.F.,(4,3,3,
3,3,3,3,4),(-60.641900484641,-59.9761868486707,-58.9765837345262,-57.9769806203817,
-56.9773775062371,-55.9777743920926,-54.9781712779481,-54.3587151774614),
 .UNSPECIFIED.);
#11331=B_SPLINE_CURVE_WITH_KNOTS('',3,(#50177,#50178,#50179,#50180,#50181,
#50182,#50183,#50184,#50185,#50186,#50187,#50188,#50189,#50190,#50191,#50192,
#50193,#50194,#50195,#50196,#50197,#50198),.UNSPECIFIED.,.F.,.F.,(4,3,3,
3,3,3,3,4),(51.3803644666526,51.9793619355146,52.9789650496591,53.9785681638036,
54.9781712779481,55.9777743920926,56.9773775062371,57.6635497738322),
 .UNSPECIFIED.);
#11332=B_SPLINE_CURVE_WITH_KNOTS('',3,(#50203,#50204,#50205,#50206,#50207,
#50208,#50209,#50210,#50211,#50212,#50213,#50214,#50215,#50216,#50217,#50218,
#50219,#50220,#50221,#50222,#50223,#50224),.UNSPECIFIED.,.F.,.F.,(4,3,3,
3,3,3,3,4),(-66.9250857918206,-65.9738055335377,-64.9742024193932,-63.9745993052487,
-62.9749961911042,-61.9753930769597,-60.9757899628152,-60.641900484641),
 .UNSPECIFIED.);
#11333=B_SPLINE_CURVE_WITH_KNOTS('',3,(#50225,#50226,#50227,#50228,#50229,
#50230,#50231,#50232,#50233,#50234,#50235,#50236,#50237,#50238,#50239,#50240,
#50241,#50242,#50243,#50244,#50245,#50246),.UNSPECIFIED.,.F.,.F.,(4,3,3,
3,3,3,3,4),(57.6635497738322,57.9769806203816,58.9765837345261,59.9761868486707,
60.9757899628152,61.9753930769597,62.9749961911042,63.9467350810118),
 .UNSPECIFIED.);
#11334=B_SPLINE_CURVE_WITH_KNOTS('',3,(#50251,#50252,#50253,#50254,#50255,
#50256,#50257,#50258,#50259,#50260,#50261,#50262,#50263,#50264,#50265,#50266,
#50267,#50268,#50269,#50270,#50271,#50272,#50273,#50274,#50275),
 .UNSPECIFIED.,.F.,.F.,(4,3,3,3,3,3,3,3,4),(-73.2082710990002,-72.9710273325493,
-71.9714242184048,-70.9718211042603,-69.9722179901158,-68.9726148759713,
-67.9730117618268,-66.9734086476822,-66.9250857918206),.UNSPECIFIED.);
#11335=B_SPLINE_CURVE_WITH_KNOTS('',3,(#50276,#50277,#50278,#50279,#50280,
#50281,#50282,#50283,#50284,#50285,#50286,#50287,#50288,#50289,#50290,#50291,
#50292,#50293,#50294,#50295,#50296,#50297,#50298,#50299,#50300),
 .UNSPECIFIED.,.F.,.F.,(4,3,3,3,3,3,3,3,4),(63.9467350810118,63.9745993052487,
64.9742024193932,65.9738055335377,66.9734086476822,67.9730117618267,68.9726148759712,
69.9722179901158,70.2299203881913),.UNSPECIFIED.);
#11336=B_SPLINE_CURVE_WITH_KNOTS('',3,(#50305,#50306,#50307,#50308,#50309,
#50310,#50311,#50312,#50313,#50314,#50315,#50316,#50317,#50318,#50319,#50320,
#50321,#50322,#50323,#50324,#50325,#50326),.UNSPECIFIED.,.F.,.F.,(4,3,3,
3,3,3,3,4),(-79.4914564061798,-78.9686460174164,-77.9690429032719,-76.9694397891273,
-75.9698366749828,-74.9702335608383,-73.9706304466938,-73.2082710990002),
 .UNSPECIFIED.);
#11337=B_SPLINE_CURVE_WITH_KNOTS('',3,(#50327,#50328,#50329,#50330,#50331,
#50332,#50333,#50334,#50335,#50336,#50337,#50338,#50339,#50340,#50341,#50342,
#50343,#50344,#50345,#50346,#50347,#50348),.UNSPECIFIED.,.F.,.F.,(4,3,3,
3,3,3,3,4),(70.2299203881913,70.9718211042603,71.9714242184048,72.9710273325493,
73.9706304466938,74.9702335608383,75.9698366749828,76.5131056953709),
 .UNSPECIFIED.);
#11338=B_SPLINE_CURVE_WITH_KNOTS('',3,(#50353,#50354,#50355,#50356,#50357,
#50358,#50359,#50360,#50361,#50362,#50363,#50364,#50365,#50366,#50367,#50368,
#50369,#50370,#50371,#50372,#50373,#50374),.UNSPECIFIED.,.F.,.F.,(4,3,3,
3,3,3,3,4),(-85.7746417133594,-84.9662647022835,-83.9666615881389,-82.9670584739944,
-81.9674553598499,-80.9678522457054,-79.9682491315609,-79.4914564061798),
 .UNSPECIFIED.);
#11339=B_SPLINE_CURVE_WITH_KNOTS('',3,(#50375,#50376,#50377,#50378,#50379,
#50380,#50381,#50382,#50383,#50384,#50385,#50386,#50387,#50388,#50389,#50390,
#50391,#50392,#50393,#50394,#50395,#50396),.UNSPECIFIED.,.F.,.F.,(4,3,3,
3,3,3,3,4),(76.5131056953709,76.9694397891273,77.9690429032718,78.9686460174164,
79.9682491315609,80.9678522457054,81.9674553598499,82.7962910025505),
 .UNSPECIFIED.);
#11340=B_SPLINE_CURVE_WITH_KNOTS('',3,(#50401,#50402,#50403,#50404,#50405,
#50406,#50407,#50408,#50409,#50410,#50411,#50412,#50413,#50414,#50415,#50416,
#50417,#50418,#50419,#50420,#50421,#50422,#50423,#50424,#50425),
 .UNSPECIFIED.,.F.,.F.,(4,3,3,3,3,3,3,3,4),(-92.057827020539,-91.963486501295,
-90.9638833871505,-89.964280273006,-88.9646771588615,-87.965074044717,-86.9654709305725,
-85.965867816428,-85.7746417133594),.UNSPECIFIED.);
#11341=B_SPLINE_CURVE_WITH_KNOTS('',3,(#50426,#50427,#50428,#50429,#50430,
#50431,#50432,#50433,#50434,#50435,#50436,#50437,#50438,#50439,#50440,#50441,
#50442,#50443,#50444,#50445,#50446,#50447,#50448,#50449,#50450),
 .UNSPECIFIED.,.F.,.F.,(4,3,3,3,3,3,3,3,4),(82.7962910025505,82.9670584739944,
83.9666615881389,84.9662647022834,85.9658678164279,86.9654709305725,87.965074044717,
88.9646771588615,89.0794763097301),.UNSPECIFIED.);
#11342=B_SPLINE_CURVE_WITH_KNOTS('',3,(#50455,#50456,#50457,#50458,#50459,
#50460,#50461,#50462,#50463,#50464,#50465,#50466,#50467,#50468,#50469,#50470,
#50471,#50472,#50473,#50474,#50475,#50476),.UNSPECIFIED.,.F.,.F.,(4,3,3,
3,3,3,3,4),(-98.3410123277186,-97.9611051861621,-96.9615020720176,-95.961898957873,
-94.9622958437285,-93.962692729584,-92.9630896154395,-92.057827020539),
 .UNSPECIFIED.);
#11343=B_SPLINE_CURVE_WITH_KNOTS('',3,(#50477,#50478,#50479,#50480,#50481,
#50482,#50483,#50484,#50485,#50486,#50487,#50488,#50489,#50490,#50491,#50492,
#50493,#50494,#50495,#50496,#50497,#50498),.UNSPECIFIED.,.F.,.F.,(4,3,3,
3,3,3,3,4),(89.0794763097301,89.964280273006,90.9638833871505,91.963486501295,
92.9630896154395,93.962692729584,94.9622958437285,95.3626616169097),
 .UNSPECIFIED.);
#11344=B_SPLINE_CURVE_WITH_KNOTS('',3,(#50503,#50504,#50505,#50506,#50507,
#50508,#50509,#50510,#50511,#50512,#50513,#50514,#50515,#50516,#50517,#50518,
#50519,#50520,#50521,#50522,#50523,#50524),.UNSPECIFIED.,.F.,.F.,(4,3,3,
3,3,3,3,4),(-104.624197634898,-103.958723871029,-102.959120756885,-101.95951764274,
-100.959914528596,-99.9603114144511,-98.9607083003066,-98.3410123277186),
 .UNSPECIFIED.);
#11345=B_SPLINE_CURVE_WITH_KNOTS('',3,(#50525,#50526,#50527,#50528,#50529,
#50530,#50531,#50532,#50533,#50534,#50535,#50536,#50537,#50538,#50539,#50540,
#50541,#50542,#50543,#50544,#50545,#50546),.UNSPECIFIED.,.F.,.F.,(4,3,3,
3,3,3,3,4),(95.3626616169097,95.961898957873,96.9615020720176,97.9611051861621,
98.9607083003066,99.9603114144511,100.959914528596,101.645846924089),
 .UNSPECIFIED.);
#11346=B_SPLINE_CURVE_WITH_KNOTS('',3,(#50551,#50552,#50553,#50554,#50555,
#50556,#50557,#50558,#50559,#50560,#50561,#50562,#50563,#50564,#50565,#50566,
#50567,#50568,#50569,#50570,#50571,#50572),.UNSPECIFIED.,.F.,.F.,(4,3,3,
3,3,3,3,4),(-110.907382942078,-109.956342555896,-108.956739441752,-107.957136327607,
-106.957533213463,-105.957930099318,-104.958326985174,-104.624197634898),
 .UNSPECIFIED.);
#11347=B_SPLINE_CURVE_WITH_KNOTS('',3,(#50573,#50574,#50575,#50576,#50577,
#50578,#50579,#50580,#50581,#50582,#50583,#50584,#50585,#50586,#50587,#50588,
#50589,#50590,#50591,#50592,#50593,#50594),.UNSPECIFIED.,.F.,.F.,(4,3,3,
3,3,3,3,4),(101.645846924089,101.95951764274,102.959120756885,103.958723871029,
104.958326985174,105.957930099318,106.957533213463,107.929032231269),
 .UNSPECIFIED.);
#11348=B_SPLINE_CURVE_WITH_KNOTS('',3,(#50599,#50600,#50601,#50602,#50603,
#50604,#50605,#50606,#50607,#50608,#50609,#50610,#50611,#50612,#50613,#50614,
#50615,#50616,#50617,#50618,#50619,#50620,#50621,#50622,#50623),
 .UNSPECIFIED.,.F.,.F.,(4,3,3,3,3,3,3,3,4),(-117.190568249257,-116.953564354908,
-115.953961240763,-114.954358126619,-113.954755012474,-112.95515189833,
-111.955548784185,-110.955945670041,-110.907382942078),.UNSPECIFIED.);
#11349=B_SPLINE_CURVE_WITH_KNOTS('',3,(#50624,#50625,#50626,#50627,#50628,
#50629,#50630,#50631,#50632,#50633,#50634,#50635,#50636,#50637,#50638,#50639,
#50640,#50641,#50642,#50643,#50644,#50645,#50646,#50647,#50648),
 .UNSPECIFIED.,.F.,.F.,(4,3,3,3,3,3,3,3,4),(107.929032231269,107.957136327607,
108.956739441752,109.956342555896,110.955945670041,111.955548784185,112.95515189833,
113.954755012474,114.212217538448),.UNSPECIFIED.);
#11350=B_SPLINE_CURVE_WITH_KNOTS('',3,(#50653,#50654,#50655,#50656,#50657,
#50658,#50659,#50660,#50661,#50662,#50663,#50664,#50665,#50666,#50667,#50668,
#50669,#50670,#50671,#50672,#50673,#50674),.UNSPECIFIED.,.F.,.F.,(4,3,3,
3,3,3,3,4),(-123.473753556437,-122.951183039775,-121.95157992563,-120.951976811486,
-119.952373697341,-118.952770583197,-117.953167469052,-117.190568249257),
 .UNSPECIFIED.);
#11351=B_SPLINE_CURVE_WITH_KNOTS('',3,(#50675,#50676,#50677,#50678,#50679,
#50680,#50681,#50682,#50683,#50684,#50685,#50686,#50687,#50688,#50689,#50690,
#50691,#50692,#50693,#50694,#50695,#50696),.UNSPECIFIED.,.F.,.F.,(4,3,3,
3,3,3,3,4),(114.212217538448,114.954358126619,115.953961240763,116.953564354908,
117.953167469052,118.952770583197,119.952373697341,120.495402845628),
 .UNSPECIFIED.);
#11352=B_SPLINE_CURVE_WITH_KNOTS('',3,(#50702,#50703,#50704,#50705),
 .UNSPECIFIED.,.F.,.F.,(4,4),(135.088484104361,135.498200854482),
 .UNSPECIFIED.);
#11353=B_SPLINE_CURVE_WITH_KNOTS('',3,(#50711,#50712,#50713,#50714,#50715,
#50716,#50717,#50718,#50719,#50720),.UNSPECIFIED.,.F.,.F.,(4,1,1,1,1,1,
1,4),(128.805298797182,129.567898016976,130.567501131121,131.567104245265,
132.56670735941,133.566310473554,134.565913587699,135.088484104361),
 .UNSPECIFIED.);
#11354=B_SPLINE_CURVE_WITH_KNOTS('',3,(#50723,#50724,#50725,#50726,#50727,
#50728,#50729,#50730,#50731,#50732),.UNSPECIFIED.,.F.,.F.,(4,1,1,1,1,1,
1,4),(128.805298797182,129.261872763039,130.261475877184,131.261078991328,
132.260682105473,133.260285219617,133.760086776689,134.259888333762),
 .UNSPECIFIED.);
#11355=B_SPLINE_CURVE_WITH_KNOTS('',3,(#50737,#50738,#50739,#50740,#50741,
#50742,#50743,#50744,#50745,#50746,#50747),.UNSPECIFIED.,.F.,.F.,(4,1,1,
1,1,1,1,1,4),(122.522113490002,122.570676217965,123.570279332109,124.569882446254,
125.569485560398,126.569088674543,127.568691788687,128.568294902832,128.805298797182),
 .UNSPECIFIED.);
#11356=B_SPLINE_CURVE_WITH_KNOTS('',3,(#50748,#50749,#50750,#50751,#50752,
#50753,#50754,#50755,#50756,#50757),.UNSPECIFIED.,.F.,.F.,(4,1,1,1,1,1,
1,4),(122.522113490002,123.264254078172,124.263857192317,125.263460306461,
126.263063420606,127.26266653475,128.262269648895,128.805298797182),
 .UNSPECIFIED.);
#11357=B_SPLINE_CURVE_WITH_KNOTS('',3,(#50762,#50763,#50764,#50765,#50766,
#50767,#50768,#50769,#50770,#50771),.UNSPECIFIED.,.F.,.F.,(4,1,1,1,1,1,
1,4),(116.238928182822,116.573057533098,117.572660647242,118.572263761387,
119.571866875531,120.571469989676,121.57107310382,122.522113490002),
 .UNSPECIFIED.);
#11358=B_SPLINE_CURVE_WITH_KNOTS('',3,(#50772,#50773,#50774,#50775,#50776,
#50777,#50778,#50779,#50780,#50781,#50782),.UNSPECIFIED.,.F.,.F.,(4,1,1,
1,1,1,1,1,4),(116.238928182822,116.26703227916,117.266635393305,118.26623850745,
119.265841621594,120.265444735739,121.265047849883,122.264650964028,122.522113490002),
 .UNSPECIFIED.);
#11359=B_SPLINE_CURVE_WITH_KNOTS('',3,(#50787,#50788,#50789,#50790,#50791,
#50792,#50793,#50794,#50795,#50796),.UNSPECIFIED.,.F.,.F.,(4,1,1,1,1,1,
1,4),(109.955742875643,110.575438848231,111.575041962375,112.57464507652,
113.574248190664,114.573851304809,115.573454418953,116.238928182822),
 .UNSPECIFIED.);
#11360=B_SPLINE_CURVE_WITH_KNOTS('',3,(#50797,#50798,#50799,#50800,#50801,
#50802,#50803,#50804,#50805,#50806),.UNSPECIFIED.,.F.,.F.,(4,1,1,1,1,1,
1,4),(109.955742875643,110.269413594293,111.269016708438,112.268619822582,
113.268222936727,114.267826050871,115.267429165016,116.238928182822),
 .UNSPECIFIED.);
#11361=B_SPLINE_CURVE_WITH_KNOTS('',3,(#50811,#50812,#50813,#50814,#50815,
#50816,#50817,#50818,#50819,#50820),.UNSPECIFIED.,.F.,.F.,(4,1,1,1,1,1,
1,4),(103.672557568463,104.577820163364,105.577423277508,106.577026391653,
107.576629505797,108.576232619942,109.575835734086,109.955742875643),
 .UNSPECIFIED.);
#11362=B_SPLINE_CURVE_WITH_KNOTS('',3,(#50821,#50822,#50823,#50824,#50825,
#50826,#50827,#50828,#50829,#50830),.UNSPECIFIED.,.F.,.F.,(4,1,1,1,1,1,
1,4),(103.672557568463,104.271794909426,105.271398023571,106.271001137715,
107.27060425186,108.270207366004,109.269810480149,109.955742875643),
 .UNSPECIFIED.);
#11363=B_SPLINE_CURVE_WITH_KNOTS('',3,(#50835,#50836,#50837,#50838,#50839,
#50840,#50841,#50842,#50843,#50844,#50845),.UNSPECIFIED.,.F.,.F.,(4,1,1,
1,1,1,1,1,4),(97.3893722612836,97.5805983643521,98.5802014784966,99.5798045926411,
100.579407706786,101.57901082093,102.578613935075,103.578217049219,103.672557568463),
 .UNSPECIFIED.);
#11364=B_SPLINE_CURVE_WITH_KNOTS('',3,(#50846,#50847,#50848,#50849,#50850,
#50851,#50852,#50853,#50854,#50855),.UNSPECIFIED.,.F.,.F.,(4,1,1,1,1,1,
1,4),(97.3893722612836,98.2741762245593,99.2737793387038,100.273382452848,
101.272985566993,102.272588681137,103.272191795282,103.672557568463),
 .UNSPECIFIED.);
#11365=B_SPLINE_CURVE_WITH_KNOTS('',3,(#50860,#50861,#50862,#50863,#50864,
#50865,#50866,#50867,#50868,#50869),.UNSPECIFIED.,.F.,.F.,(4,1,1,1,1,1,
1,4),(91.106186954104,91.582979679485,92.5825827936296,93.5821859077741,
94.5817890219186,95.5813921360631,96.5809952502076,97.3893722612836),
 .UNSPECIFIED.);
#11366=B_SPLINE_CURVE_WITH_KNOTS('',3,(#50870,#50871,#50872,#50873,#50874,
#50875,#50876,#50877,#50878,#50879,#50880),.UNSPECIFIED.,.F.,.F.,(4,1,1,
1,1,1,1,1,4),(91.106186954104,91.2769544255477,92.2765575396922,93.2761606538367,
94.2757637679812,95.2753668821258,96.2749699962703,97.2745731104148,97.3893722612836),
 .UNSPECIFIED.);
#11367=B_SPLINE_CURVE_WITH_KNOTS('',3,(#50885,#50886,#50887,#50888,#50889,
#50890,#50891,#50892,#50893,#50894),.UNSPECIFIED.,.F.,.F.,(4,1,1,1,1,1,
1,4),(84.8230016469244,85.585360994618,86.5849641087625,87.584567222907,
88.5841703370515,89.583773451196,90.5833765653405,91.106186954104),
 .UNSPECIFIED.);
#11368=B_SPLINE_CURVE_WITH_KNOTS('',3,(#50895,#50896,#50897,#50898,#50899,
#50900,#50901,#50902,#50903,#50904),.UNSPECIFIED.,.F.,.F.,(4,1,1,1,1,1,
1,4),(84.8230016469244,85.2793357406806,86.2789388548251,87.2785419689697,
88.2781450831142,89.2777481972587,90.2773513114032,91.106186954104),
 .UNSPECIFIED.);
#11369=B_SPLINE_CURVE_WITH_KNOTS('',3,(#50909,#50910,#50911,#50912,#50913,
#50914,#50915,#50916,#50917,#50918,#50919),.UNSPECIFIED.,.F.,.F.,(4,1,1,
1,1,1,1,1,4),(78.5398163397448,78.5881391956064,79.5877423097509,80.5873454238954,
81.5869485380399,82.5865516521845,83.586154766329,84.5857578804735,84.8230016469244),
 .UNSPECIFIED.);
#11370=B_SPLINE_CURVE_WITH_KNOTS('',3,(#50920,#50921,#50922,#50923,#50924,
#50925,#50926,#50927,#50928,#50929),.UNSPECIFIED.,.F.,.F.,(4,1,1,1,1,1,
1,4),(78.5398163397448,79.2817170558136,80.2813201699581,81.2809232841026,
82.2805263982471,83.2801295123916,84.2797326265361,84.8230016469244),
 .UNSPECIFIED.);
#11371=B_SPLINE_CURVE_WITH_KNOTS('',3,(#50934,#50935,#50936,#50937,#50938,
#50939,#50940,#50941,#50942,#50943),.UNSPECIFIED.,.F.,.F.,(4,1,1,1,1,1,
1,4),(72.2566310325652,72.5905205107393,73.5901236248838,74.5897267390284,
75.5893298531729,76.5889329673174,77.5885360814619,78.5398163397448),
 .UNSPECIFIED.);
#11372=B_SPLINE_CURVE_WITH_KNOTS('',3,(#50944,#50945,#50946,#50947,#50948,
#50949,#50950,#50951,#50952,#50953,#50954),.UNSPECIFIED.,.F.,.F.,(4,1,1,
1,1,1,1,1,4),(72.2566310325652,72.284495256802,73.2840983709465,74.283701485091,
75.2833045992355,76.28290771338,77.2825108275245,78.2821139416691,78.5398163397448),
 .UNSPECIFIED.);
#11373=B_SPLINE_CURVE_WITH_KNOTS('',3,(#50959,#50960,#50961,#50962,#50963,
#50964,#50965,#50966,#50967,#50968),.UNSPECIFIED.,.F.,.F.,(4,1,1,1,1,1,
1,4),(65.9734457253856,66.5929018258723,67.5925049400168,68.5921080541613,
69.5917111683058,70.5913142824503,71.5909173965948,72.2566310325652),
 .UNSPECIFIED.);
#11374=B_SPLINE_CURVE_WITH_KNOTS('',3,(#50969,#50970,#50971,#50972,#50973,
#50974,#50975,#50976,#50977,#50978),.UNSPECIFIED.,.F.,.F.,(4,1,1,1,1,1,
1,4),(65.9734457253856,66.2868765719349,67.2864796860794,68.286082800224,
69.2856859143685,70.285289028513,71.2848921426575,72.2566310325652),
 .UNSPECIFIED.);
#11375=B_SPLINE_CURVE_WITH_KNOTS('',3,(#50983,#50984,#50985,#50986,#50987,
#50988,#50989,#50990,#50991,#50992),.UNSPECIFIED.,.F.,.F.,(4,1,1,1,1,1,
1,4),(59.690260418206,60.5952831410052,61.5948862551497,62.5944893692942,
63.5940924834387,64.5936955975832,65.5932987117278,65.9734457253856),
 .UNSPECIFIED.);
#11376=B_SPLINE_CURVE_WITH_KNOTS('',3,(#50993,#50994,#50995,#50996,#50997,
#50998,#50999,#51000,#51001,#51002),.UNSPECIFIED.,.F.,.F.,(4,1,1,1,1,1,
1,4),(59.690260418206,60.2892578870679,61.2888610012124,62.2884641153569,
63.2880672295014,64.2876703436459,65.2872734577904,65.9734457253856),
 .UNSPECIFIED.);
#11377=B_SPLINE_CURVE_WITH_KNOTS('',3,(#51007,#51008,#51009,#51010,#51011,
#51012,#51013,#51014,#51015,#51016,#51017),.UNSPECIFIED.,.F.,.F.,(4,1,1,
1,1,1,1,1,4),(53.4070751110264,53.5980613419936,54.5976644561381,55.5972675702826,
56.5968706844272,57.5964737985717,58.5960769127162,59.5956800268607,59.690260418206),
 .UNSPECIFIED.);
#11378=B_SPLINE_CURVE_WITH_KNOTS('',3,(#51018,#51019,#51020,#51021,#51022,
#51023,#51024,#51025,#51026,#51027),.UNSPECIFIED.,.F.,.F.,(4,1,1,1,1,1,
1,4),(53.4070751110264,54.2916392022008,55.2912423163453,56.2908454304898,
57.2904485446343,58.2900516587789,59.2896547729234,59.690260418206),
 .UNSPECIFIED.);
#11379=B_SPLINE_CURVE_WITH_KNOTS('',3,(#51032,#51033,#51034,#51035,#51036,
#51037,#51038,#51039,#51040,#51041),.UNSPECIFIED.,.F.,.F.,(4,1,1,1,1,1,
1,4),(47.1238898038469,47.6004426571266,48.6000457712711,49.5996488854156,
50.5992519995601,51.5988551137046,52.5984582278491,53.4070751110264),
 .UNSPECIFIED.);
#11380=B_SPLINE_CURVE_WITH_KNOTS('',3,(#51042,#51043,#51044,#51045,#51046,
#51047,#51048,#51049,#51050,#51051,#51052),.UNSPECIFIED.,.F.,.F.,(4,1,1,
1,1,1,1,1,4),(47.1238898038468,47.2944174031892,48.2940205173337,49.2936236314783,
50.2932267456228,51.2928298597673,52.2924329739118,53.2920360880563,53.4070751110264),
 .UNSPECIFIED.);
#11381=B_SPLINE_CURVE_WITH_KNOTS('',3,(#51057,#51058,#51059,#51060,#51061,
#51062,#51063,#51064,#51065,#51066),.UNSPECIFIED.,.F.,.F.,(4,1,1,1,1,1,
1,4),(40.8407044966673,41.6028239722595,42.602427086404,43.6020302005485,
44.601633314693,45.6012364288375,46.600839542982,47.1238898038469),
 .UNSPECIFIED.);
#11382=B_SPLINE_CURVE_WITH_KNOTS('',3,(#51067,#51068,#51069,#51070,#51071,
#51072,#51073,#51074,#51075,#51076),.UNSPECIFIED.,.F.,.F.,(4,1,1,1,1,1,
1,4),(40.8407044966672,41.2967987183222,42.2964018324667,43.2960049466112,
44.2956080607557,45.2952111749002,46.2948142890447,47.1238898038468),
 .UNSPECIFIED.);
#11383=B_SPLINE_CURVE_WITH_KNOTS('',3,(#51081,#51082,#51083,#51084,#51085,
#51086,#51087,#51088,#51089,#51090,#51091),.UNSPECIFIED.,.F.,.F.,(4,1,1,
1,1,1,1,1,4),(34.5575191894877,34.6056021732479,35.6052052873924,36.6048084015369,
37.6044115156814,38.604014629826,39.6036177439705,40.603220858115,40.8407044966673),
 .UNSPECIFIED.);
#11384=B_SPLINE_CURVE_WITH_KNOTS('',3,(#51092,#51093,#51094,#51095,#51096,
#51097,#51098,#51099,#51100,#51101),.UNSPECIFIED.,.F.,.F.,(4,1,1,1,1,1,
1,4),(34.5575191894876,35.2991800334551,36.2987831475996,37.2983862617441,
38.2979893758886,39.2975924900331,40.2971956041777,40.8407044966672),
 .UNSPECIFIED.);
#11385=B_SPLINE_CURVE_WITH_KNOTS('',3,(#51106,#51107,#51108,#51109,#51110,
#51111,#51112,#51113,#51114,#51115),.UNSPECIFIED.,.F.,.F.,(4,1,1,1,1,1,
1,4),(28.2743338823081,28.6079834883808,29.6075866025254,30.6071897166699,
31.6067928308144,32.6063959449589,33.6059990591034,34.5575191894877),
 .UNSPECIFIED.);
#11386=B_SPLINE_CURVE_WITH_KNOTS('',3,(#51116,#51117,#51118,#51119,#51120,
#51121,#51122,#51123,#51124,#51125,#51126),.UNSPECIFIED.,.F.,.F.,(4,1,1,
1,1,1,1,1,4),(28.274333882308,28.3019582344435,29.301561348588,30.3011644627325,
31.3007675768771,32.3003706910216,33.2999738051661,34.2995769193106,34.5575191894876),
 .UNSPECIFIED.);
#11387=B_SPLINE_CURVE_WITH_KNOTS('',3,(#51131,#51132,#51133,#51134,#51135,
#51136,#51137,#51138,#51139,#51140),.UNSPECIFIED.,.F.,.F.,(4,1,1,1,1,1,
1,4),(21.9911485751285,22.6103648035138,23.6099679176583,24.6095710318028,
25.6091741459473,26.6087772600918,27.6083803742363,28.2743338823081),
 .UNSPECIFIED.);
#11388=B_SPLINE_CURVE_WITH_KNOTS('',3,(#51141,#51142,#51143,#51144,#51145,
#51146,#51147,#51148,#51149,#51150),.UNSPECIFIED.,.F.,.F.,(4,1,1,1,1,1,
1,4),(21.9911485751285,22.3043395495765,23.303942663721,24.3035457778655,
25.30314889201,26.3027520061545,27.302355120299,28.274333882308),
 .UNSPECIFIED.);
#11389=B_SPLINE_CURVE_WITH_KNOTS('',3,(#51155,#51156,#51157,#51158,#51159,
#51160,#51161,#51162,#51163,#51164),.UNSPECIFIED.,.F.,.F.,(4,1,1,1,1,1,
1,4),(15.7079632679489,16.6127461186467,17.6123492327912,18.6119523469357,
19.6115554610803,20.6111585752248,21.6107616893693,21.9911485751285),
 .UNSPECIFIED.);
#11390=B_SPLINE_CURVE_WITH_KNOTS('',3,(#51165,#51166,#51167,#51168,#51169,
#51170,#51171,#51172,#51173,#51174),.UNSPECIFIED.,.F.,.F.,(4,1,1,1,1,1,
1,4),(15.7079632679489,16.3067208647094,17.3063239788539,18.3059270929984,
19.3055302071429,20.3051333212874,21.3047364354319,21.9911485751285),
 .UNSPECIFIED.);
#11391=B_SPLINE_CURVE_WITH_KNOTS('',3,(#51700,#51701,#51702,#51703,#51704,
#51705,#51706,#51707,#51708,#51709,#51710,#51711,#51712,#51713,#51714,#51715,
#51716,#51717,#51718,#51719,#51720,#51721,#51722,#51723,#51724,#51725,#51726,
#51727,#51728,#51729,#51730,#51731,#51732,#51733,#51734,#51735,#51736,#51737,
#51738,#51739,#51740,#51741,#51742,#51743,#51744,#51745,#51746,#51747,#51748,
#51749,#51750,#51751,#51752,#51753,#51754,#51755,#51756,#51757,#51758,#51759,
#51760,#51761,#51762,#51763,#51764,#51765,#51766,#51767,#51768,#51769,#51770,
#51771,#51772,#51773,#51774,#51775,#51776,#51777,#51778,#51779,#51780,#51781,
#51782,#51783,#51784,#51785,#51786,#51787,#51788,#51789,#51790,#51791,#51792,
#51793,#51794,#51795,#51796,#51797,#51798,#51799,#51800,#51801,#51802),
 .UNSPECIFIED.,.F.,.F.,(4,3,3,3,3,3,3,3,3,3,3,3,3,3,3,3,3,3,3,3,3,3,3,3,
3,3,3,3,3,3,3,3,3,3,4),(-0.933975894023114,-0.900886022956469,-0.857613677956334,
-0.830917467558831,-0.811990732117496,-0.805266958984206,-0.762537705919167,
-0.721029781628806,-0.68471034787474,-0.677426067872528,-0.635390348422708,
-0.593572252555102,-0.552797767315397,-0.522216903385619,-0.510030154625355,
-0.502729037187648,-0.496839898567668,-0.456766765593561,-0.430474311596282,
-0.389892426332242,-0.34937929636466,-0.329910151917754,-0.324685557329147,
-0.285203392664255,-0.245885205074442,-0.210138932487817,-0.18387156592684,
-0.169358115925774,-0.161848011397128,-0.156162121436153,-0.117121591077115,
-0.0788937454479904,-0.0394468727239952,-0.00242854395559244,0.),
 .UNSPECIFIED.);
#11392=B_SPLINE_CURVE_WITH_KNOTS('',3,(#51803,#51804,#51805,#51806,#51807,
#51808,#51809,#51810,#51811,#51812,#51813,#51814,#51815),.UNSPECIFIED.,
 .F.,.F.,(4,3,3,3,4),(120.495402845628,120.951976811486,121.95157992563,
122.951183039775,123.883470306557),.UNSPECIFIED.);
#11393=B_SPLINE_CURVE_WITH_KNOTS('',3,(#51817,#51818,#51819,#51820,#51821,
#51822,#51823,#51824,#51825,#51826,#51827,#51828,#51829,#51830,#51831,#51832,
#51833,#51834,#51835,#51836,#51837,#51838,#51839,#51840,#51841,#51842,#51843,
#51844,#51845,#51846,#51847,#51848,#51849,#51850,#51851,#51852,#51853,#51854,
#51855,#51856,#51857,#51858,#51859,#51860,#51861,#51862,#51863,#51864,#51865,
#51866,#51867,#51868,#51869,#51870,#51871,#51872,#51873,#51874,#51875,#51876,
#51877,#51878,#51879,#51880,#51881,#51882,#51883,#51884,#51885,#51886,#51887,
#51888,#51889,#51890,#51891,#51892,#51893,#51894,#51895,#51896,#51897,#51898,
#51899,#51900,#51901,#51902,#51903,#51904,#51905,#51906,#51907,#51908,#51909,
#51910,#51911,#51912,#51913,#51914,#51915,#51916,#51917,#51918,#51919),
 .UNSPECIFIED.,.F.,.F.,(4,3,3,3,3,3,3,3,3,3,3,3,3,3,3,3,3,3,3,3,3,3,3,3,
3,3,3,3,3,3,3,3,3,3,4),(-0.937740963081769,-0.909984679133564,-0.872833882725954,
-0.847996397065448,-0.833928218367593,-0.824785785263065,-0.78663373762343,
-0.747733784440234,-0.730715054922586,-0.721961762671648,-0.713934774220468,
-0.674204019543976,-0.633909683375831,-0.593656192357265,-0.564100672307414,
-0.551648204867746,-0.54396197545851,-0.502501117350991,-0.475434112157862,
-0.435310758308129,-0.394542023824858,-0.374961735244211,-0.367483120962523,
-0.326359080771091,-0.284254421333978,-0.242709754795601,-0.212371035446151,
-0.198407867967393,-0.190923667635028,-0.185034664212022,-0.142232442426345,
-0.0988549974710058,-0.0555174255396185,-0.0127493435743661,0.),
 .UNSPECIFIED.);
#11394=B_SPLINE_CURVE_WITH_KNOTS('',3,(#51920,#51921,#51922,#51923,#51924,
#51925,#51926,#51927,#51928),.UNSPECIFIED.,.F.,.F.,(4,1,1,1,1,1,4),(10.3764180272042,
11.3087052939868,12.3083084081313,13.3079115222759,14.3075146364204,15.3071177505649,
15.7079632679489),.UNSPECIFIED.);
#11395=B_SPLINE_CURVE_WITH_KNOTS('',3,(#51934,#51935,#51936,#51937,#51938,
#51939,#51940,#51941,#51942,#51943,#51944,#51945,#51946,#51947,#51948,#51949,
#51950,#51951,#51952,#51953,#51954,#51955,#51956,#51957,#51958,#51959,#51960,
#51961,#51962,#51963,#51964,#51965,#51966,#51967,#51968,#51969,#51970,#51971,
#51972,#51973,#51974,#51975,#51976,#51977,#51978,#51979,#51980,#51981,#51982,
#51983,#51984,#51985,#51986,#51987,#51988,#51989,#51990,#51991,#51992,#51993,
#51994,#51995,#51996,#51997,#51998,#51999,#52000,#52001,#52002,#52003,#52004,
#52005,#52006,#52007,#52008,#52009,#52010,#52011,#52012,#52013,#52014,#52015,
#52016,#52017,#52018,#52019,#52020,#52021,#52022,#52023,#52024,#52025,#52026,
#52027,#52028,#52029,#52030,#52031,#52032,#52033,#52034,#52035,#52036),
 .UNSPECIFIED.,.F.,.F.,(4,3,3,3,3,3,3,3,3,3,3,3,3,3,3,3,3,3,3,3,3,3,3,3,
3,3,3,3,3,3,3,3,3,3,4),(-0.933975894023115,-0.90088602295648,-0.857613686561679,
-0.830917475626341,-0.811990735770248,-0.805266957540168,-0.762537700650808,
-0.72102977701899,-0.684710343841149,-0.67742606502949,-0.635390295376529,
-0.593572109506116,-0.552797660028653,-0.522216822920556,-0.510030127654026,
-0.502728981266388,-0.496839893719554,-0.456766643291822,-0.430474311596264,
-0.389892498153584,-0.349379548247307,-0.329910675083222,-0.324686090829592,
-0.285204009769594,-0.24588601906745,-0.210138932487834,-0.183871565926854,
-0.169358141411446,-0.161848180179082,-0.156162148451424,-0.117121611338568,
-0.0788936961114827,-0.0394468480557413,-0.00242847333026767,0.),
 .UNSPECIFIED.);
#11396=B_SPLINE_CURVE_WITH_KNOTS('',3,(#52039,#52040,#52041,#52042,#52043,
#52044,#52045,#52046,#52047),.UNSPECIFIED.,.F.,.F.,(4,1,1,1,1,1,4),(11.6147305479242,
12.1145321049964,12.6143336620687,13.6139367762132,14.6135398903577,15.6131430045022,
15.7079632679489),.UNSPECIFIED.);
#11397=B_SPLINE_CURVE_WITH_KNOTS('',3,(#52573,#52574,#52575,#52576,#52577,
#52578,#52579,#52580,#52581,#52582,#52583,#52584,#52585,#52586,#52587,#52588,
#52589,#52590,#52591,#52592,#52593,#52594,#52595,#52596,#52597,#52598,#52599,
#52600,#52601,#52602,#52603,#52604,#52605,#52606,#52607,#52608,#52609,#52610,
#52611,#52612,#52613,#52614,#52615,#52616,#52617,#52618,#52619,#52620,#52621,
#52622,#52623,#52624,#52625,#52626,#52627,#52628,#52629,#52630,#52631,#52632,
#52633,#52634,#52635,#52636,#52637,#52638,#52639,#52640,#52641,#52642,#52643,
#52644,#52645,#52646,#52647,#52648,#52649,#52650,#52651,#52652,#52653,#52654,
#52655,#52656,#52657,#52658,#52659,#52660,#52661,#52662,#52663,#52664,#52665,
#52666,#52667,#52668,#52669,#52670,#52671,#52672,#52673,#52674,#52675),
 .UNSPECIFIED.,.F.,.F.,(4,3,3,3,3,3,3,3,3,3,3,3,3,3,3,3,3,3,3,3,3,3,3,3,
3,3,3,3,3,3,3,3,3,3,4),(-0.93774096308164,-0.909984679133421,-0.872833901724178,
-0.847996414876281,-0.833928216062254,-0.824785782258315,-0.786633754260955,
-0.747733798998064,-0.730715068570549,-0.721961765812645,-0.713934771789967,
-0.674204030030189,-0.633909683853084,-0.593656117964,-0.564100616512456,
-0.551648127597297,-0.543961983767159,-0.502501076596855,-0.475434112157824,
-0.43531058957835,-0.394541812627602,-0.374961344140611,-0.367483133322358,
-0.326358922649391,-0.284254298812646,-0.24270975479558,-0.212371035446133,
-0.198407868112275,-0.190923678285126,-0.185034666341196,-0.142232895600103,
-0.0988556198980695,-0.0555180472647553,-0.0127497906429885,0.),
 .UNSPECIFIED.);
#11398=B_SPLINE_CURVE_WITH_KNOTS('',3,(#52676,#52677,#52678,#52679,#52680,
#52681,#52682,#52683,#52684,#52685,#52686,#52687,#52688),.UNSPECIFIED.,
 .F.,.F.,(4,3,3,3,4),(-125.949992382208,-125.450190825136,-124.950389268064,
-123.950786153919,-123.473753556437),.UNSPECIFIED.);
#11399=B_SPLINE_CURVE_WITH_KNOTS('',3,(#53623,#53624,#53625,#53626,#53627,
#53628,#53629,#53630,#53631,#53632),.UNSPECIFIED.,.F.,.F.,(4,3,3,4),(-4.09157007060748,
-3.98172109321816,-2.98629081991362,-2.06659765062439),.UNSPECIFIED.);
#11400=B_SPLINE_CURVE_WITH_KNOTS('',3,(#53635,#53636,#53637,#53638,#53639,
#53640,#53641),.UNSPECIFIED.,.F.,.F.,(4,3,4),(0.,0.995430273304535,1.11662023360662),
 .UNSPECIFIED.);
#11401=B_SPLINE_CURVE_WITH_KNOTS('',3,(#53646,#53647,#53648,#53649,#53650,
#53651,#53652,#53653,#53654,#53655,#53656,#53657,#53658,#53659,#53660,#53661,
#53662,#53663,#53664,#53665,#53666,#53667),.UNSPECIFIED.,.F.,.F.,(4,3,3,
3,3,3,3,4),(-10.3747553777871,-9.95430273304539,-8.95887245974085,-7.96344218643631,
-6.96801191313177,-5.97258163982723,-4.9771513665227,-4.09157007060748),
 .UNSPECIFIED.);
#11402=B_SPLINE_CURVE_WITH_KNOTS('',3,(#53668,#53669,#53670,#53671,#53672,
#53673,#53674,#53675,#53676,#53677,#53678,#53679,#53680,#53681,#53682,#53683,
#53684,#53685,#53686,#53687,#53688,#53689),.UNSPECIFIED.,.F.,.F.,(4,3,3,
3,3,3,3,4),(1.11662023360662,1.99086054660907,2.98629081991362,3.98172109321816,
4.9771513665227,5.97258163982724,6.96801191313178,7.39980554078621),
 .UNSPECIFIED.);
#11403=B_SPLINE_CURVE_WITH_KNOTS('',3,(#53694,#53695,#53696,#53697,#53698,
#53699,#53700,#53701,#53702,#53703,#53704,#53705,#53706,#53707,#53708,#53709,
#53710,#53711,#53712,#53713,#53714,#53715),.UNSPECIFIED.,.F.,.F.,(4,3,3,
3,3,3,3,4),(-16.6579406849666,-15.9268843728726,-14.9314540995681,-13.9360238262635,
-12.940593552959,-11.9451632796545,-10.9497330063499,-10.3747553777871),
 .UNSPECIFIED.);
#11404=B_SPLINE_CURVE_WITH_KNOTS('',3,(#53716,#53717,#53718,#53719,#53720,
#53721,#53722,#53723,#53724,#53725,#53726,#53727,#53728,#53729,#53730,#53731,
#53732,#53733,#53734,#53735,#53736,#53737),.UNSPECIFIED.,.F.,.F.,(4,3,3,
3,3,3,3,4),(7.39980554078621,7.96344218643632,8.95887245974086,9.9543027330454,
10.9497330063499,11.9451632796545,12.940593552959,13.6829908479658),
 .UNSPECIFIED.);
#11405=B_SPLINE_CURVE_WITH_KNOTS('',3,(#53742,#53743,#53744,#53745,#53746,
#53747,#53748,#53749,#53750,#53751,#53752,#53753,#53754,#53755,#53756,#53757,
#53758,#53759,#53760,#53761,#53762,#53763,#53764,#53765,#53766),
 .UNSPECIFIED.,.F.,.F.,(4,3,3,3,3,3,3,3,4),(-22.9411259921462,-22.8948962860044,
-21.8994660126999,-20.9040357393953,-19.9086054660908,-18.9131751927862,
-17.9177449194817,-16.9223146461772,-16.6579406849666),.UNSPECIFIED.);
#11406=B_SPLINE_CURVE_WITH_KNOTS('',3,(#53767,#53768,#53769,#53770,#53771,
#53772,#53773,#53774,#53775,#53776,#53777,#53778,#53779,#53780,#53781,#53782,
#53783,#53784,#53785,#53786,#53787,#53788,#53789,#53790,#53791),
 .UNSPECIFIED.,.F.,.F.,(4,3,3,3,3,3,3,3,4),(13.6829908479658,13.9360238262635,
14.9314540995681,15.9268843728726,16.9223146461772,17.9177449194817,18.9131751927862,
19.9086054660908,19.9661761551454),.UNSPECIFIED.);
#11407=B_SPLINE_CURVE_WITH_KNOTS('',3,(#53796,#53797,#53798,#53799,#53800,
#53801,#53802,#53803,#53804,#53805,#53806,#53807,#53808,#53809,#53810,#53811,
#53812,#53813,#53814,#53815,#53816,#53817),.UNSPECIFIED.,.F.,.F.,(4,3,3,
3,3,3,3,4),(-29.2243112993258,-28.8674779258316,-27.8720476525271,-26.8766173792226,
-25.881187105918,-24.8857568326135,-23.8903265593089,-22.9411259921462),
 .UNSPECIFIED.);
#11408=B_SPLINE_CURVE_WITH_KNOTS('',3,(#53818,#53819,#53820,#53821,#53822,
#53823,#53824,#53825,#53826,#53827,#53828,#53829,#53830,#53831,#53832,#53833,
#53834,#53835,#53836,#53837,#53838,#53839),.UNSPECIFIED.,.F.,.F.,(4,3,3,
3,3,3,3,4),(19.9661761551454,20.9040357393953,21.8994660126999,22.8948962860044,
23.8903265593089,24.8857568326135,25.881187105918,26.249361462325),
 .UNSPECIFIED.);
#11409=B_SPLINE_CURVE_WITH_KNOTS('',3,(#53844,#53845,#53846,#53847,#53848,
#53849,#53850,#53851,#53852,#53853,#53854,#53855,#53856,#53857,#53858,#53859,
#53860,#53861,#53862,#53863,#53864,#53865),.UNSPECIFIED.,.F.,.F.,(4,3,3,
3,3,3,3,4),(-35.5074966065054,-34.8400595656589,-33.8446292923543,-32.8491990190498,
-31.8537687457452,-30.8583384724407,-29.8629081991362,-29.2243112993258),
 .UNSPECIFIED.);
#11410=B_SPLINE_CURVE_WITH_KNOTS('',3,(#53866,#53867,#53868,#53869,#53870,
#53871,#53872,#53873,#53874,#53875,#53876,#53877,#53878,#53879,#53880,#53881,
#53882,#53883,#53884,#53885,#53886,#53887),.UNSPECIFIED.,.F.,.F.,(4,3,3,
3,3,3,3,4),(26.249361462325,26.8766173792225,27.8720476525271,28.8674779258316,
29.8629081991362,30.8583384724407,31.8537687457452,32.5325467695045),
 .UNSPECIFIED.);
#11411=B_SPLINE_CURVE_WITH_KNOTS('',3,(#53892,#53893,#53894,#53895,#53896,
#53897,#53898,#53899,#53900,#53901,#53902,#53903,#53904,#53905,#53906,#53907,
#53908,#53909,#53910,#53911,#53912,#53913),.UNSPECIFIED.,.F.,.F.,(4,3,3,
3,3,3,3,4),(-41.790681913685,-40.8126412054861,-39.8172109321816,-38.821780658877,
-37.8263503855725,-36.8309201122679,-35.8354898389634,-35.5074966065054),
 .UNSPECIFIED.);
#11412=B_SPLINE_CURVE_WITH_KNOTS('',3,(#53914,#53915,#53916,#53917,#53918,
#53919,#53920,#53921,#53922,#53923,#53924,#53925,#53926,#53927,#53928,#53929,
#53930,#53931,#53932,#53933,#53934,#53935),.UNSPECIFIED.,.F.,.F.,(4,3,3,
3,3,3,3,4),(32.5325467695045,32.8491990190498,33.8446292923543,34.8400595656589,
35.8354898389634,36.8309201122679,37.8263503855725,38.8157320766841),
 .UNSPECIFIED.);
#11413=B_SPLINE_CURVE_WITH_KNOTS('',3,(#53940,#53941,#53942,#53943,#53944,
#53945,#53946,#53947,#53948,#53949,#53950,#53951,#53952,#53953,#53954,#53955,
#53956,#53957,#53958,#53959,#53960,#53961,#53962,#53963,#53964),
 .UNSPECIFIED.,.F.,.F.,(4,3,3,3,3,3,3,3,4),(-48.0738672208646,-47.7806531186179,
-46.7852228453133,-45.7897925720088,-44.7943622987043,-43.7989320253997,
-42.8035017520952,-41.8080714787906,-41.790681913685),.UNSPECIFIED.);
#11414=B_SPLINE_CURVE_WITH_KNOTS('',3,(#53965,#53966,#53967,#53968,#53969,
#53970,#53971,#53972,#53973,#53974,#53975,#53976,#53977,#53978,#53979,#53980,
#53981,#53982,#53983,#53984,#53985,#53986,#53987,#53988,#53989),
 .UNSPECIFIED.,.F.,.F.,(4,3,3,3,3,3,3,3,4),(38.8157320766841,38.821780658877,
39.8172109321815,40.8126412054861,41.8080714787906,42.8035017520952,43.7989320253997,
44.7943622987042,45.0989173838637),.UNSPECIFIED.);
#11415=B_SPLINE_CURVE_WITH_KNOTS('',3,(#53994,#53995,#53996,#53997,#53998,
#53999,#54000,#54001,#54002,#54003,#54004,#54005,#54006,#54007,#54008,#54009,
#54010,#54011,#54012,#54013,#54014,#54015),.UNSPECIFIED.,.F.,.F.,(4,3,3,
3,3,3,3,4),(-54.3570525280442,-53.7532347584451,-52.7578044851406,-51.762374211836,
-50.7669439385315,-49.771513665227,-48.7760833919224,-48.0738672208646),
 .UNSPECIFIED.);
#11416=B_SPLINE_CURVE_WITH_KNOTS('',3,(#54016,#54017,#54018,#54019,#54020,
#54021,#54022,#54023,#54024,#54025,#54026,#54027,#54028,#54029,#54030,#54031,
#54032,#54033,#54034,#54035,#54036,#54037),.UNSPECIFIED.,.F.,.F.,(4,3,3,
3,3,3,3,4),(45.0989173838637,45.7897925720088,46.7852228453133,47.7806531186179,
48.7760833919224,49.7715136652269,50.7669439385315,51.3821026910433),
 .UNSPECIFIED.);
#11417=B_SPLINE_CURVE_WITH_KNOTS('',3,(#54042,#54043,#54044,#54045,#54046,
#54047,#54048,#54049,#54050,#54051,#54052,#54053,#54054,#54055,#54056,#54057,
#54058,#54059,#54060,#54061,#54062,#54063),.UNSPECIFIED.,.F.,.F.,(4,3,3,
3,3,3,3,4),(-60.6402378352238,-59.7258163982724,-58.7303861249678,-57.7349558516633,
-56.7395255783587,-55.7440953050542,-54.7486650317496,-54.3570525280442),
 .UNSPECIFIED.);
#11418=B_SPLINE_CURVE_WITH_KNOTS('',3,(#54064,#54065,#54066,#54067,#54068,
#54069,#54070,#54071,#54072,#54073,#54074,#54075,#54076,#54077,#54078,#54079,
#54080,#54081,#54082,#54083,#54084,#54085),.UNSPECIFIED.,.F.,.F.,(4,3,3,
3,3,3,3,4),(51.3821026910433,51.762374211836,52.7578044851406,53.7532347584451,
54.7486650317496,55.7440953050542,56.7395255783587,57.6652879982229),
 .UNSPECIFIED.);
#11419=B_SPLINE_CURVE_WITH_KNOTS('',3,(#54090,#54091,#54092,#54093,#54094,
#54095,#54096,#54097,#54098,#54099,#54100,#54101,#54102,#54103,#54104,#54105,
#54106,#54107,#54108,#54109,#54110,#54111,#54112,#54113,#54114),
 .UNSPECIFIED.,.F.,.F.,(4,3,3,3,3,3,3,3,4),(-66.9234231424034,-66.6938283114041,
-65.6983980380996,-64.702967764795,-63.7075374914905,-62.712107218186,-61.7166769448814,
-60.7212466715769,-60.6402378352238),.UNSPECIFIED.);
#11420=B_SPLINE_CURVE_WITH_KNOTS('',3,(#54115,#54116,#54117,#54118,#54119,
#54120,#54121,#54122,#54123,#54124,#54125,#54126,#54127,#54128,#54129,#54130,
#54131,#54132,#54133,#54134,#54135,#54136,#54137,#54138,#54139),
 .UNSPECIFIED.,.F.,.F.,(4,3,3,3,3,3,3,3,4),(57.6652879982229,57.7349558516632,
58.7303861249678,59.7258163982723,60.7212466715769,61.7166769448814,62.712107218186,
63.7075374914905,63.9484733054025),.UNSPECIFIED.);
#11421=B_SPLINE_CURVE_WITH_KNOTS('',3,(#54144,#54145,#54146,#54147,#54148,
#54149,#54150,#54151,#54152,#54153,#54154,#54155,#54156,#54157,#54158,#54159,
#54160,#54161,#54162,#54163,#54164,#54165),.UNSPECIFIED.,.F.,.F.,(4,3,3,
3,3,3,3,4),(-73.206608449583,-72.6664099512313,-71.6709796779268,-70.6755494046223,
-69.6801191313177,-68.6846888580132,-67.6892585847087,-66.9234231424034),
 .UNSPECIFIED.);
#11422=B_SPLINE_CURVE_WITH_KNOTS('',3,(#54166,#54167,#54168,#54169,#54170,
#54171,#54172,#54173,#54174,#54175,#54176,#54177,#54178,#54179,#54180,#54181,
#54182,#54183,#54184,#54185,#54186,#54187),.UNSPECIFIED.,.F.,.F.,(4,3,3,
3,3,3,3,4),(63.9484733054025,64.702967764795,65.6983980380996,66.6938283114041,
67.6892585847086,68.6846888580132,69.6801191313178,70.2316586125821),
 .UNSPECIFIED.);
#11423=B_SPLINE_CURVE_WITH_KNOTS('',3,(#54194,#54195,#54196,#54197,#54198,
#54199,#54200,#54201,#54202,#54203,#54204,#54205,#54206,#54207,#54208,#54209,
#54210,#54211,#54212),.UNSPECIFIED.,.F.,.F.,(4,3,3,3,3,3,4),(-78.6389915910586,
-77.643561317754,-76.6481310444495,-75.652700771145,-74.6572704978404,-73.6618402245359,
-73.206608449583),.UNSPECIFIED.);
#11424=B_SPLINE_CURVE_WITH_KNOTS('',3,(#54213,#54214,#54215,#54216,#54217,
#54218,#54219,#54220,#54221,#54222,#54223,#54224,#54225,#54226,#54227,#54228,
#54229,#54230,#54231,#54232,#54233,#54234),.UNSPECIFIED.,.F.,.F.,(4,3,3,
3,3,3,3,4),(70.2316586125821,70.6755494046223,71.6709796779268,72.6664099512313,
73.6618402245359,74.6572704978404,75.6527007711449,76.5148439197617),
 .UNSPECIFIED.);
#11425=B_SPLINE_CURVE_WITH_KNOTS('',3,(#54240,#54241,#54242,#54243,#54244,
#54245,#54246),.UNSPECIFIED.,.F.,.F.,(4,1,1,1,4),(84.8230016469244,85.2782334218773,
86.2736636951819,87.2690939684864,88.1887871377756),.UNSPECIFIED.);
#11426=B_SPLINE_CURVE_WITH_KNOTS('',3,(#54249,#54250,#54251,#54252,#54253,
#54254),.UNSPECIFIED.,.F.,.F.,(4,1,1,4),(84.8230016469244,84.9562887716121,
85.9517190449167,86.9471493182212),.UNSPECIFIED.);
#11427=B_SPLINE_CURVE_WITH_KNOTS('',3,(#54259,#54260,#54261,#54262,#54263,
#54264,#54265,#54266,#54267,#54268),.UNSPECIFIED.,.F.,.F.,(4,1,1,1,1,1,
1,4),(78.5398163397448,79.3056517820501,80.3010820553546,81.2965123286592,
82.2919426019637,83.2873728752682,84.2828031485728,84.8230016469244),
 .UNSPECIFIED.);
#11428=B_SPLINE_CURVE_WITH_KNOTS('',3,(#54269,#54270,#54271,#54272,#54273,
#54274,#54275,#54276,#54277,#54278),.UNSPECIFIED.,.F.,.F.,(4,1,1,1,1,1,
1,4),(78.5398163397448,78.9837071317849,79.9791374050894,80.974567678394,
81.9699979516985,82.9654282250031,83.9608584983076,84.8230016469244),
 .UNSPECIFIED.);
#11429=B_SPLINE_CURVE_WITH_KNOTS('',3,(#54283,#54284,#54285,#54286,#54287,
#54288,#54289,#54290,#54291,#54292,#54293),.UNSPECIFIED.,.F.,.F.,(4,1,1,
1,1,1,1,1,4),(72.2566310325652,72.3376398689183,73.3330701422229,74.3285004155274,
75.3239306888319,76.3193609621365,77.314791235441,78.3102215087456,78.5398163397448),
 .UNSPECIFIED.);
#11430=B_SPLINE_CURVE_WITH_KNOTS('',3,(#54294,#54295,#54296,#54297,#54298,
#54299,#54300,#54301,#54302,#54303),.UNSPECIFIED.,.F.,.F.,(4,1,1,1,1,1,
1,4),(72.2566310325652,73.0111254919577,74.0065557652622,75.0019860385667,
75.9974163118713,76.9928465851758,77.9882768584804,78.5398163397448),
 .UNSPECIFIED.);
#11431=B_SPLINE_CURVE_WITH_KNOTS('',3,(#54308,#54309,#54310,#54311,#54312,
#54313,#54314,#54315,#54316,#54317),.UNSPECIFIED.,.F.,.F.,(4,1,1,1,1,1,
1,4),(65.9734457253856,66.3650582290911,67.3604885023956,68.3559187757002,
69.3513490490047,70.3467793223092,71.3422095956138,72.2566310325652),
 .UNSPECIFIED.);
#11432=B_SPLINE_CURVE_WITH_KNOTS('',3,(#54318,#54319,#54320,#54321,#54322,
#54323,#54324,#54325,#54326,#54327,#54328),.UNSPECIFIED.,.F.,.F.,(4,1,1,
1,1,1,1,1,4),(65.9734457253856,66.0431135788259,67.0385438521304,68.033974125435,
69.0294043987395,70.0248346720441,71.0202649453486,72.0156952186531,72.2566310325652),
 .UNSPECIFIED.);
#11433=B_SPLINE_CURVE_WITH_KNOTS('',3,(#54333,#54334,#54335,#54336,#54337,
#54338,#54339,#54340,#54341,#54342),.UNSPECIFIED.,.F.,.F.,(4,1,1,1,1,1,
1,4),(59.6902604182061,60.3924765892639,61.3879068625684,62.3833371358729,
63.3787674091775,64.374197682482,65.3696279557865,65.9734457253856),
 .UNSPECIFIED.);
#11434=B_SPLINE_CURVE_WITH_KNOTS('',3,(#54343,#54344,#54345,#54346,#54347,
#54348,#54349,#54350,#54351,#54352),.UNSPECIFIED.,.F.,.F.,(4,1,1,1,1,1,
1,4),(59.690260418206,60.0705319389987,61.0659622123032,62.0613924856077,
63.0568227589123,64.0522530322168,65.0476833055214,65.9734457253856),
 .UNSPECIFIED.);
#11435=B_SPLINE_CURVE_WITH_KNOTS('',3,(#54357,#54358,#54359,#54360,#54361,
#54362,#54363,#54364,#54365,#54366,#54367),.UNSPECIFIED.,.F.,.F.,(4,1,1,
1,1,1,1,1,4),(53.4070751110265,53.4244646761321,54.4198949494366,55.4153252227412,
56.4107554960457,57.4061857693502,58.4016160426548,59.3970463159593,59.6902604182061),
 .UNSPECIFIED.);
#11436=B_SPLINE_CURVE_WITH_KNOTS('',3,(#54368,#54369,#54370,#54371,#54372,
#54373,#54374,#54375,#54376,#54377),.UNSPECIFIED.,.F.,.F.,(4,1,1,1,1,1,
1,4),(53.4070751110264,54.0979502991714,55.093380572476,56.0888108457805,
57.084241119085,58.0796713923896,59.0751016656941,59.690260418206),
 .UNSPECIFIED.);
#11437=B_SPLINE_CURVE_WITH_KNOTS('',3,(#54382,#54383,#54384,#54385,#54386,
#54387,#54388,#54389,#54390,#54391),.UNSPECIFIED.,.F.,.F.,(4,1,1,1,1,1,
1,4),(47.1238898038469,47.4518830363048,48.4473133096094,49.4427435829139,
50.4381738562185,51.433604129523,52.4290344028275,53.4070751110265),
 .UNSPECIFIED.);
#11438=B_SPLINE_CURVE_WITH_KNOTS('',3,(#54392,#54393,#54394,#54395,#54396,
#54397,#54398,#54399,#54400,#54401,#54402),.UNSPECIFIED.,.F.,.F.,(4,1,1,
1,1,1,1,1,4),(47.1238898038468,47.1299383860397,48.1253686593442,49.1207989326487,
50.1162292059533,51.1116594792578,52.1070897525623,53.1025200258669,53.4070751110264),
 .UNSPECIFIED.);
#11439=B_SPLINE_CURVE_WITH_KNOTS('',3,(#54407,#54408,#54409,#54410,#54411,
#54412,#54413,#54414,#54415,#54416),.UNSPECIFIED.,.F.,.F.,(4,1,1,1,1,1,
1,4),(40.8407044966673,41.4793013964776,42.4747316697821,43.4701619430867,
44.4655922163912,45.4610224896958,46.4564527630003,47.1238898038469),
 .UNSPECIFIED.);
#11440=B_SPLINE_CURVE_WITH_KNOTS('',3,(#54417,#54418,#54419,#54420,#54421,
#54422,#54423,#54424,#54425,#54426),.UNSPECIFIED.,.F.,.F.,(4,1,1,1,1,1,
1,4),(40.8407044966673,41.1573567462124,42.152787019517,43.1482172928215,
44.143647566126,45.1390778394306,46.1345081127351,47.1238898038468),
 .UNSPECIFIED.);
#11441=B_SPLINE_CURVE_WITH_KNOTS('',3,(#54431,#54432,#54433,#54434,#54435,
#54436,#54437,#54438,#54439,#54440),.UNSPECIFIED.,.F.,.F.,(4,1,1,1,1,1,
1,4),(34.5575191894877,35.5067197566504,36.5021500299549,37.4975803032595,
38.493010576564,39.4884408498685,40.4838711231731,40.8407044966673),
 .UNSPECIFIED.);
#11442=B_SPLINE_CURVE_WITH_KNOTS('',3,(#54441,#54442,#54443,#54444,#54445,
#54446,#54447,#54448,#54449,#54450),.UNSPECIFIED.,.F.,.F.,(4,1,1,1,1,1,
1,4),(34.5575191894877,35.1847751063852,36.1802053796897,37.1756356529943,
38.1710659262988,39.1664961996033,40.1619264729079,40.8407044966673),
 .UNSPECIFIED.);
#11443=B_SPLINE_CURVE_WITH_KNOTS('',3,(#54455,#54456,#54457,#54458,#54459,
#54460,#54461,#54462,#54463,#54464,#54465),.UNSPECIFIED.,.F.,.F.,(4,1,1,
1,1,1,1,1,4),(28.2743338823081,28.5387078435186,29.5341381168231,30.5295683901277,
31.5249986634322,32.5204289367368,33.5158592100413,34.5112894833458,34.5575191894877),
 .UNSPECIFIED.);
#11444=B_SPLINE_CURVE_WITH_KNOTS('',3,(#54466,#54467,#54468,#54469,#54470,
#54471,#54472,#54473,#54474,#54475),.UNSPECIFIED.,.F.,.F.,(4,1,1,1,1,1,
1,4),(28.2743338823081,29.212193466558,30.2076237398625,31.203054013167,
32.1984842864716,33.1939145597761,34.1893448330807,34.5575191894877),
 .UNSPECIFIED.);
#11445=B_SPLINE_CURVE_WITH_KNOTS('',3,(#54480,#54481,#54482,#54483,#54484,
#54485,#54486,#54487,#54488,#54489),.UNSPECIFIED.,.F.,.F.,(4,1,1,1,1,1,
1,4),(21.9911485751285,22.5661262036914,23.5615564769959,24.5569867503004,
25.552417023605,26.5478472969095,27.5432775702141,28.2743338823081),
 .UNSPECIFIED.);
#11446=B_SPLINE_CURVE_WITH_KNOTS('',3,(#54490,#54491,#54492,#54493,#54494,
#54495,#54496,#54497,#54498,#54499,#54500),.UNSPECIFIED.,.F.,.F.,(4,1,1,
1,1,1,1,1,4),(21.9911485751285,22.2441815534262,23.2396118267307,24.2350421000353,
25.2304723733398,26.2259026466443,27.2213329199489,28.2167631932534,28.2743338823081),
 .UNSPECIFIED.);
#11447=B_SPLINE_CURVE_WITH_KNOTS('',3,(#54505,#54506,#54507,#54508,#54509,
#54510,#54511,#54512,#54513,#54514),.UNSPECIFIED.,.F.,.F.,(4,1,1,1,1,1,
1,4),(15.7079632679489,16.5935445638641,17.5889748371687,18.5844051104732,
19.5798353837777,20.5752656570823,21.5706959303868,21.9911485751285),
 .UNSPECIFIED.);
#11448=B_SPLINE_CURVE_WITH_KNOTS('',3,(#54515,#54516,#54517,#54518,#54519,
#54520,#54521,#54522,#54523,#54524),.UNSPECIFIED.,.F.,.F.,(4,1,1,1,1,1,
1,4),(15.7079632679489,16.271599913599,17.2670301869035,18.262460460208,
19.2578907335126,20.2533210068171,21.2487512801216,21.9911485751285),
 .UNSPECIFIED.);
#11449=B_SPLINE_CURVE_WITH_KNOTS('',3,(#54854,#54855,#54856,#54857,#54858,
#54859,#54860,#54861,#54862,#54863,#54864,#54865,#54866,#54867,#54868,#54869,
#54870,#54871,#54872,#54873,#54874,#54875,#54876,#54877,#54878,#54879,#54880,
#54881,#54882,#54883,#54884,#54885,#54886,#54887,#54888,#54889,#54890,#54891,
#54892,#54893,#54894,#54895,#54896,#54897,#54898,#54899,#54900,#54901,#54902,
#54903,#54904,#54905,#54906,#54907,#54908,#54909,#54910,#54911,#54912,#54913,
#54914,#54915,#54916,#54917,#54918,#54919,#54920,#54921,#54922,#54923,#54924,
#54925,#54926,#54927,#54928,#54929,#54930,#54931,#54932,#54933,#54934,#54935,
#54936,#54937,#54938),.UNSPECIFIED.,.F.,.F.,(4,3,3,3,3,3,3,3,3,3,3,3,3,
3,3,3,3,3,3,3,3,3,3,3,3,3,3,3,4),(-0.46178896489977,-0.443269576631881,
-0.417631722778642,-0.404721877370092,-0.398764222638072,-0.394155820681543,
-0.368772666244105,-0.349060357493822,-0.339629635278542,-0.335643839010919,
-0.310878151516634,-0.285927162697937,-0.262162840527267,-0.247926297736166,
-0.244191128511931,-0.22070382990977,-0.211074196241844,-0.187109670400446,
-0.16372096160039,-0.158787676279632,-0.135433515521448,-0.112095499914898,
-0.0891458125607591,-0.0803315743918779,-0.0766175656125797,-0.0541537985024097,
-0.0320532662641283,-0.0106598536043234,0.),.UNSPECIFIED.);
#11450=B_SPLINE_CURVE_WITH_KNOTS('',3,(#54939,#54940,#54941,#54942),
 .UNSPECIFIED.,.F.,.F.,(4,4),(76.5148439197617,76.5723939404342),
 .UNSPECIFIED.);
#11451=B_SPLINE_CURVE_WITH_KNOTS('',3,(#54944,#54945,#54946,#54947,#54948,
#54949,#54950,#54951,#54952,#54953,#54954,#54955,#54956,#54957,#54958,#54959,
#54960,#54961,#54962,#54963,#54964,#54965,#54966,#54967,#54968,#54969,#54970,
#54971,#54972,#54973,#54974,#54975,#54976,#54977,#54978,#54979,#54980,#54981,
#54982,#54983,#54984,#54985,#54986,#54987,#54988,#54989,#54990,#54991,#54992,
#54993,#54994,#54995,#54996,#54997,#54998,#54999,#55000,#55001,#55002,#55003,
#55004,#55005,#55006,#55007,#55008,#55009,#55010,#55011,#55012,#55013,#55014,
#55015,#55016,#55017,#55018,#55019,#55020,#55021,#55022,#55023,#55024,#55025,
#55026,#55027,#55028),.UNSPECIFIED.,.F.,.F.,(4,3,3,3,3,3,3,3,3,3,3,3,3,
3,3,3,3,3,3,3,3,3,3,3,3,3,3,3,4),(-0.463803050843718,-0.448467893697323,
-0.426743397417581,-0.414223922938524,-0.409751274283662,-0.387170225743088,
-0.368152587837341,-0.359003292171437,-0.354824498455266,-0.331563035795037,
-0.307429557470556,-0.289329448727194,-0.275754367169673,-0.271732612569561,
-0.267646445348118,-0.243218974605062,-0.23502912249711,-0.211434740552809,
-0.187352387065262,-0.181481954926502,-0.157053292656267,-0.132137985018908,
-0.107029339777651,-0.0963678781398328,-0.09101691238576,-0.0652788128183591,
-0.0394985536882287,-0.0142609901943899,0.),.UNSPECIFIED.);
#11452=B_SPLINE_CURVE_WITH_KNOTS('',3,(#55029,#55030,#55031,#55032,#55033,
#55034,#55035,#55036,#55037),.UNSPECIFIED.,.F.,.F.,(4,1,1,1,1,1,4),(10.374755377787,
11.2944485470763,12.2898788203808,13.2853090936853,14.2807393669899,15.2761696402944,
15.7079632679489),.UNSPECIFIED.);
#11453=B_SPLINE_CURVE_WITH_KNOTS('',3,(#55043,#55044,#55045,#55046,#55047,
#55048,#55049,#55050,#55051,#55052,#55053,#55054,#55055,#55056,#55057,#55058,
#55059,#55060,#55061,#55062,#55063,#55064,#55065,#55066,#55067,#55068,#55069,
#55070,#55071,#55072,#55073,#55074,#55075,#55076,#55077,#55078,#55079,#55080,
#55081,#55082,#55083,#55084,#55085,#55086,#55087,#55088,#55089,#55090,#55091,
#55092,#55093,#55094,#55095,#55096,#55097,#55098,#55099,#55100,#55101,#55102,
#55103,#55104,#55105,#55106,#55107,#55108,#55109,#55110,#55111,#55112,#55113,
#55114,#55115,#55116,#55117,#55118,#55119,#55120,#55121,#55122,#55123,#55124,
#55125,#55126,#55127),.UNSPECIFIED.,.F.,.F.,(4,3,3,3,3,3,3,3,3,3,3,3,3,
3,3,3,3,3,3,3,3,3,3,3,3,3,3,3,4),(-0.461788964899772,-0.44326957663188,
-0.417631722122037,-0.404721876754524,-0.398764200476566,-0.394155769220187,
-0.368772614542353,-0.349060312254788,-0.339629567665009,-0.335643823398429,
-0.31087813518458,-0.285927150448892,-0.262162811144695,-0.247926244119766,
-0.244191073680388,-0.220703763308337,-0.211074196241828,-0.187109662130682,
-0.163720954364347,-0.158787676781602,-0.135433511432081,-0.112095502700825,
-0.0891458325698699,-0.0803315769099513,-0.0766175669273989,-0.0541538125628121,
-0.0320532998196413,-0.0106599118168654,0.),.UNSPECIFIED.);
#11454=B_SPLINE_CURVE_WITH_KNOTS('',3,(#55130,#55131,#55132,#55133,#55134,
#55135,#55136,#55137),.UNSPECIFIED.,.F.,.F.,(4,1,1,1,1,4),(11.6163931973414,
12.611823470646,13.6072537439505,14.6026840172551,15.5981142905596,15.7079632679489),
 .UNSPECIFIED.);
#11455=B_SPLINE_CURVE_WITH_KNOTS('',3,(#55466,#55467,#55468,#55469,#55470,
#55471,#55472,#55473,#55474,#55475,#55476,#55477,#55478,#55479,#55480,#55481,
#55482,#55483,#55484,#55485,#55486,#55487,#55488,#55489,#55490,#55491,#55492,
#55493,#55494,#55495,#55496,#55497,#55498,#55499,#55500,#55501,#55502,#55503,
#55504,#55505,#55506,#55507,#55508,#55509,#55510,#55511,#55512,#55513,#55514,
#55515,#55516,#55517,#55518,#55519,#55520,#55521,#55522,#55523,#55524,#55525,
#55526,#55527,#55528,#55529,#55530,#55531,#55532,#55533,#55534,#55535,#55536,
#55537,#55538,#55539,#55540,#55541,#55542,#55543,#55544,#55545,#55546,#55547,
#55548,#55549,#55550),.UNSPECIFIED.,.F.,.F.,(4,3,3,3,3,3,3,3,3,3,3,3,3,
3,3,3,3,3,3,3,3,3,3,3,3,3,3,3,4),(-0.463803050843723,-0.448467893697328,
-0.42674338256529,-0.414223896421318,-0.409751265194179,-0.387170206067839,
-0.368152570621498,-0.359003265127981,-0.354824456856625,-0.331562984878854,
-0.307429519283418,-0.28932942008684,-0.275754345689407,-0.271732471107105,
-0.267646412172009,-0.243218942153542,-0.235029122497107,-0.211434734441675,
-0.187352373722984,-0.181481960030832,-0.157053290808756,-0.132137976349438,
-0.107029329959023,-0.096367863765101,-0.0910169135905318,-0.0652788097838639,
-0.039498554230681,-0.0142610096161325,0.),.UNSPECIFIED.);
#11456=B_SPLINE_CURVE_WITH_KNOTS('',3,(#55554,#55555,#55556,#55557,#55558,
#55559),.UNSPECIFIED.,.F.,.F.,(4,2,4),(1.2907552072404,1.37375394746467,
1.45675268768893),.UNSPECIFIED.);
#11457=B_SPLINE_CURVE_WITH_KNOTS('',3,(#55567,#55568,#55569,#55570,#55571,
#55572),.UNSPECIFIED.,.F.,.F.,(4,2,4),(1.2907552072404,1.37375394746467,
1.45675268768893),.UNSPECIFIED.);
#11458=B_SPLINE_CURVE_WITH_KNOTS('',3,(#55578,#55579,#55580,#55581,#55582,
#55583),.UNSPECIFIED.,.F.,.F.,(4,2,4),(1.2907552072404,1.37375394746467,
1.45675268768893),.UNSPECIFIED.);
#11459=B_SPLINE_CURVE_WITH_KNOTS('',3,(#55589,#55590,#55591,#55592,#55593,
#55594),.UNSPECIFIED.,.F.,.F.,(4,2,4),(1.2907552072404,1.37375394746467,
1.45675268768893),.UNSPECIFIED.);
#11460=B_SPLINE_CURVE_WITH_KNOTS('',3,(#55600,#55601,#55602,#55603,#55604,
#55605),.UNSPECIFIED.,.F.,.F.,(4,2,4),(1.2907552072404,1.37375394746467,
1.45675268768893),.UNSPECIFIED.);
#11461=B_SPLINE_CURVE_WITH_KNOTS('',3,(#55610,#55611,#55612,#55613,#55614,
#55615),.UNSPECIFIED.,.F.,.F.,(4,2,4),(1.2907552072404,1.37375394746467,
1.45675268768893),.UNSPECIFIED.);
#11462=VERTEX_POINT('',#37378);
#11463=VERTEX_POINT('',#37379);
#11464=VERTEX_POINT('',#37386);
#11465=VERTEX_POINT('',#37388);
#11466=VERTEX_POINT('',#37391);
#11467=VERTEX_POINT('',#37393);
#11468=VERTEX_POINT('',#37414);
#11469=VERTEX_POINT('',#37416);
#11470=VERTEX_POINT('',#37418);
#11471=VERTEX_POINT('',#37420);
#11472=VERTEX_POINT('',#37431);
#11473=VERTEX_POINT('',#37433);
#11474=VERTEX_POINT('',#37444);
#11475=VERTEX_POINT('',#37446);
#11476=VERTEX_POINT('',#37457);
#11477=VERTEX_POINT('',#37459);
#11478=VERTEX_POINT('',#37470);
#11479=VERTEX_POINT('',#37472);
#11480=VERTEX_POINT('',#37483);
#11481=VERTEX_POINT('',#37492);
#11482=VERTEX_POINT('',#37494);
#11483=VERTEX_POINT('',#37496);
#11484=VERTEX_POINT('',#37498);
#11485=VERTEX_POINT('',#37500);
#11486=VERTEX_POINT('',#37503);
#11487=VERTEX_POINT('',#37509);
#11488=VERTEX_POINT('',#37511);
#11489=VERTEX_POINT('',#37513);
#11490=VERTEX_POINT('',#37515);
#11491=VERTEX_POINT('',#37517);
#11492=VERTEX_POINT('',#37519);
#11493=VERTEX_POINT('',#37521);
#11494=VERTEX_POINT('',#37523);
#11495=VERTEX_POINT('',#37525);
#11496=VERTEX_POINT('',#37528);
#11497=VERTEX_POINT('',#37529);
#11498=VERTEX_POINT('',#37531);
#11499=VERTEX_POINT('',#37533);
#11500=VERTEX_POINT('',#37545);
#11501=VERTEX_POINT('',#37546);
#11502=VERTEX_POINT('',#37551);
#11503=VERTEX_POINT('',#37552);
#11504=VERTEX_POINT('',#37565);
#11505=VERTEX_POINT('',#37566);
#11506=VERTEX_POINT('',#37571);
#11507=VERTEX_POINT('',#37572);
#11508=VERTEX_POINT('',#37585);
#11509=VERTEX_POINT('',#37586);
#11510=VERTEX_POINT('',#37591);
#11511=VERTEX_POINT('',#37592);
#11512=VERTEX_POINT('',#37608);
#11513=VERTEX_POINT('',#37610);
#11514=VERTEX_POINT('',#37614);
#11515=VERTEX_POINT('',#37618);
#11516=VERTEX_POINT('',#37622);
#11517=VERTEX_POINT('',#37626);
#11518=VERTEX_POINT('',#37628);
#11519=VERTEX_POINT('',#37631);
#11520=VERTEX_POINT('',#37632);
#11521=VERTEX_POINT('',#37634);
#11522=VERTEX_POINT('',#37636);
#11523=VERTEX_POINT('',#37648);
#11524=VERTEX_POINT('',#37649);
#11525=VERTEX_POINT('',#37654);
#11526=VERTEX_POINT('',#37667);
#11527=VERTEX_POINT('',#37671);
#11528=VERTEX_POINT('',#37683);
#11529=VERTEX_POINT('',#37687);
#11530=VERTEX_POINT('',#37708);
#11531=VERTEX_POINT('',#37709);
#11532=VERTEX_POINT('',#37711);
#11533=VERTEX_POINT('',#37713);
#11534=VERTEX_POINT('',#37715);
#11535=VERTEX_POINT('',#37717);
#11536=VERTEX_POINT('',#37719);
#11537=VERTEX_POINT('',#37721);
#11538=VERTEX_POINT('',#37724);
#11539=VERTEX_POINT('',#37726);
#11540=VERTEX_POINT('',#37729);
#11541=VERTEX_POINT('',#37730);
#11542=VERTEX_POINT('',#37732);
#11543=VERTEX_POINT('',#37734);
#11544=VERTEX_POINT('',#37746);
#11545=VERTEX_POINT('',#37747);
#11546=VERTEX_POINT('',#37752);
#11547=VERTEX_POINT('',#37753);
#11548=VERTEX_POINT('',#37766);
#11549=VERTEX_POINT('',#37767);
#11550=VERTEX_POINT('',#37772);
#11551=VERTEX_POINT('',#37773);
#11552=VERTEX_POINT('',#37786);
#11553=VERTEX_POINT('',#37787);
#11554=VERTEX_POINT('',#37792);
#11555=VERTEX_POINT('',#37793);
#11556=VERTEX_POINT('',#37809);
#11557=VERTEX_POINT('',#37811);
#11558=VERTEX_POINT('',#37815);
#11559=VERTEX_POINT('',#37819);
#11560=VERTEX_POINT('',#37823);
#11561=VERTEX_POINT('',#37827);
#11562=VERTEX_POINT('',#37830);
#11563=VERTEX_POINT('',#37831);
#11564=VERTEX_POINT('',#37833);
#11565=VERTEX_POINT('',#37835);
#11566=VERTEX_POINT('',#37847);
#11567=VERTEX_POINT('',#37848);
#11568=VERTEX_POINT('',#37853);
#11569=VERTEX_POINT('',#37854);
#11570=VERTEX_POINT('',#37867);
#11571=VERTEX_POINT('',#37868);
#11572=VERTEX_POINT('',#37873);
#11573=VERTEX_POINT('',#37874);
#11574=VERTEX_POINT('',#37887);
#11575=VERTEX_POINT('',#37888);
#11576=VERTEX_POINT('',#37893);
#11577=VERTEX_POINT('',#37894);
#11578=VERTEX_POINT('',#37910);
#11579=VERTEX_POINT('',#37912);
#11580=VERTEX_POINT('',#37916);
#11581=VERTEX_POINT('',#37920);
#11582=VERTEX_POINT('',#37924);
#11583=VERTEX_POINT('',#37928);
#11584=VERTEX_POINT('',#37931);
#11585=VERTEX_POINT('',#37935);
#11586=VERTEX_POINT('',#37937);
#11587=VERTEX_POINT('',#37939);
#11588=VERTEX_POINT('',#37941);
#11589=VERTEX_POINT('',#37952);
#11590=VERTEX_POINT('',#37954);
#11591=VERTEX_POINT('',#37965);
#11592=VERTEX_POINT('',#37969);
#11593=VERTEX_POINT('',#37971);
#11594=VERTEX_POINT('',#37975);
#11595=VERTEX_POINT('',#37977);
#11596=VERTEX_POINT('',#37981);
#11597=VERTEX_POINT('',#37985);
#11598=VERTEX_POINT('',#38002);
#11599=VERTEX_POINT('',#38021);
#11600=VERTEX_POINT('',#38025);
#11601=VERTEX_POINT('',#38031);
#11602=VERTEX_POINT('',#38032);
#11603=VERTEX_POINT('',#38034);
#11604=VERTEX_POINT('',#38036);
#11605=VERTEX_POINT('',#38038);
#11606=VERTEX_POINT('',#38089);
#11607=VERTEX_POINT('',#38090);
#11608=VERTEX_POINT('',#38109);
#11609=VERTEX_POINT('',#38110);
#11610=VERTEX_POINT('',#38179);
#11611=VERTEX_POINT('',#38181);
#11612=VERTEX_POINT('',#38183);
#11613=VERTEX_POINT('',#38185);
#11614=VERTEX_POINT('',#38189);
#11615=VERTEX_POINT('',#38193);
#11616=VERTEX_POINT('',#38197);
#11617=VERTEX_POINT('',#38199);
#11618=VERTEX_POINT('',#38203);
#11619=VERTEX_POINT('',#38204);
#11620=VERTEX_POINT('',#38206);
#11621=VERTEX_POINT('',#38208);
#11622=VERTEX_POINT('',#38212);
#11623=VERTEX_POINT('',#38213);
#11624=VERTEX_POINT('',#38224);
#11625=VERTEX_POINT('',#38226);
#11626=VERTEX_POINT('',#38228);
#11627=VERTEX_POINT('',#38230);
#11628=VERTEX_POINT('',#38246);
#11629=VERTEX_POINT('',#38247);
#11630=VERTEX_POINT('',#38250);
#11631=VERTEX_POINT('',#38254);
#11632=VERTEX_POINT('',#38258);
#11633=VERTEX_POINT('',#38262);
#11634=VERTEX_POINT('',#38266);
#11635=VERTEX_POINT('',#38270);
#11636=VERTEX_POINT('',#38271);
#11637=VERTEX_POINT('',#38276);
#11638=VERTEX_POINT('',#38277);
#11639=VERTEX_POINT('',#38285);
#11640=VERTEX_POINT('',#38289);
#11641=VERTEX_POINT('',#38291);
#11642=VERTEX_POINT('',#38293);
#11643=VERTEX_POINT('',#38296);
#11644=VERTEX_POINT('',#38298);
#11645=VERTEX_POINT('',#38300);
#11646=VERTEX_POINT('',#38303);
#11647=VERTEX_POINT('',#38306);
#11648=VERTEX_POINT('',#38308);
#11649=VERTEX_POINT('',#38310);
#11650=VERTEX_POINT('',#38367);
#11651=VERTEX_POINT('',#38379);
#11652=VERTEX_POINT('',#38380);
#11653=VERTEX_POINT('',#38452);
#11654=VERTEX_POINT('',#38460);
#11655=VERTEX_POINT('',#38465);
#11656=VERTEX_POINT('',#38470);
#11657=VERTEX_POINT('',#38478);
#11658=VERTEX_POINT('',#38482);
#11659=VERTEX_POINT('',#38487);
#11660=VERTEX_POINT('',#38492);
#11661=VERTEX_POINT('',#38497);
#11662=VERTEX_POINT('',#38502);
#11663=VERTEX_POINT('',#38507);
#11664=VERTEX_POINT('',#38512);
#11665=VERTEX_POINT('',#38517);
#11666=VERTEX_POINT('',#38522);
#11667=VERTEX_POINT('',#38527);
#11668=VERTEX_POINT('',#38532);
#11669=VERTEX_POINT('',#38537);
#11670=VERTEX_POINT('',#38543);
#11671=VERTEX_POINT('',#38579);
#11672=VERTEX_POINT('',#38610);
#11673=VERTEX_POINT('',#38611);
#11674=VERTEX_POINT('',#38667);
#11675=VERTEX_POINT('',#38672);
#11676=VERTEX_POINT('',#38753);
#11677=VERTEX_POINT('',#38760);
#11678=VERTEX_POINT('',#38769);
#11679=VERTEX_POINT('',#38770);
#11680=VERTEX_POINT('',#38775);
#11681=VERTEX_POINT('',#38777);
#11682=VERTEX_POINT('',#38779);
#11683=VERTEX_POINT('',#38781);
#11684=VERTEX_POINT('',#38783);
#11685=VERTEX_POINT('',#38787);
#11686=VERTEX_POINT('',#38789);
#11687=VERTEX_POINT('',#38853);
#11688=VERTEX_POINT('',#38880);
#11689=VERTEX_POINT('',#38968);
#11690=VERTEX_POINT('',#38978);
#11691=VERTEX_POINT('',#38982);
#11692=VERTEX_POINT('',#38995);
#11693=VERTEX_POINT('',#39022);
#11694=VERTEX_POINT('',#39023);
#11695=VERTEX_POINT('',#39079);
#11696=VERTEX_POINT('',#39084);
#11697=VERTEX_POINT('',#39165);
#11698=VERTEX_POINT('',#39172);
#11699=VERTEX_POINT('',#39181);
#11700=VERTEX_POINT('',#39182);
#11701=VERTEX_POINT('',#39187);
#11702=VERTEX_POINT('',#39189);
#11703=VERTEX_POINT('',#39191);
#11704=VERTEX_POINT('',#39195);
#11705=VERTEX_POINT('',#39199);
#11706=VERTEX_POINT('',#39226);
#11707=VERTEX_POINT('',#39227);
#11708=VERTEX_POINT('',#39283);
#11709=VERTEX_POINT('',#39288);
#11710=VERTEX_POINT('',#39369);
#11711=VERTEX_POINT('',#39376);
#11712=VERTEX_POINT('',#39385);
#11713=VERTEX_POINT('',#39386);
#11714=VERTEX_POINT('',#39391);
#11715=VERTEX_POINT('',#39393);
#11716=VERTEX_POINT('',#39395);
#11717=VERTEX_POINT('',#39397);
#11718=VERTEX_POINT('',#39401);
#11719=VERTEX_POINT('',#39403);
#11720=VERTEX_POINT('',#39466);
#11721=VERTEX_POINT('',#39493);
#11722=VERTEX_POINT('',#39577);
#11723=VERTEX_POINT('',#39586);
#11724=VERTEX_POINT('',#39590);
#11725=VERTEX_POINT('',#39603);
#11726=VERTEX_POINT('',#39630);
#11727=VERTEX_POINT('',#39631);
#11728=VERTEX_POINT('',#39687);
#11729=VERTEX_POINT('',#39692);
#11730=VERTEX_POINT('',#39777);
#11731=VERTEX_POINT('',#39785);
#11732=VERTEX_POINT('',#39795);
#11733=VERTEX_POINT('',#39796);
#11734=VERTEX_POINT('',#39801);
#11735=VERTEX_POINT('',#39803);
#11736=VERTEX_POINT('',#39805);
#11737=VERTEX_POINT('',#39807);
#11738=VERTEX_POINT('',#39811);
#11739=VERTEX_POINT('',#39813);
#11740=VERTEX_POINT('',#39877);
#11741=VERTEX_POINT('',#39904);
#11742=VERTEX_POINT('',#39992);
#11743=VERTEX_POINT('',#40002);
#11744=VERTEX_POINT('',#40006);
#11745=VERTEX_POINT('',#40019);
#11746=VERTEX_POINT('',#40023);
#11747=VERTEX_POINT('',#40025);
#11748=VERTEX_POINT('',#40029);
#11749=VERTEX_POINT('',#40033);
#11750=VERTEX_POINT('',#40037);
#11751=VERTEX_POINT('',#40041);
#11752=VERTEX_POINT('',#40043);
#11753=VERTEX_POINT('',#40045);
#11754=VERTEX_POINT('',#40047);
#11755=VERTEX_POINT('',#40049);
#11756=VERTEX_POINT('',#40051);
#11757=VERTEX_POINT('',#40053);
#11758=VERTEX_POINT('',#40055);
#11759=VERTEX_POINT('',#40057);
#11760=VERTEX_POINT('',#40059);
#11761=VERTEX_POINT('',#40061);
#11762=VERTEX_POINT('',#40064);
#11763=VERTEX_POINT('',#40067);
#11764=VERTEX_POINT('',#40070);
#11765=VERTEX_POINT('',#40074);
#11766=VERTEX_POINT('',#40089);
#11767=VERTEX_POINT('',#40104);
#11768=VERTEX_POINT('',#40108);
#11769=VERTEX_POINT('',#40109);
#11770=VERTEX_POINT('',#40111);
#11771=VERTEX_POINT('',#40113);
#11772=VERTEX_POINT('',#40115);
#11773=VERTEX_POINT('',#40117);
#11774=VERTEX_POINT('',#40119);
#11775=VERTEX_POINT('',#40121);
#11776=VERTEX_POINT('',#40123);
#11777=VERTEX_POINT('',#40125);
#11778=VERTEX_POINT('',#40127);
#11779=VERTEX_POINT('',#40129);
#11780=VERTEX_POINT('',#40131);
#11781=VERTEX_POINT('',#40133);
#11782=VERTEX_POINT('',#40135);
#11783=VERTEX_POINT('',#40137);
#11784=VERTEX_POINT('',#40139);
#11785=VERTEX_POINT('',#40141);
#11786=VERTEX_POINT('',#40143);
#11787=VERTEX_POINT('',#40145);
#11788=VERTEX_POINT('',#40147);
#11789=VERTEX_POINT('',#40149);
#11790=VERTEX_POINT('',#40151);
#11791=VERTEX_POINT('',#40153);
#11792=VERTEX_POINT('',#40155);
#11793=VERTEX_POINT('',#40159);
#11794=VERTEX_POINT('',#40161);
#11795=VERTEX_POINT('',#40165);
#11796=VERTEX_POINT('',#40169);
#11797=VERTEX_POINT('',#40170);
#11798=VERTEX_POINT('',#40174);
#11799=VERTEX_POINT('',#40178);
#11800=VERTEX_POINT('',#40182);
#11801=VERTEX_POINT('',#40184);
#11802=VERTEX_POINT('',#40188);
#11803=VERTEX_POINT('',#40192);
#11804=VERTEX_POINT('',#40196);
#11805=VERTEX_POINT('',#40200);
#11806=VERTEX_POINT('',#40204);
#11807=VERTEX_POINT('',#40208);
#11808=VERTEX_POINT('',#40212);
#11809=VERTEX_POINT('',#40216);
#11810=VERTEX_POINT('',#40220);
#11811=VERTEX_POINT('',#40224);
#11812=VERTEX_POINT('',#40228);
#11813=VERTEX_POINT('',#40232);
#11814=VERTEX_POINT('',#40236);
#11815=VERTEX_POINT('',#40240);
#11816=VERTEX_POINT('',#40244);
#11817=VERTEX_POINT('',#40248);
#11818=VERTEX_POINT('',#40252);
#11819=VERTEX_POINT('',#40256);
#11820=VERTEX_POINT('',#40258);
#11821=VERTEX_POINT('',#40262);
#11822=VERTEX_POINT('',#40266);
#11823=VERTEX_POINT('',#40270);
#11824=VERTEX_POINT('',#40274);
#11825=VERTEX_POINT('',#40278);
#11826=VERTEX_POINT('',#40282);
#11827=VERTEX_POINT('',#40286);
#11828=VERTEX_POINT('',#40290);
#11829=VERTEX_POINT('',#40294);
#11830=VERTEX_POINT('',#40298);
#11831=VERTEX_POINT('',#40305);
#11832=VERTEX_POINT('',#40306);
#11833=VERTEX_POINT('',#40308);
#11834=VERTEX_POINT('',#40310);
#11835=VERTEX_POINT('',#40312);
#11836=VERTEX_POINT('',#40314);
#11837=VERTEX_POINT('',#40316);
#11838=VERTEX_POINT('',#40318);
#11839=VERTEX_POINT('',#40320);
#11840=VERTEX_POINT('',#40324);
#11841=VERTEX_POINT('',#40328);
#11842=VERTEX_POINT('',#40331);
#11843=VERTEX_POINT('',#40332);
#11844=VERTEX_POINT('',#40334);
#11845=VERTEX_POINT('',#40336);
#11846=VERTEX_POINT('',#40338);
#11847=VERTEX_POINT('',#40340);
#11848=VERTEX_POINT('',#40342);
#11849=VERTEX_POINT('',#40344);
#11850=VERTEX_POINT('',#40346);
#11851=VERTEX_POINT('',#40348);
#11852=VERTEX_POINT('',#40350);
#11853=VERTEX_POINT('',#40352);
#11854=VERTEX_POINT('',#40355);
#11855=VERTEX_POINT('',#40356);
#11856=VERTEX_POINT('',#40358);
#11857=VERTEX_POINT('',#40362);
#11858=VERTEX_POINT('',#40366);
#11859=VERTEX_POINT('',#40370);
#11860=VERTEX_POINT('',#40374);
#11861=VERTEX_POINT('',#40378);
#11862=VERTEX_POINT('',#40382);
#11863=VERTEX_POINT('',#40386);
#11864=VERTEX_POINT('',#40390);
#11865=VERTEX_POINT('',#40394);
#11866=VERTEX_POINT('',#40398);
#11867=VERTEX_POINT('',#40402);
#11868=VERTEX_POINT('',#40405);
#11869=VERTEX_POINT('',#40406);
#11870=VERTEX_POINT('',#40408);
#11871=VERTEX_POINT('',#40412);
#11872=VERTEX_POINT('',#40416);
#11873=VERTEX_POINT('',#40420);
#11874=VERTEX_POINT('',#40424);
#11875=VERTEX_POINT('',#40428);
#11876=VERTEX_POINT('',#40432);
#11877=VERTEX_POINT('',#40436);
#11878=VERTEX_POINT('',#40438);
#11879=VERTEX_POINT('',#40440);
#11880=VERTEX_POINT('',#40442);
#11881=VERTEX_POINT('',#40444);
#11882=VERTEX_POINT('',#40446);
#11883=VERTEX_POINT('',#40448);
#11884=VERTEX_POINT('',#40450);
#11885=VERTEX_POINT('',#40452);
#11886=VERTEX_POINT('',#40454);
#11887=VERTEX_POINT('',#40456);
#11888=VERTEX_POINT('',#40460);
#11889=VERTEX_POINT('',#40464);
#11890=VERTEX_POINT('',#40468);
#11891=VERTEX_POINT('',#40472);
#11892=VERTEX_POINT('',#40474);
#11893=VERTEX_POINT('',#40476);
#11894=VERTEX_POINT('',#40480);
#11895=VERTEX_POINT('',#40493);
#11896=VERTEX_POINT('',#40499);
#11897=VERTEX_POINT('',#40514);
#11898=VERTEX_POINT('',#40518);
#11899=VERTEX_POINT('',#40536);
#11900=VERTEX_POINT('',#40537);
#11901=VERTEX_POINT('',#40539);
#11902=VERTEX_POINT('',#40554);
#11903=VERTEX_POINT('',#40571);
#11904=VERTEX_POINT('',#40573);
#11905=VERTEX_POINT('',#40586);
#11906=VERTEX_POINT('',#40588);
#11907=VERTEX_POINT('',#40603);
#11908=VERTEX_POINT('',#40604);
#11909=VERTEX_POINT('',#40607);
#11910=VERTEX_POINT('',#40611);
#11911=VERTEX_POINT('',#40613);
#11912=VERTEX_POINT('',#40616);
#11913=VERTEX_POINT('',#40640);
#11914=VERTEX_POINT('',#40642);
#11915=VERTEX_POINT('',#40666);
#11916=VERTEX_POINT('',#40670);
#11917=VERTEX_POINT('',#40672);
#11918=VERTEX_POINT('',#40676);
#11919=VERTEX_POINT('',#40678);
#11920=VERTEX_POINT('',#40682);
#11921=VERTEX_POINT('',#40684);
#11922=VERTEX_POINT('',#40688);
#11923=VERTEX_POINT('',#40690);
#11924=VERTEX_POINT('',#40692);
#11925=VERTEX_POINT('',#40696);
#11926=VERTEX_POINT('',#40698);
#11927=VERTEX_POINT('',#40702);
#11928=VERTEX_POINT('',#40704);
#11929=VERTEX_POINT('',#40708);
#11930=VERTEX_POINT('',#40716);
#11931=VERTEX_POINT('',#40719);
#11932=VERTEX_POINT('',#40721);
#11933=VERTEX_POINT('',#40728);
#11934=VERTEX_POINT('',#40730);
#11935=VERTEX_POINT('',#40734);
#11936=VERTEX_POINT('',#40738);
#11937=VERTEX_POINT('',#40742);
#11938=VERTEX_POINT('',#40746);
#11939=VERTEX_POINT('',#40750);
#11940=VERTEX_POINT('',#40754);
#11941=VERTEX_POINT('',#40758);
#11942=VERTEX_POINT('',#40764);
#11943=VERTEX_POINT('',#40776);
#11944=VERTEX_POINT('',#40778);
#11945=VERTEX_POINT('',#40789);
#11946=VERTEX_POINT('',#40800);
#11947=VERTEX_POINT('',#40811);
#11948=VERTEX_POINT('',#40822);
#11949=VERTEX_POINT('',#40833);
#11950=VERTEX_POINT('',#40844);
#11951=VERTEX_POINT('',#40855);
#11952=VERTEX_POINT('',#40866);
#11953=VERTEX_POINT('',#40877);
#11954=VERTEX_POINT('',#40885);
#11955=VERTEX_POINT('',#40904);
#11956=VERTEX_POINT('',#40906);
#11957=VERTEX_POINT('',#40917);
#11958=VERTEX_POINT('',#40928);
#11959=VERTEX_POINT('',#40939);
#11960=VERTEX_POINT('',#40950);
#11961=VERTEX_POINT('',#40961);
#11962=VERTEX_POINT('',#40972);
#11963=VERTEX_POINT('',#40983);
#11964=VERTEX_POINT('',#40994);
#11965=VERTEX_POINT('',#41005);
#11966=VERTEX_POINT('',#41016);
#11967=VERTEX_POINT('',#41027);
#11968=VERTEX_POINT('',#41038);
#11969=VERTEX_POINT('',#41044);
#11970=VERTEX_POINT('',#41053);
#11971=VERTEX_POINT('',#41064);
#11972=VERTEX_POINT('',#41075);
#11973=VERTEX_POINT('',#41086);
#11974=VERTEX_POINT('',#41097);
#11975=VERTEX_POINT('',#41108);
#11976=VERTEX_POINT('',#41119);
#11977=VERTEX_POINT('',#41130);
#11978=VERTEX_POINT('',#41141);
#11979=VERTEX_POINT('',#41152);
#11980=VERTEX_POINT('',#41163);
#11981=VERTEX_POINT('',#41174);
#11982=VERTEX_POINT('',#41185);
#11983=VERTEX_POINT('',#41196);
#11984=VERTEX_POINT('',#41207);
#11985=VERTEX_POINT('',#41218);
#11986=VERTEX_POINT('',#41229);
#11987=VERTEX_POINT('',#41240);
#11988=VERTEX_POINT('',#41246);
#11989=VERTEX_POINT('',#41255);
#11990=VERTEX_POINT('',#41271);
#11991=VERTEX_POINT('',#41273);
#11992=VERTEX_POINT('',#41282);
#11993=VERTEX_POINT('',#41293);
#11994=VERTEX_POINT('',#41304);
#11995=VERTEX_POINT('',#41315);
#11996=VERTEX_POINT('',#41323);
#11997=VERTEX_POINT('',#41332);
#11998=VERTEX_POINT('',#41343);
#11999=VERTEX_POINT('',#41354);
#12000=VERTEX_POINT('',#41365);
#12001=VERTEX_POINT('',#41376);
#12002=VERTEX_POINT('',#41387);
#12003=VERTEX_POINT('',#41398);
#12004=VERTEX_POINT('',#41406);
#12005=VERTEX_POINT('',#41413);
#12006=VERTEX_POINT('',#41415);
#12007=VERTEX_POINT('',#41419);
#12008=VERTEX_POINT('',#41423);
#12009=VERTEX_POINT('',#41432);
#12010=VERTEX_POINT('',#41443);
#12011=VERTEX_POINT('',#41449);
#12012=VERTEX_POINT('',#41453);
#12013=VERTEX_POINT('',#41457);
#12014=VERTEX_POINT('',#41461);
#12015=VERTEX_POINT('',#41465);
#12016=VERTEX_POINT('',#41481);
#12017=VERTEX_POINT('',#41483);
#12018=VERTEX_POINT('',#41494);
#12019=VERTEX_POINT('',#41496);
#12020=VERTEX_POINT('',#41500);
#12021=VERTEX_POINT('',#41504);
#12022=VERTEX_POINT('',#41505);
#12023=VERTEX_POINT('',#41507);
#12024=VERTEX_POINT('',#41509);
#12025=VERTEX_POINT('',#41511);
#12026=VERTEX_POINT('',#41513);
#12027=VERTEX_POINT('',#41515);
#12028=VERTEX_POINT('',#41517);
#12029=VERTEX_POINT('',#41521);
#12030=VERTEX_POINT('',#41525);
#12031=VERTEX_POINT('',#41528);
#12032=VERTEX_POINT('',#41530);
#12033=VERTEX_POINT('',#41534);
#12034=VERTEX_POINT('',#41535);
#12035=VERTEX_POINT('',#41537);
#12036=VERTEX_POINT('',#41539);
#12037=VERTEX_POINT('',#41541);
#12038=VERTEX_POINT('',#41543);
#12039=VERTEX_POINT('',#41545);
#12040=VERTEX_POINT('',#41547);
#12041=VERTEX_POINT('',#41549);
#12042=VERTEX_POINT('',#41551);
#12043=VERTEX_POINT('',#41554);
#12044=VERTEX_POINT('',#41556);
#12045=VERTEX_POINT('',#41557);
#12046=VERTEX_POINT('',#41559);
#12047=VERTEX_POINT('',#41561);
#12048=VERTEX_POINT('',#41563);
#12049=VERTEX_POINT('',#41565);
#12050=VERTEX_POINT('',#41567);
#12051=VERTEX_POINT('',#41569);
#12052=VERTEX_POINT('',#41573);
#12053=VERTEX_POINT('',#41577);
#12054=VERTEX_POINT('',#41581);
#12055=VERTEX_POINT('',#41585);
#12056=VERTEX_POINT('',#41586);
#12057=VERTEX_POINT('',#41588);
#12058=VERTEX_POINT('',#41590);
#12059=VERTEX_POINT('',#41613);
#12060=VERTEX_POINT('',#41623);
#12061=VERTEX_POINT('',#41625);
#12062=VERTEX_POINT('',#41628);
#12063=VERTEX_POINT('',#41630);
#12064=VERTEX_POINT('',#41632);
#12065=VERTEX_POINT('',#41634);
#12066=VERTEX_POINT('',#41636);
#12067=VERTEX_POINT('',#41638);
#12068=VERTEX_POINT('',#41640);
#12069=VERTEX_POINT('',#41643);
#12070=VERTEX_POINT('',#41644);
#12071=VERTEX_POINT('',#41646);
#12072=VERTEX_POINT('',#41648);
#12073=VERTEX_POINT('',#41650);
#12074=VERTEX_POINT('',#41652);
#12075=VERTEX_POINT('',#41654);
#12076=VERTEX_POINT('',#41656);
#12077=VERTEX_POINT('',#41660);
#12078=VERTEX_POINT('',#41664);
#12079=VERTEX_POINT('',#41666);
#12080=VERTEX_POINT('',#41668);
#12081=VERTEX_POINT('',#41696);
#12082=VERTEX_POINT('',#41704);
#12083=VERTEX_POINT('',#41708);
#12084=VERTEX_POINT('',#41710);
#12085=VERTEX_POINT('',#41733);
#12086=VERTEX_POINT('',#41743);
#12087=VERTEX_POINT('',#41747);
#12088=VERTEX_POINT('',#41749);
#12089=VERTEX_POINT('',#41751);
#12090=VERTEX_POINT('',#41775);
#12091=VERTEX_POINT('',#41779);
#12092=VERTEX_POINT('',#41783);
#12093=VERTEX_POINT('',#41784);
#12094=VERTEX_POINT('',#41786);
#12095=VERTEX_POINT('',#41788);
#12096=VERTEX_POINT('',#41792);
#12097=VERTEX_POINT('',#41797);
#12098=VERTEX_POINT('',#41799);
#12099=VERTEX_POINT('',#41804);
#12100=VERTEX_POINT('',#41809);
#12101=VERTEX_POINT('',#41811);
#12102=VERTEX_POINT('',#41813);
#12103=VERTEX_POINT('',#41814);
#12104=VERTEX_POINT('',#41816);
#12105=VERTEX_POINT('',#41818);
#12106=VERTEX_POINT('',#41820);
#12107=VERTEX_POINT('',#41822);
#12108=VERTEX_POINT('',#41824);
#12109=VERTEX_POINT('',#41826);
#12110=VERTEX_POINT('',#41829);
#12111=VERTEX_POINT('',#41838);
#12112=VERTEX_POINT('',#41840);
#12113=VERTEX_POINT('',#41844);
#12114=VERTEX_POINT('',#41846);
#12115=VERTEX_POINT('',#41848);
#12116=VERTEX_POINT('',#41850);
#12117=VERTEX_POINT('',#41852);
#12118=VERTEX_POINT('',#41855);
#12119=VERTEX_POINT('',#41859);
#12120=VERTEX_POINT('',#41863);
#12121=VERTEX_POINT('',#41867);
#12122=VERTEX_POINT('',#41871);
#12123=VERTEX_POINT('',#41875);
#12124=VERTEX_POINT('',#41879);
#12125=VERTEX_POINT('',#41883);
#12126=VERTEX_POINT('',#41887);
#12127=VERTEX_POINT('',#41888);
#12128=VERTEX_POINT('',#41890);
#12129=VERTEX_POINT('',#41892);
#12130=VERTEX_POINT('',#41894);
#12131=VERTEX_POINT('',#41896);
#12132=VERTEX_POINT('',#41898);
#12133=VERTEX_POINT('',#41900);
#12134=VERTEX_POINT('',#41903);
#12135=VERTEX_POINT('',#41908);
#12136=VERTEX_POINT('',#41910);
#12137=VERTEX_POINT('',#41914);
#12138=VERTEX_POINT('',#41918);
#12139=VERTEX_POINT('',#41920);
#12140=VERTEX_POINT('',#41922);
#12141=VERTEX_POINT('',#41924);
#12142=VERTEX_POINT('',#41926);
#12143=VERTEX_POINT('',#41929);
#12144=VERTEX_POINT('',#41933);
#12145=VERTEX_POINT('',#41935);
#12146=VERTEX_POINT('',#41937);
#12147=VERTEX_POINT('',#41939);
#12148=VERTEX_POINT('',#41941);
#12149=VERTEX_POINT('',#41944);
#12150=VERTEX_POINT('',#41946);
#12151=VERTEX_POINT('',#41950);
#12152=VERTEX_POINT('',#41957);
#12153=VERTEX_POINT('',#41961);
#12154=VERTEX_POINT('',#41963);
#12155=VERTEX_POINT('',#41965);
#12156=VERTEX_POINT('',#41984);
#12157=VERTEX_POINT('',#41999);
#12158=VERTEX_POINT('',#42010);
#12159=VERTEX_POINT('',#42014);
#12160=VERTEX_POINT('',#42016);
#12161=VERTEX_POINT('',#42020);
#12162=VERTEX_POINT('',#42031);
#12163=VERTEX_POINT('',#42035);
#12164=VERTEX_POINT('',#42037);
#12165=VERTEX_POINT('',#42041);
#12166=VERTEX_POINT('',#42052);
#12167=VERTEX_POINT('',#42056);
#12168=VERTEX_POINT('',#42077);
#12169=VERTEX_POINT('',#42082);
#12170=VERTEX_POINT('',#42091);
#12171=VERTEX_POINT('',#42096);
#12172=VERTEX_POINT('',#42108);
#12173=VERTEX_POINT('',#42110);
#12174=VERTEX_POINT('',#42122);
#12175=VERTEX_POINT('',#42126);
#12176=VERTEX_POINT('',#42138);
#12177=VERTEX_POINT('',#42142);
#12178=VERTEX_POINT('',#42154);
#12179=VERTEX_POINT('',#42158);
#12180=VERTEX_POINT('',#42181);
#12181=VERTEX_POINT('',#42188);
#12182=VERTEX_POINT('',#42190);
#12183=VERTEX_POINT('',#42193);
#12184=VERTEX_POINT('',#42195);
#12185=VERTEX_POINT('',#42199);
#12186=VERTEX_POINT('',#42201);
#12187=VERTEX_POINT('',#42205);
#12188=VERTEX_POINT('',#42207);
#12189=VERTEX_POINT('',#42213);
#12190=VERTEX_POINT('',#42217);
#12191=VERTEX_POINT('',#42221);
#12192=VERTEX_POINT('',#42223);
#12193=VERTEX_POINT('',#42227);
#12194=VERTEX_POINT('',#42231);
#12195=VERTEX_POINT('',#42236);
#12196=VERTEX_POINT('',#42237);
#12197=VERTEX_POINT('',#42239);
#12198=VERTEX_POINT('',#42241);
#12199=VERTEX_POINT('',#42245);
#12200=VERTEX_POINT('',#42246);
#12201=VERTEX_POINT('',#42251);
#12202=VERTEX_POINT('',#42252);
#12203=VERTEX_POINT('',#42257);
#12204=VERTEX_POINT('',#42258);
#12205=VERTEX_POINT('',#42263);
#12206=VERTEX_POINT('',#42264);
#12207=VERTEX_POINT('',#42269);
#12208=VERTEX_POINT('',#42270);
#12209=VERTEX_POINT('',#42275);
#12210=VERTEX_POINT('',#42276);
#12211=VERTEX_POINT('',#42284);
#12212=VERTEX_POINT('',#42286);
#12213=VERTEX_POINT('',#42290);
#12214=VERTEX_POINT('',#42294);
#12215=VERTEX_POINT('',#42298);
#12216=VERTEX_POINT('',#42302);
#12217=VERTEX_POINT('',#42303);
#12218=VERTEX_POINT('',#42308);
#12219=VERTEX_POINT('',#42310);
#12220=VERTEX_POINT('',#42314);
#12221=VERTEX_POINT('',#42315);
#12222=VERTEX_POINT('',#42320);
#12223=VERTEX_POINT('',#42321);
#12224=VERTEX_POINT('',#42326);
#12225=VERTEX_POINT('',#42327);
#12226=VERTEX_POINT('',#42332);
#12227=VERTEX_POINT('',#42337);
#12228=VERTEX_POINT('',#42341);
#12229=VERTEX_POINT('',#42356);
#12230=VERTEX_POINT('',#42358);
#12231=VERTEX_POINT('',#42362);
#12232=VERTEX_POINT('',#42363);
#12233=VERTEX_POINT('',#42368);
#12234=VERTEX_POINT('',#42369);
#12235=VERTEX_POINT('',#42374);
#12236=VERTEX_POINT('',#42379);
#12237=VERTEX_POINT('',#42383);
#12238=VERTEX_POINT('',#42384);
#12239=VERTEX_POINT('',#42389);
#12240=VERTEX_POINT('',#42390);
#12241=VERTEX_POINT('',#42401);
#12242=VERTEX_POINT('',#42403);
#12243=VERTEX_POINT('',#42405);
#12244=VERTEX_POINT('',#42407);
#12245=VERTEX_POINT('',#42409);
#12246=VERTEX_POINT('',#42411);
#12247=VERTEX_POINT('',#42416);
#12248=VERTEX_POINT('',#42419);
#12249=VERTEX_POINT('',#42421);
#12250=VERTEX_POINT('',#42425);
#12251=VERTEX_POINT('',#42429);
#12252=VERTEX_POINT('',#42433);
#12253=VERTEX_POINT('',#42437);
#12254=VERTEX_POINT('',#42441);
#12255=VERTEX_POINT('',#42445);
#12256=VERTEX_POINT('',#42451);
#12257=VERTEX_POINT('',#42453);
#12258=VERTEX_POINT('',#42457);
#12259=VERTEX_POINT('',#42461);
#12260=VERTEX_POINT('',#42465);
#12261=VERTEX_POINT('',#42472);
#12262=VERTEX_POINT('',#42476);
#12263=VERTEX_POINT('',#42480);
#12264=VERTEX_POINT('',#42512);
#12265=VERTEX_POINT('',#42514);
#12266=VERTEX_POINT('',#42519);
#12267=VERTEX_POINT('',#42521);
#12268=VERTEX_POINT('',#42567);
#12269=VERTEX_POINT('',#42568);
#12270=VERTEX_POINT('',#42570);
#12271=VERTEX_POINT('',#42572);
#12272=VERTEX_POINT('',#42576);
#12273=VERTEX_POINT('',#42578);
#12274=VERTEX_POINT('',#42582);
#12275=VERTEX_POINT('',#42584);
#12276=VERTEX_POINT('',#42586);
#12277=VERTEX_POINT('',#42588);
#12278=VERTEX_POINT('',#42590);
#12279=VERTEX_POINT('',#42592);
#12280=VERTEX_POINT('',#42594);
#12281=VERTEX_POINT('',#42596);
#12282=VERTEX_POINT('',#42598);
#12283=VERTEX_POINT('',#42600);
#12284=VERTEX_POINT('',#42602);
#12285=VERTEX_POINT('',#42604);
#12286=VERTEX_POINT('',#42606);
#12287=VERTEX_POINT('',#42608);
#12288=VERTEX_POINT('',#42610);
#12289=VERTEX_POINT('',#42612);
#12290=VERTEX_POINT('',#42614);
#12291=VERTEX_POINT('',#42616);
#12292=VERTEX_POINT('',#42618);
#12293=VERTEX_POINT('',#42620);
#12294=VERTEX_POINT('',#42622);
#12295=VERTEX_POINT('',#42624);
#12296=VERTEX_POINT('',#42626);
#12297=VERTEX_POINT('',#42628);
#12298=VERTEX_POINT('',#42630);
#12299=VERTEX_POINT('',#42632);
#12300=VERTEX_POINT('',#42634);
#12301=VERTEX_POINT('',#42636);
#12302=VERTEX_POINT('',#42638);
#12303=VERTEX_POINT('',#42640);
#12304=VERTEX_POINT('',#42642);
#12305=VERTEX_POINT('',#42644);
#12306=VERTEX_POINT('',#42646);
#12307=VERTEX_POINT('',#42648);
#12308=VERTEX_POINT('',#42650);
#12309=VERTEX_POINT('',#42652);
#12310=VERTEX_POINT('',#42654);
#12311=VERTEX_POINT('',#42656);
#12312=VERTEX_POINT('',#42658);
#12313=VERTEX_POINT('',#42660);
#12314=VERTEX_POINT('',#42662);
#12315=VERTEX_POINT('',#42664);
#12316=VERTEX_POINT('',#42666);
#12317=VERTEX_POINT('',#42668);
#12318=VERTEX_POINT('',#42670);
#12319=VERTEX_POINT('',#42672);
#12320=VERTEX_POINT('',#42674);
#12321=VERTEX_POINT('',#42676);
#12322=VERTEX_POINT('',#42678);
#12323=VERTEX_POINT('',#42680);
#12324=VERTEX_POINT('',#42682);
#12325=VERTEX_POINT('',#42684);
#12326=VERTEX_POINT('',#42686);
#12327=VERTEX_POINT('',#42688);
#12328=VERTEX_POINT('',#42690);
#12329=VERTEX_POINT('',#42692);
#12330=VERTEX_POINT('',#42694);
#12331=VERTEX_POINT('',#42696);
#12332=VERTEX_POINT('',#42698);
#12333=VERTEX_POINT('',#42700);
#12334=VERTEX_POINT('',#42702);
#12335=VERTEX_POINT('',#42704);
#12336=VERTEX_POINT('',#42706);
#12337=VERTEX_POINT('',#42708);
#12338=VERTEX_POINT('',#42710);
#12339=VERTEX_POINT('',#42712);
#12340=VERTEX_POINT('',#42714);
#12341=VERTEX_POINT('',#42716);
#12342=VERTEX_POINT('',#42718);
#12343=VERTEX_POINT('',#42720);
#12344=VERTEX_POINT('',#42722);
#12345=VERTEX_POINT('',#42724);
#12346=VERTEX_POINT('',#42726);
#12347=VERTEX_POINT('',#42728);
#12348=VERTEX_POINT('',#42730);
#12349=VERTEX_POINT('',#42732);
#12350=VERTEX_POINT('',#42734);
#12351=VERTEX_POINT('',#42736);
#12352=VERTEX_POINT('',#42738);
#12353=VERTEX_POINT('',#42740);
#12354=VERTEX_POINT('',#42742);
#12355=VERTEX_POINT('',#42744);
#12356=VERTEX_POINT('',#42746);
#12357=VERTEX_POINT('',#42748);
#12358=VERTEX_POINT('',#42750);
#12359=VERTEX_POINT('',#42752);
#12360=VERTEX_POINT('',#42754);
#12361=VERTEX_POINT('',#42756);
#12362=VERTEX_POINT('',#42758);
#12363=VERTEX_POINT('',#42760);
#12364=VERTEX_POINT('',#42762);
#12365=VERTEX_POINT('',#42764);
#12366=VERTEX_POINT('',#42766);
#12367=VERTEX_POINT('',#42768);
#12368=VERTEX_POINT('',#42770);
#12369=VERTEX_POINT('',#42772);
#12370=VERTEX_POINT('',#42774);
#12371=VERTEX_POINT('',#42776);
#12372=VERTEX_POINT('',#42778);
#12373=VERTEX_POINT('',#42780);
#12374=VERTEX_POINT('',#42782);
#12375=VERTEX_POINT('',#42784);
#12376=VERTEX_POINT('',#42786);
#12377=VERTEX_POINT('',#42788);
#12378=VERTEX_POINT('',#42790);
#12379=VERTEX_POINT('',#42792);
#12380=VERTEX_POINT('',#42794);
#12381=VERTEX_POINT('',#42796);
#12382=VERTEX_POINT('',#42798);
#12383=VERTEX_POINT('',#42800);
#12384=VERTEX_POINT('',#42802);
#12385=VERTEX_POINT('',#42804);
#12386=VERTEX_POINT('',#42806);
#12387=VERTEX_POINT('',#42808);
#12388=VERTEX_POINT('',#42810);
#12389=VERTEX_POINT('',#42812);
#12390=VERTEX_POINT('',#42814);
#12391=VERTEX_POINT('',#42816);
#12392=VERTEX_POINT('',#42818);
#12393=VERTEX_POINT('',#42820);
#12394=VERTEX_POINT('',#42822);
#12395=VERTEX_POINT('',#42824);
#12396=VERTEX_POINT('',#42826);
#12397=VERTEX_POINT('',#42828);
#12398=VERTEX_POINT('',#42830);
#12399=VERTEX_POINT('',#42832);
#12400=VERTEX_POINT('',#42834);
#12401=VERTEX_POINT('',#42836);
#12402=VERTEX_POINT('',#42838);
#12403=VERTEX_POINT('',#42840);
#12404=VERTEX_POINT('',#42842);
#12405=VERTEX_POINT('',#42844);
#12406=VERTEX_POINT('',#42846);
#12407=VERTEX_POINT('',#42848);
#12408=VERTEX_POINT('',#42850);
#12409=VERTEX_POINT('',#42852);
#12410=VERTEX_POINT('',#42854);
#12411=VERTEX_POINT('',#42856);
#12412=VERTEX_POINT('',#42858);
#12413=VERTEX_POINT('',#42860);
#12414=VERTEX_POINT('',#42862);
#12415=VERTEX_POINT('',#42864);
#12416=VERTEX_POINT('',#42866);
#12417=VERTEX_POINT('',#42868);
#12418=VERTEX_POINT('',#42870);
#12419=VERTEX_POINT('',#42872);
#12420=VERTEX_POINT('',#42874);
#12421=VERTEX_POINT('',#42876);
#12422=VERTEX_POINT('',#42878);
#12423=VERTEX_POINT('',#42880);
#12424=VERTEX_POINT('',#42882);
#12425=VERTEX_POINT('',#42884);
#12426=VERTEX_POINT('',#42886);
#12427=VERTEX_POINT('',#42888);
#12428=VERTEX_POINT('',#42890);
#12429=VERTEX_POINT('',#42892);
#12430=VERTEX_POINT('',#42894);
#12431=VERTEX_POINT('',#42896);
#12432=VERTEX_POINT('',#42898);
#12433=VERTEX_POINT('',#42900);
#12434=VERTEX_POINT('',#42902);
#12435=VERTEX_POINT('',#42904);
#12436=VERTEX_POINT('',#42906);
#12437=VERTEX_POINT('',#42908);
#12438=VERTEX_POINT('',#42910);
#12439=VERTEX_POINT('',#42912);
#12440=VERTEX_POINT('',#42914);
#12441=VERTEX_POINT('',#42916);
#12442=VERTEX_POINT('',#42918);
#12443=VERTEX_POINT('',#42920);
#12444=VERTEX_POINT('',#42922);
#12445=VERTEX_POINT('',#42924);
#12446=VERTEX_POINT('',#42926);
#12447=VERTEX_POINT('',#42928);
#12448=VERTEX_POINT('',#42930);
#12449=VERTEX_POINT('',#42932);
#12450=VERTEX_POINT('',#42934);
#12451=VERTEX_POINT('',#42936);
#12452=VERTEX_POINT('',#42938);
#12453=VERTEX_POINT('',#42940);
#12454=VERTEX_POINT('',#42942);
#12455=VERTEX_POINT('',#42944);
#12456=VERTEX_POINT('',#42946);
#12457=VERTEX_POINT('',#42948);
#12458=VERTEX_POINT('',#42950);
#12459=VERTEX_POINT('',#42952);
#12460=VERTEX_POINT('',#42954);
#12461=VERTEX_POINT('',#42956);
#12462=VERTEX_POINT('',#42958);
#12463=VERTEX_POINT('',#42960);
#12464=VERTEX_POINT('',#42962);
#12465=VERTEX_POINT('',#42964);
#12466=VERTEX_POINT('',#42966);
#12467=VERTEX_POINT('',#42968);
#12468=VERTEX_POINT('',#42971);
#12469=VERTEX_POINT('',#42973);
#12470=VERTEX_POINT('',#42975);
#12471=VERTEX_POINT('',#42977);
#12472=VERTEX_POINT('',#42979);
#12473=VERTEX_POINT('',#42981);
#12474=VERTEX_POINT('',#42983);
#12475=VERTEX_POINT('',#42985);
#12476=VERTEX_POINT('',#42987);
#12477=VERTEX_POINT('',#42989);
#12478=VERTEX_POINT('',#42991);
#12479=VERTEX_POINT('',#42993);
#12480=VERTEX_POINT('',#42995);
#12481=VERTEX_POINT('',#42997);
#12482=VERTEX_POINT('',#42999);
#12483=VERTEX_POINT('',#43001);
#12484=VERTEX_POINT('',#43003);
#12485=VERTEX_POINT('',#43005);
#12486=VERTEX_POINT('',#43007);
#12487=VERTEX_POINT('',#43009);
#12488=VERTEX_POINT('',#43011);
#12489=VERTEX_POINT('',#43013);
#12490=VERTEX_POINT('',#43015);
#12491=VERTEX_POINT('',#43017);
#12492=VERTEX_POINT('',#43019);
#12493=VERTEX_POINT('',#43021);
#12494=VERTEX_POINT('',#43023);
#12495=VERTEX_POINT('',#43025);
#12496=VERTEX_POINT('',#43027);
#12497=VERTEX_POINT('',#43029);
#12498=VERTEX_POINT('',#43031);
#12499=VERTEX_POINT('',#43033);
#12500=VERTEX_POINT('',#43035);
#12501=VERTEX_POINT('',#43037);
#12502=VERTEX_POINT('',#43039);
#12503=VERTEX_POINT('',#43041);
#12504=VERTEX_POINT('',#43043);
#12505=VERTEX_POINT('',#43045);
#12506=VERTEX_POINT('',#43047);
#12507=VERTEX_POINT('',#43049);
#12508=VERTEX_POINT('',#43051);
#12509=VERTEX_POINT('',#43053);
#12510=VERTEX_POINT('',#43055);
#12511=VERTEX_POINT('',#43057);
#12512=VERTEX_POINT('',#43059);
#12513=VERTEX_POINT('',#43061);
#12514=VERTEX_POINT('',#43063);
#12515=VERTEX_POINT('',#43065);
#12516=VERTEX_POINT('',#43067);
#12517=VERTEX_POINT('',#43069);
#12518=VERTEX_POINT('',#43071);
#12519=VERTEX_POINT('',#43073);
#12520=VERTEX_POINT('',#43075);
#12521=VERTEX_POINT('',#43077);
#12522=VERTEX_POINT('',#43079);
#12523=VERTEX_POINT('',#43081);
#12524=VERTEX_POINT('',#43083);
#12525=VERTEX_POINT('',#43085);
#12526=VERTEX_POINT('',#43087);
#12527=VERTEX_POINT('',#43089);
#12528=VERTEX_POINT('',#43091);
#12529=VERTEX_POINT('',#43093);
#12530=VERTEX_POINT('',#43095);
#12531=VERTEX_POINT('',#43097);
#12532=VERTEX_POINT('',#43099);
#12533=VERTEX_POINT('',#43101);
#12534=VERTEX_POINT('',#43103);
#12535=VERTEX_POINT('',#43105);
#12536=VERTEX_POINT('',#43107);
#12537=VERTEX_POINT('',#43109);
#12538=VERTEX_POINT('',#43111);
#12539=VERTEX_POINT('',#43113);
#12540=VERTEX_POINT('',#43115);
#12541=VERTEX_POINT('',#43117);
#12542=VERTEX_POINT('',#43119);
#12543=VERTEX_POINT('',#43121);
#12544=VERTEX_POINT('',#43123);
#12545=VERTEX_POINT('',#43125);
#12546=VERTEX_POINT('',#43127);
#12547=VERTEX_POINT('',#43129);
#12548=VERTEX_POINT('',#43131);
#12549=VERTEX_POINT('',#43133);
#12550=VERTEX_POINT('',#43135);
#12551=VERTEX_POINT('',#43137);
#12552=VERTEX_POINT('',#43139);
#12553=VERTEX_POINT('',#43141);
#12554=VERTEX_POINT('',#43143);
#12555=VERTEX_POINT('',#43145);
#12556=VERTEX_POINT('',#43147);
#12557=VERTEX_POINT('',#43149);
#12558=VERTEX_POINT('',#43151);
#12559=VERTEX_POINT('',#43153);
#12560=VERTEX_POINT('',#43155);
#12561=VERTEX_POINT('',#43157);
#12562=VERTEX_POINT('',#43159);
#12563=VERTEX_POINT('',#43161);
#12564=VERTEX_POINT('',#43163);
#12565=VERTEX_POINT('',#43165);
#12566=VERTEX_POINT('',#43167);
#12567=VERTEX_POINT('',#43169);
#12568=VERTEX_POINT('',#43171);
#12569=VERTEX_POINT('',#43173);
#12570=VERTEX_POINT('',#43175);
#12571=VERTEX_POINT('',#43177);
#12572=VERTEX_POINT('',#43179);
#12573=VERTEX_POINT('',#43181);
#12574=VERTEX_POINT('',#43183);
#12575=VERTEX_POINT('',#43185);
#12576=VERTEX_POINT('',#43187);
#12577=VERTEX_POINT('',#43189);
#12578=VERTEX_POINT('',#43191);
#12579=VERTEX_POINT('',#43193);
#12580=VERTEX_POINT('',#43195);
#12581=VERTEX_POINT('',#43197);
#12582=VERTEX_POINT('',#43199);
#12583=VERTEX_POINT('',#43201);
#12584=VERTEX_POINT('',#43203);
#12585=VERTEX_POINT('',#43205);
#12586=VERTEX_POINT('',#43207);
#12587=VERTEX_POINT('',#43209);
#12588=VERTEX_POINT('',#43211);
#12589=VERTEX_POINT('',#43213);
#12590=VERTEX_POINT('',#43215);
#12591=VERTEX_POINT('',#43217);
#12592=VERTEX_POINT('',#43219);
#12593=VERTEX_POINT('',#43221);
#12594=VERTEX_POINT('',#43223);
#12595=VERTEX_POINT('',#43225);
#12596=VERTEX_POINT('',#43227);
#12597=VERTEX_POINT('',#43229);
#12598=VERTEX_POINT('',#43231);
#12599=VERTEX_POINT('',#43233);
#12600=VERTEX_POINT('',#43235);
#12601=VERTEX_POINT('',#43237);
#12602=VERTEX_POINT('',#43239);
#12603=VERTEX_POINT('',#43241);
#12604=VERTEX_POINT('',#43243);
#12605=VERTEX_POINT('',#43245);
#12606=VERTEX_POINT('',#43247);
#12607=VERTEX_POINT('',#43249);
#12608=VERTEX_POINT('',#43251);
#12609=VERTEX_POINT('',#43253);
#12610=VERTEX_POINT('',#43255);
#12611=VERTEX_POINT('',#43257);
#12612=VERTEX_POINT('',#43259);
#12613=VERTEX_POINT('',#43261);
#12614=VERTEX_POINT('',#43263);
#12615=VERTEX_POINT('',#43265);
#12616=VERTEX_POINT('',#43267);
#12617=VERTEX_POINT('',#43269);
#12618=VERTEX_POINT('',#43271);
#12619=VERTEX_POINT('',#43273);
#12620=VERTEX_POINT('',#43275);
#12621=VERTEX_POINT('',#43277);
#12622=VERTEX_POINT('',#43279);
#12623=VERTEX_POINT('',#43281);
#12624=VERTEX_POINT('',#43283);
#12625=VERTEX_POINT('',#43285);
#12626=VERTEX_POINT('',#43287);
#12627=VERTEX_POINT('',#43289);
#12628=VERTEX_POINT('',#43291);
#12629=VERTEX_POINT('',#43293);
#12630=VERTEX_POINT('',#43295);
#12631=VERTEX_POINT('',#43297);
#12632=VERTEX_POINT('',#43299);
#12633=VERTEX_POINT('',#43303);
#12634=VERTEX_POINT('',#43305);
#12635=VERTEX_POINT('',#43309);
#12636=VERTEX_POINT('',#43311);
#12637=VERTEX_POINT('',#43318);
#12638=VERTEX_POINT('',#43322);
#12639=VERTEX_POINT('',#43328);
#12640=VERTEX_POINT('',#43330);
#12641=VERTEX_POINT('',#43334);
#12642=VERTEX_POINT('',#43336);
#12643=VERTEX_POINT('',#43343);
#12644=VERTEX_POINT('',#43347);
#12645=VERTEX_POINT('',#43353);
#12646=VERTEX_POINT('',#43355);
#12647=VERTEX_POINT('',#43359);
#12648=VERTEX_POINT('',#43361);
#12649=VERTEX_POINT('',#43368);
#12650=VERTEX_POINT('',#43372);
#12651=VERTEX_POINT('',#43378);
#12652=VERTEX_POINT('',#43380);
#12653=VERTEX_POINT('',#43384);
#12654=VERTEX_POINT('',#43386);
#12655=VERTEX_POINT('',#43390);
#12656=VERTEX_POINT('',#43394);
#12657=VERTEX_POINT('',#43401);
#12658=VERTEX_POINT('',#43404);
#12659=VERTEX_POINT('',#43406);
#12660=VERTEX_POINT('',#43409);
#12661=VERTEX_POINT('',#43411);
#12662=VERTEX_POINT('',#43414);
#12663=VERTEX_POINT('',#43416);
#12664=VERTEX_POINT('',#43419);
#12665=VERTEX_POINT('',#43421);
#12666=VERTEX_POINT('',#43424);
#12667=VERTEX_POINT('',#43426);
#12668=VERTEX_POINT('',#43429);
#12669=VERTEX_POINT('',#43431);
#12670=VERTEX_POINT('',#43434);
#12671=VERTEX_POINT('',#43436);
#12672=VERTEX_POINT('',#43439);
#12673=VERTEX_POINT('',#43441);
#12674=VERTEX_POINT('',#43444);
#12675=VERTEX_POINT('',#43446);
#12676=VERTEX_POINT('',#43449);
#12677=VERTEX_POINT('',#43451);
#12678=VERTEX_POINT('',#43454);
#12679=VERTEX_POINT('',#43456);
#12680=VERTEX_POINT('',#43459);
#12681=VERTEX_POINT('',#43461);
#12682=VERTEX_POINT('',#43464);
#12683=VERTEX_POINT('',#43466);
#12684=VERTEX_POINT('',#43469);
#12685=VERTEX_POINT('',#43471);
#12686=VERTEX_POINT('',#43474);
#12687=VERTEX_POINT('',#43476);
#12688=VERTEX_POINT('',#43479);
#12689=VERTEX_POINT('',#43481);
#12690=VERTEX_POINT('',#43484);
#12691=VERTEX_POINT('',#43486);
#12692=VERTEX_POINT('',#43489);
#12693=VERTEX_POINT('',#43491);
#12694=VERTEX_POINT('',#43494);
#12695=VERTEX_POINT('',#43496);
#12696=VERTEX_POINT('',#43499);
#12697=VERTEX_POINT('',#43501);
#12698=VERTEX_POINT('',#43504);
#12699=VERTEX_POINT('',#43506);
#12700=VERTEX_POINT('',#43509);
#12701=VERTEX_POINT('',#43511);
#12702=VERTEX_POINT('',#43514);
#12703=VERTEX_POINT('',#43516);
#12704=VERTEX_POINT('',#43519);
#12705=VERTEX_POINT('',#43521);
#12706=VERTEX_POINT('',#43524);
#12707=VERTEX_POINT('',#43526);
#12708=VERTEX_POINT('',#43529);
#12709=VERTEX_POINT('',#43530);
#12710=VERTEX_POINT('',#43532);
#12711=VERTEX_POINT('',#43534);
#12712=VERTEX_POINT('',#43536);
#12713=VERTEX_POINT('',#43538);
#12714=VERTEX_POINT('',#43540);
#12715=VERTEX_POINT('',#43542);
#12716=VERTEX_POINT('',#43546);
#12717=VERTEX_POINT('',#43550);
#12718=VERTEX_POINT('',#43556);
#12719=VERTEX_POINT('',#43560);
#12720=VERTEX_POINT('',#43566);
#12721=VERTEX_POINT('',#43570);
#12722=VERTEX_POINT('',#43576);
#12723=VERTEX_POINT('',#43580);
#12724=VERTEX_POINT('',#43586);
#12725=VERTEX_POINT('',#43590);
#12726=VERTEX_POINT('',#43596);
#12727=VERTEX_POINT('',#43600);
#12728=VERTEX_POINT('',#43606);
#12729=VERTEX_POINT('',#43610);
#12730=VERTEX_POINT('',#43616);
#12731=VERTEX_POINT('',#43620);
#12732=VERTEX_POINT('',#43626);
#12733=VERTEX_POINT('',#43630);
#12734=VERTEX_POINT('',#43636);
#12735=VERTEX_POINT('',#43640);
#12736=VERTEX_POINT('',#43646);
#12737=VERTEX_POINT('',#43650);
#12738=VERTEX_POINT('',#43656);
#12739=VERTEX_POINT('',#43660);
#12740=VERTEX_POINT('',#43666);
#12741=VERTEX_POINT('',#43670);
#12742=VERTEX_POINT('',#43676);
#12743=VERTEX_POINT('',#43680);
#12744=VERTEX_POINT('',#43686);
#12745=VERTEX_POINT('',#43690);
#12746=VERTEX_POINT('',#43696);
#12747=VERTEX_POINT('',#43700);
#12748=VERTEX_POINT('',#43706);
#12749=VERTEX_POINT('',#43710);
#12750=VERTEX_POINT('',#43716);
#12751=VERTEX_POINT('',#43720);
#12752=VERTEX_POINT('',#43726);
#12753=VERTEX_POINT('',#43730);
#12754=VERTEX_POINT('',#43736);
#12755=VERTEX_POINT('',#43740);
#12756=VERTEX_POINT('',#43744);
#12757=VERTEX_POINT('',#43750);
#12758=VERTEX_POINT('',#43756);
#12759=VERTEX_POINT('',#43760);
#12760=VERTEX_POINT('',#43766);
#12761=VERTEX_POINT('',#43770);
#12762=VERTEX_POINT('',#43776);
#12763=VERTEX_POINT('',#43780);
#12764=VERTEX_POINT('',#43786);
#12765=VERTEX_POINT('',#43790);
#12766=VERTEX_POINT('',#43796);
#12767=VERTEX_POINT('',#43800);
#12768=VERTEX_POINT('',#43806);
#12769=VERTEX_POINT('',#43810);
#12770=VERTEX_POINT('',#43816);
#12771=VERTEX_POINT('',#43820);
#12772=VERTEX_POINT('',#43826);
#12773=VERTEX_POINT('',#43830);
#12774=VERTEX_POINT('',#43836);
#12775=VERTEX_POINT('',#43840);
#12776=VERTEX_POINT('',#43846);
#12777=VERTEX_POINT('',#43850);
#12778=VERTEX_POINT('',#43856);
#12779=VERTEX_POINT('',#43860);
#12780=VERTEX_POINT('',#43866);
#12781=VERTEX_POINT('',#43870);
#12782=VERTEX_POINT('',#43876);
#12783=VERTEX_POINT('',#43880);
#12784=VERTEX_POINT('',#43886);
#12785=VERTEX_POINT('',#43890);
#12786=VERTEX_POINT('',#43896);
#12787=VERTEX_POINT('',#43900);
#12788=VERTEX_POINT('',#43906);
#12789=VERTEX_POINT('',#43910);
#12790=VERTEX_POINT('',#43916);
#12791=VERTEX_POINT('',#43920);
#12792=VERTEX_POINT('',#43926);
#12793=VERTEX_POINT('',#43930);
#12794=VERTEX_POINT('',#43936);
#12795=VERTEX_POINT('',#43940);
#12796=VERTEX_POINT('',#43946);
#12797=VERTEX_POINT('',#43950);
#12798=VERTEX_POINT('',#43956);
#12799=VERTEX_POINT('',#43960);
#12800=VERTEX_POINT('',#43966);
#12801=VERTEX_POINT('',#43970);
#12802=VERTEX_POINT('',#43976);
#12803=VERTEX_POINT('',#43980);
#12804=VERTEX_POINT('',#43986);
#12805=VERTEX_POINT('',#43990);
#12806=VERTEX_POINT('',#43996);
#12807=VERTEX_POINT('',#43997);
#12808=VERTEX_POINT('',#43999);
#12809=VERTEX_POINT('',#44001);
#12810=VERTEX_POINT('',#44009);
#12811=VERTEX_POINT('',#44011);
#12812=VERTEX_POINT('',#44014);
#12813=VERTEX_POINT('',#44016);
#12814=VERTEX_POINT('',#44019);
#12815=VERTEX_POINT('',#44021);
#12816=VERTEX_POINT('',#44024);
#12817=VERTEX_POINT('',#44026);
#12818=VERTEX_POINT('',#44029);
#12819=VERTEX_POINT('',#44031);
#12820=VERTEX_POINT('',#44034);
#12821=VERTEX_POINT('',#44036);
#12822=VERTEX_POINT('',#44039);
#12823=VERTEX_POINT('',#44041);
#12824=VERTEX_POINT('',#44044);
#12825=VERTEX_POINT('',#44046);
#12826=VERTEX_POINT('',#44049);
#12827=VERTEX_POINT('',#44051);
#12828=VERTEX_POINT('',#44054);
#12829=VERTEX_POINT('',#44056);
#12830=VERTEX_POINT('',#44059);
#12831=VERTEX_POINT('',#44061);
#12832=VERTEX_POINT('',#44064);
#12833=VERTEX_POINT('',#44066);
#12834=VERTEX_POINT('',#44069);
#12835=VERTEX_POINT('',#44071);
#12836=VERTEX_POINT('',#44074);
#12837=VERTEX_POINT('',#44076);
#12838=VERTEX_POINT('',#44079);
#12839=VERTEX_POINT('',#44081);
#12840=VERTEX_POINT('',#44084);
#12841=VERTEX_POINT('',#44086);
#12842=VERTEX_POINT('',#44089);
#12843=VERTEX_POINT('',#44091);
#12844=VERTEX_POINT('',#44094);
#12845=VERTEX_POINT('',#44096);
#12846=VERTEX_POINT('',#44099);
#12847=VERTEX_POINT('',#44101);
#12848=VERTEX_POINT('',#44104);
#12849=VERTEX_POINT('',#44106);
#12850=VERTEX_POINT('',#44109);
#12851=VERTEX_POINT('',#44111);
#12852=VERTEX_POINT('',#44114);
#12853=VERTEX_POINT('',#44116);
#12854=VERTEX_POINT('',#44119);
#12855=VERTEX_POINT('',#44121);
#12856=VERTEX_POINT('',#44124);
#12857=VERTEX_POINT('',#44126);
#12858=VERTEX_POINT('',#44129);
#12859=VERTEX_POINT('',#44131);
#12860=VERTEX_POINT('',#44134);
#12861=VERTEX_POINT('',#44136);
#12862=VERTEX_POINT('',#44139);
#12863=VERTEX_POINT('',#44141);
#12864=VERTEX_POINT('',#44144);
#12865=VERTEX_POINT('',#44146);
#12866=VERTEX_POINT('',#44149);
#12867=VERTEX_POINT('',#44151);
#12868=VERTEX_POINT('',#44154);
#12869=VERTEX_POINT('',#44155);
#12870=VERTEX_POINT('',#44157);
#12871=VERTEX_POINT('',#44159);
#12872=VERTEX_POINT('',#44161);
#12873=VERTEX_POINT('',#44163);
#12874=VERTEX_POINT('',#44165);
#12875=VERTEX_POINT('',#44167);
#12876=VERTEX_POINT('',#44173);
#12877=VERTEX_POINT('',#44175);
#12878=VERTEX_POINT('',#44183);
#12879=VERTEX_POINT('',#44185);
#12880=VERTEX_POINT('',#44193);
#12881=VERTEX_POINT('',#44197);
#12882=VERTEX_POINT('',#44201);
#12883=VERTEX_POINT('',#44203);
#12884=VERTEX_POINT('',#44211);
#12885=VERTEX_POINT('',#44213);
#12886=VERTEX_POINT('',#44221);
#12887=VERTEX_POINT('',#44225);
#12888=VERTEX_POINT('',#44229);
#12889=VERTEX_POINT('',#44231);
#12890=VERTEX_POINT('',#44239);
#12891=VERTEX_POINT('',#44241);
#12892=VERTEX_POINT('',#44249);
#12893=VERTEX_POINT('',#44253);
#12894=VERTEX_POINT('',#44257);
#12895=VERTEX_POINT('',#44261);
#12896=VERTEX_POINT('',#44267);
#12897=VERTEX_POINT('',#44269);
#12898=VERTEX_POINT('',#44277);
#12899=VERTEX_POINT('',#44279);
#12900=VERTEX_POINT('',#44287);
#12901=VERTEX_POINT('',#44291);
#12902=VERTEX_POINT('',#44295);
#12903=VERTEX_POINT('',#44297);
#12904=VERTEX_POINT('',#44305);
#12905=VERTEX_POINT('',#44307);
#12906=VERTEX_POINT('',#44315);
#12907=VERTEX_POINT('',#44319);
#12908=VERTEX_POINT('',#44323);
#12909=VERTEX_POINT('',#44325);
#12910=VERTEX_POINT('',#44333);
#12911=VERTEX_POINT('',#44335);
#12912=VERTEX_POINT('',#44343);
#12913=VERTEX_POINT('',#44347);
#12914=VERTEX_POINT('',#44351);
#12915=VERTEX_POINT('',#44353);
#12916=VERTEX_POINT('',#44361);
#12917=VERTEX_POINT('',#44363);
#12918=VERTEX_POINT('',#44371);
#12919=VERTEX_POINT('',#44375);
#12920=VERTEX_POINT('',#44379);
#12921=VERTEX_POINT('',#44381);
#12922=VERTEX_POINT('',#44389);
#12923=VERTEX_POINT('',#44391);
#12924=VERTEX_POINT('',#44399);
#12925=VERTEX_POINT('',#44403);
#12926=VERTEX_POINT('',#44407);
#12927=VERTEX_POINT('',#44409);
#12928=VERTEX_POINT('',#44417);
#12929=VERTEX_POINT('',#44419);
#12930=VERTEX_POINT('',#44427);
#12931=VERTEX_POINT('',#44431);
#12932=VERTEX_POINT('',#44435);
#12933=VERTEX_POINT('',#44437);
#12934=VERTEX_POINT('',#44445);
#12935=VERTEX_POINT('',#44447);
#12936=VERTEX_POINT('',#44455);
#12937=VERTEX_POINT('',#44457);
#12938=VERTEX_POINT('',#44465);
#12939=VERTEX_POINT('',#44469);
#12940=VERTEX_POINT('',#44473);
#12941=VERTEX_POINT('',#44475);
#12942=VERTEX_POINT('',#44483);
#12943=VERTEX_POINT('',#44485);
#12944=VERTEX_POINT('',#44493);
#12945=VERTEX_POINT('',#44497);
#12946=VERTEX_POINT('',#44501);
#12947=VERTEX_POINT('',#44503);
#12948=VERTEX_POINT('',#44511);
#12949=VERTEX_POINT('',#44513);
#12950=VERTEX_POINT('',#44521);
#12951=VERTEX_POINT('',#44525);
#12952=VERTEX_POINT('',#44529);
#12953=VERTEX_POINT('',#44533);
#12954=VERTEX_POINT('',#44539);
#12955=VERTEX_POINT('',#44541);
#12956=VERTEX_POINT('',#44549);
#12957=VERTEX_POINT('',#44551);
#12958=VERTEX_POINT('',#44559);
#12959=VERTEX_POINT('',#44563);
#12960=VERTEX_POINT('',#44567);
#12961=VERTEX_POINT('',#44569);
#12962=VERTEX_POINT('',#44573);
#12963=VERTEX_POINT('',#44577);
#12964=VERTEX_POINT('',#44581);
#12965=VERTEX_POINT('',#44583);
#12966=VERTEX_POINT('',#44587);
#12967=VERTEX_POINT('',#44591);
#12968=VERTEX_POINT('',#44595);
#12969=VERTEX_POINT('',#44597);
#12970=VERTEX_POINT('',#44608);
#12971=VERTEX_POINT('',#44609);
#12972=VERTEX_POINT('',#44614);
#12973=VERTEX_POINT('',#44620);
#12974=VERTEX_POINT('',#44622);
#12975=VERTEX_POINT('',#44626);
#12976=VERTEX_POINT('',#44643);
#12977=VERTEX_POINT('',#44645);
#12978=VERTEX_POINT('',#44655);
#12979=VERTEX_POINT('',#44657);
#12980=VERTEX_POINT('',#44671);
#12981=VERTEX_POINT('',#44673);
#12982=VERTEX_POINT('',#44687);
#12983=VERTEX_POINT('',#44689);
#12984=VERTEX_POINT('',#44703);
#12985=VERTEX_POINT('',#44705);
#12986=VERTEX_POINT('',#44715);
#12987=VERTEX_POINT('',#44717);
#12988=VERTEX_POINT('',#44731);
#12989=VERTEX_POINT('',#44733);
#12990=VERTEX_POINT('',#44747);
#12991=VERTEX_POINT('',#44749);
#12992=VERTEX_POINT('',#44763);
#12993=VERTEX_POINT('',#44765);
#12994=VERTEX_POINT('',#44779);
#12995=VERTEX_POINT('',#44781);
#12996=VERTEX_POINT('',#44797);
#12997=VERTEX_POINT('',#44799);
#12998=VERTEX_POINT('',#44813);
#12999=VERTEX_POINT('',#44815);
#13000=VERTEX_POINT('',#44825);
#13001=VERTEX_POINT('',#44827);
#13002=VERTEX_POINT('',#44842);
#13003=VERTEX_POINT('',#44846);
#13004=VERTEX_POINT('',#44853);
#13005=VERTEX_POINT('',#44855);
#13006=VERTEX_POINT('',#44864);
#13007=VERTEX_POINT('',#44868);
#13008=VERTEX_POINT('',#44878);
#13009=VERTEX_POINT('',#44882);
#13010=VERTEX_POINT('',#44889);
#13011=VERTEX_POINT('',#44891);
#13012=VERTEX_POINT('',#44900);
#13013=VERTEX_POINT('',#44904);
#13014=VERTEX_POINT('',#44914);
#13015=VERTEX_POINT('',#44918);
#13016=VERTEX_POINT('',#44925);
#13017=VERTEX_POINT('',#44927);
#13018=VERTEX_POINT('',#44936);
#13019=VERTEX_POINT('',#44940);
#13020=VERTEX_POINT('',#44947);
#13021=VERTEX_POINT('',#44949);
#13022=VERTEX_POINT('',#44960);
#13023=VERTEX_POINT('',#44961);
#13024=VERTEX_POINT('',#44963);
#13025=VERTEX_POINT('',#44965);
#13026=VERTEX_POINT('',#44969);
#13027=VERTEX_POINT('',#44971);
#13028=VERTEX_POINT('',#44975);
#13029=VERTEX_POINT('',#44977);
#13030=VERTEX_POINT('',#44985);
#13031=VERTEX_POINT('',#44986);
#13032=VERTEX_POINT('',#44997);
#13033=VERTEX_POINT('',#45008);
#13034=VERTEX_POINT('',#45010);
#13035=VERTEX_POINT('',#45066);
#13036=VERTEX_POINT('',#45069);
#13037=VERTEX_POINT('',#45073);
#13038=VERTEX_POINT('',#45078);
#13039=VERTEX_POINT('',#45082);
#13040=VERTEX_POINT('',#45086);
#13041=VERTEX_POINT('',#45089);
#13042=VERTEX_POINT('',#45093);
#13043=VERTEX_POINT('',#45096);
#13044=VERTEX_POINT('',#45100);
#13045=VERTEX_POINT('',#45103);
#13046=VERTEX_POINT('',#45107);
#13047=VERTEX_POINT('',#45110);
#13048=VERTEX_POINT('',#45114);
#13049=VERTEX_POINT('',#45117);
#13050=VERTEX_POINT('',#45121);
#13051=VERTEX_POINT('',#45127);
#13052=VERTEX_POINT('',#45129);
#13053=VERTEX_POINT('',#45133);
#13054=VERTEX_POINT('',#45136);
#13055=VERTEX_POINT('',#45140);
#13056=VERTEX_POINT('',#45143);
#13057=VERTEX_POINT('',#45147);
#13058=VERTEX_POINT('',#45151);
#13059=VERTEX_POINT('',#45155);
#13060=VERTEX_POINT('',#45158);
#13061=VERTEX_POINT('',#45162);
#13062=VERTEX_POINT('',#45165);
#13063=VERTEX_POINT('',#45169);
#13064=VERTEX_POINT('',#45172);
#13065=VERTEX_POINT('',#45176);
#13066=VERTEX_POINT('',#45180);
#13067=VERTEX_POINT('',#45186);
#13068=VERTEX_POINT('',#45188);
#13069=VERTEX_POINT('',#45190);
#13070=VERTEX_POINT('',#45194);
#13071=VERTEX_POINT('',#45198);
#13072=VERTEX_POINT('',#45201);
#13073=VERTEX_POINT('',#45203);
#13074=VERTEX_POINT('',#45207);
#13075=VERTEX_POINT('',#45212);
#13076=VERTEX_POINT('',#45216);
#13077=VERTEX_POINT('',#45219);
#13078=VERTEX_POINT('',#45225);
#13079=VERTEX_POINT('',#45227);
#13080=VERTEX_POINT('',#45231);
#13081=VERTEX_POINT('',#45234);
#13082=VERTEX_POINT('',#45238);
#13083=VERTEX_POINT('',#45244);
#13084=VERTEX_POINT('',#45247);
#13085=VERTEX_POINT('',#45251);
#13086=VERTEX_POINT('',#45255);
#13087=VERTEX_POINT('',#45261);
#13088=VERTEX_POINT('',#45263);
#13089=VERTEX_POINT('',#45267);
#13090=VERTEX_POINT('',#45270);
#13091=VERTEX_POINT('',#45276);
#13092=VERTEX_POINT('',#45281);
#13093=VERTEX_POINT('',#45282);
#13094=VERTEX_POINT('',#45284);
#13095=VERTEX_POINT('',#45286);
#13096=VERTEX_POINT('',#45293);
#13097=VERTEX_POINT('',#45295);
#13098=VERTEX_POINT('',#45302);
#13099=VERTEX_POINT('',#45304);
#13100=VERTEX_POINT('',#45310);
#13101=VERTEX_POINT('',#45311);
#13102=VERTEX_POINT('',#45313);
#13103=VERTEX_POINT('',#45315);
#13104=VERTEX_POINT('',#45322);
#13105=VERTEX_POINT('',#45323);
#13106=VERTEX_POINT('',#45325);
#13107=VERTEX_POINT('',#45327);
#13108=VERTEX_POINT('',#45348);
#13109=VERTEX_POINT('',#45349);
#13110=VERTEX_POINT('',#45351);
#13111=VERTEX_POINT('',#45357);
#13112=VERTEX_POINT('',#45358);
#13113=VERTEX_POINT('',#45360);
#13114=VERTEX_POINT('',#45366);
#13115=VERTEX_POINT('',#45367);
#13116=VERTEX_POINT('',#45372);
#13117=VERTEX_POINT('',#45373);
#13118=VERTEX_POINT('',#45377);
#13119=VERTEX_POINT('',#45381);
#13120=VERTEX_POINT('',#45382);
#13121=VERTEX_POINT('',#45384);
#13122=VERTEX_POINT('',#45393);
#13123=VERTEX_POINT('',#45394);
#13124=VERTEX_POINT('',#45402);
#13125=VERTEX_POINT('',#45403);
#13126=VERTEX_POINT('',#45414);
#13127=VERTEX_POINT('',#45415);
#13128=VERTEX_POINT('',#45431);
#13129=VERTEX_POINT('',#45433);
#13130=VERTEX_POINT('',#45437);
#13131=VERTEX_POINT('',#45438);
#13132=VERTEX_POINT('',#45445);
#13133=VERTEX_POINT('',#45452);
#13134=VERTEX_POINT('',#45459);
#13135=VERTEX_POINT('',#45466);
#13136=VERTEX_POINT('',#45473);
#13137=VERTEX_POINT('',#45487);
#13138=VERTEX_POINT('',#45488);
#13139=VERTEX_POINT('',#45503);
#13140=VERTEX_POINT('',#45510);
#13141=VERTEX_POINT('',#45519);
#13142=VERTEX_POINT('',#45520);
#13143=VERTEX_POINT('',#45535);
#13144=VERTEX_POINT('',#45542);
#13145=VERTEX_POINT('',#45551);
#13146=VERTEX_POINT('',#45552);
#13147=VERTEX_POINT('',#45567);
#13148=VERTEX_POINT('',#45574);
#13149=VERTEX_POINT('',#45613);
#13150=VERTEX_POINT('',#45614);
#13151=VERTEX_POINT('',#45679);
#13152=VERTEX_POINT('',#45680);
#13153=VERTEX_POINT('',#45685);
#13154=VERTEX_POINT('',#45686);
#13155=VERTEX_POINT('',#45751);
#13156=VERTEX_POINT('',#45752);
#13157=VERTEX_POINT('',#45757);
#13158=VERTEX_POINT('',#45758);
#13159=VERTEX_POINT('',#45793);
#13160=VERTEX_POINT('',#45794);
#13161=VERTEX_POINT('',#45799);
#13162=VERTEX_POINT('',#45801);
#13163=VERTEX_POINT('',#45805);
#13164=VERTEX_POINT('',#45809);
#13165=VERTEX_POINT('',#45813);
#13166=VERTEX_POINT('',#45817);
#13167=VERTEX_POINT('',#45821);
#13168=VERTEX_POINT('',#45825);
#13169=VERTEX_POINT('',#45827);
#13170=VERTEX_POINT('',#45831);
#13171=VERTEX_POINT('',#45833);
#13172=VERTEX_POINT('',#45837);
#13173=VERTEX_POINT('',#45857);
#13174=VERTEX_POINT('',#45861);
#13175=VERTEX_POINT('',#45864);
#13176=VERTEX_POINT('',#45871);
#13177=VERTEX_POINT('',#45872);
#13178=VERTEX_POINT('',#45874);
#13179=VERTEX_POINT('',#45876);
#13180=VERTEX_POINT('',#45880);
#13181=VERTEX_POINT('',#45881);
#13182=VERTEX_POINT('',#45886);
#13183=VERTEX_POINT('',#45887);
#13184=VERTEX_POINT('',#45892);
#13185=VERTEX_POINT('',#45893);
#13186=VERTEX_POINT('',#45898);
#13187=VERTEX_POINT('',#45899);
#13188=VERTEX_POINT('',#45904);
#13189=VERTEX_POINT('',#45905);
#13190=VERTEX_POINT('',#45910);
#13191=VERTEX_POINT('',#45911);
#13192=VERTEX_POINT('',#45919);
#13193=VERTEX_POINT('',#45921);
#13194=VERTEX_POINT('',#45925);
#13195=VERTEX_POINT('',#45929);
#13196=VERTEX_POINT('',#45933);
#13197=VERTEX_POINT('',#45937);
#13198=VERTEX_POINT('',#45939);
#13199=VERTEX_POINT('',#45941);
#13200=VERTEX_POINT('',#45943);
#13201=VERTEX_POINT('',#45945);
#13202=VERTEX_POINT('',#45946);
#13203=VERTEX_POINT('',#45948);
#13204=VERTEX_POINT('',#45950);
#13205=VERTEX_POINT('',#45952);
#13206=VERTEX_POINT('',#45954);
#13207=VERTEX_POINT('',#45956);
#13208=VERTEX_POINT('',#45958);
#13209=VERTEX_POINT('',#45962);
#13210=VERTEX_POINT('',#45964);
#13211=VERTEX_POINT('',#45968);
#13212=VERTEX_POINT('',#45969);
#13213=VERTEX_POINT('',#45974);
#13214=VERTEX_POINT('',#45975);
#13215=VERTEX_POINT('',#45980);
#13216=VERTEX_POINT('',#45981);
#13217=VERTEX_POINT('',#45986);
#13218=VERTEX_POINT('',#45991);
#13219=VERTEX_POINT('',#45995);
#13220=VERTEX_POINT('',#46007);
#13221=VERTEX_POINT('',#46009);
#13222=VERTEX_POINT('',#46011);
#13223=VERTEX_POINT('',#46013);
#13224=VERTEX_POINT('',#46016);
#13225=VERTEX_POINT('',#46017);
#13226=VERTEX_POINT('',#46019);
#13227=VERTEX_POINT('',#46021);
#13228=VERTEX_POINT('',#46025);
#13229=VERTEX_POINT('',#46026);
#13230=VERTEX_POINT('',#46031);
#13231=VERTEX_POINT('',#46032);
#13232=VERTEX_POINT('',#46037);
#13233=VERTEX_POINT('',#46038);
#13234=VERTEX_POINT('',#46043);
#13235=VERTEX_POINT('',#46044);
#13236=VERTEX_POINT('',#46049);
#13237=VERTEX_POINT('',#46050);
#13238=VERTEX_POINT('',#46055);
#13239=VERTEX_POINT('',#46056);
#13240=VERTEX_POINT('',#46091);
#13241=VERTEX_POINT('',#46092);
#13242=VERTEX_POINT('',#46096);
#13243=VERTEX_POINT('',#46098);
#13244=VERTEX_POINT('',#46100);
#13245=VERTEX_POINT('',#46106);
#13246=VERTEX_POINT('',#46110);
#13247=VERTEX_POINT('',#46112);
#13248=VERTEX_POINT('',#46115);
#13249=VERTEX_POINT('',#46119);
#13250=VERTEX_POINT('',#46123);
#13251=VERTEX_POINT('',#46127);
#13252=VERTEX_POINT('',#46129);
#13253=VERTEX_POINT('',#46133);
#13254=VERTEX_POINT('',#46135);
#13255=VERTEX_POINT('',#46139);
#13256=VERTEX_POINT('',#46143);
#13257=VERTEX_POINT('',#46147);
#13258=VERTEX_POINT('',#46149);
#13259=VERTEX_POINT('',#46153);
#13260=VERTEX_POINT('',#46157);
#13261=VERTEX_POINT('',#46161);
#13262=VERTEX_POINT('',#46163);
#13263=VERTEX_POINT('',#46167);
#13264=VERTEX_POINT('',#46171);
#13265=VERTEX_POINT('',#46175);
#13266=VERTEX_POINT('',#46177);
#13267=VERTEX_POINT('',#46185);
#13268=VERTEX_POINT('',#46186);
#13269=VERTEX_POINT('',#46189);
#13270=VERTEX_POINT('',#46193);
#13271=VERTEX_POINT('',#46194);
#13272=VERTEX_POINT('',#46199);
#13273=VERTEX_POINT('',#46202);
#13274=VERTEX_POINT('',#46206);
#13275=VERTEX_POINT('',#46212);
#13276=VERTEX_POINT('',#46216);
#13277=VERTEX_POINT('',#46222);
#13278=VERTEX_POINT('',#46223);
#13279=VERTEX_POINT('',#46225);
#13280=VERTEX_POINT('',#46229);
#13281=VERTEX_POINT('',#46230);
#13282=VERTEX_POINT('',#46235);
#13283=VERTEX_POINT('',#46236);
#13284=VERTEX_POINT('',#46238);
#13285=VERTEX_POINT('',#46242);
#13286=VERTEX_POINT('',#46243);
#13287=VERTEX_POINT('',#46245);
#13288=VERTEX_POINT('',#46249);
#13289=VERTEX_POINT('',#46250);
#13290=VERTEX_POINT('',#46258);
#13291=VERTEX_POINT('',#46259);
#13292=VERTEX_POINT('',#46261);
#13293=VERTEX_POINT('',#46268);
#13294=VERTEX_POINT('',#46269);
#13295=VERTEX_POINT('',#46271);
#13296=VERTEX_POINT('',#46275);
#13297=VERTEX_POINT('',#46276);
#13298=VERTEX_POINT('',#46278);
#13299=VERTEX_POINT('',#46309);
#13300=VERTEX_POINT('',#46310);
#13301=VERTEX_POINT('',#46315);
#13302=VERTEX_POINT('',#46316);
#13303=VERTEX_POINT('',#46320);
#13304=VERTEX_POINT('',#46354);
#13305=VERTEX_POINT('',#46355);
#13306=VERTEX_POINT('',#46357);
#13307=VERTEX_POINT('',#46361);
#13308=VERTEX_POINT('',#46362);
#13309=VERTEX_POINT('',#46367);
#13310=VERTEX_POINT('',#46368);
#13311=VERTEX_POINT('',#46371);
#13312=VERTEX_POINT('',#46375);
#13313=VERTEX_POINT('',#46376);
#13314=VERTEX_POINT('',#46379);
#13315=VERTEX_POINT('',#46384);
#13316=VERTEX_POINT('',#46386);
#13317=VERTEX_POINT('',#46390);
#13318=VERTEX_POINT('',#46394);
#13319=VERTEX_POINT('',#46396);
#13320=VERTEX_POINT('',#46400);
#13321=VERTEX_POINT('',#46401);
#13322=VERTEX_POINT('',#46403);
#13323=VERTEX_POINT('',#46407);
#13324=VERTEX_POINT('',#46408);
#13325=VERTEX_POINT('',#46410);
#13326=VERTEX_POINT('',#46415);
#13327=VERTEX_POINT('',#46428);
#13328=VERTEX_POINT('',#46439);
#13329=VERTEX_POINT('',#46440);
#13330=VERTEX_POINT('',#46442);
#13331=VERTEX_POINT('',#46446);
#13332=VERTEX_POINT('',#46447);
#13333=VERTEX_POINT('',#46452);
#13334=VERTEX_POINT('',#46453);
#13335=VERTEX_POINT('',#46455);
#13336=VERTEX_POINT('',#46459);
#13337=VERTEX_POINT('',#46460);
#13338=VERTEX_POINT('',#46462);
#13339=VERTEX_POINT('',#46466);
#13340=VERTEX_POINT('',#46467);
#13341=VERTEX_POINT('',#46475);
#13342=VERTEX_POINT('',#46476);
#13343=VERTEX_POINT('',#46478);
#13344=VERTEX_POINT('',#46485);
#13345=VERTEX_POINT('',#46486);
#13346=VERTEX_POINT('',#46488);
#13347=VERTEX_POINT('',#46492);
#13348=VERTEX_POINT('',#46493);
#13349=VERTEX_POINT('',#46495);
#13350=VERTEX_POINT('',#46645);
#13351=VERTEX_POINT('',#46678);
#13352=VERTEX_POINT('',#46680);
#13353=VERTEX_POINT('',#46695);
#13354=VERTEX_POINT('',#46702);
#13355=VERTEX_POINT('',#46703);
#13356=VERTEX_POINT('',#46705);
#13357=VERTEX_POINT('',#46716);
#13358=VERTEX_POINT('',#46729);
#13359=VERTEX_POINT('',#46730);
#13360=VERTEX_POINT('',#46777);
#13361=VERTEX_POINT('',#46778);
#13362=VERTEX_POINT('',#46825);
#13363=VERTEX_POINT('',#46826);
#13364=VERTEX_POINT('',#46873);
#13365=VERTEX_POINT('',#46874);
#13366=VERTEX_POINT('',#46927);
#13367=VERTEX_POINT('',#46928);
#13368=VERTEX_POINT('',#46975);
#13369=VERTEX_POINT('',#46976);
#13370=VERTEX_POINT('',#47023);
#13371=VERTEX_POINT('',#47024);
#13372=VERTEX_POINT('',#47077);
#13373=VERTEX_POINT('',#47078);
#13374=VERTEX_POINT('',#47125);
#13375=VERTEX_POINT('',#47126);
#13376=VERTEX_POINT('',#47173);
#13377=VERTEX_POINT('',#47174);
#13378=VERTEX_POINT('',#47221);
#13379=VERTEX_POINT('',#47222);
#13380=VERTEX_POINT('',#47275);
#13381=VERTEX_POINT('',#47276);
#13382=VERTEX_POINT('',#47323);
#13383=VERTEX_POINT('',#47324);
#13384=VERTEX_POINT('',#47371);
#13385=VERTEX_POINT('',#47372);
#13386=VERTEX_POINT('',#47425);
#13387=VERTEX_POINT('',#47426);
#13388=VERTEX_POINT('',#47473);
#13389=VERTEX_POINT('',#47474);
#13390=VERTEX_POINT('',#47521);
#13391=VERTEX_POINT('',#47522);
#13392=VERTEX_POINT('',#47569);
#13393=VERTEX_POINT('',#47570);
#13394=VERTEX_POINT('',#47623);
#13395=VERTEX_POINT('',#47624);
#13396=VERTEX_POINT('',#47671);
#13397=VERTEX_POINT('',#47672);
#13398=VERTEX_POINT('',#47674);
#13399=VERTEX_POINT('',#47681);
#13400=VERTEX_POINT('',#47682);
#13401=VERTEX_POINT('',#47694);
#13402=VERTEX_POINT('',#47707);
#13403=VERTEX_POINT('',#47708);
#13404=VERTEX_POINT('',#47732);
#13405=VERTEX_POINT('',#47733);
#13406=VERTEX_POINT('',#47757);
#13407=VERTEX_POINT('',#47758);
#13408=VERTEX_POINT('',#47781);
#13409=VERTEX_POINT('',#47782);
#13410=VERTEX_POINT('',#47805);
#13411=VERTEX_POINT('',#47806);
#13412=VERTEX_POINT('',#47830);
#13413=VERTEX_POINT('',#47831);
#13414=VERTEX_POINT('',#47855);
#13415=VERTEX_POINT('',#47856);
#13416=VERTEX_POINT('',#47879);
#13417=VERTEX_POINT('',#47880);
#13418=VERTEX_POINT('',#47904);
#13419=VERTEX_POINT('',#47905);
#13420=VERTEX_POINT('',#47929);
#13421=VERTEX_POINT('',#47930);
#13422=VERTEX_POINT('',#47953);
#13423=VERTEX_POINT('',#47954);
#13424=VERTEX_POINT('',#47977);
#13425=VERTEX_POINT('',#47978);
#13426=VERTEX_POINT('',#48002);
#13427=VERTEX_POINT('',#48003);
#13428=VERTEX_POINT('',#48027);
#13429=VERTEX_POINT('',#48028);
#13430=VERTEX_POINT('',#48051);
#13431=VERTEX_POINT('',#48052);
#13432=VERTEX_POINT('',#48076);
#13433=VERTEX_POINT('',#48077);
#13434=VERTEX_POINT('',#48101);
#13435=VERTEX_POINT('',#48102);
#13436=VERTEX_POINT('',#48125);
#13437=VERTEX_POINT('',#48126);
#13438=VERTEX_POINT('',#48672);
#13439=VERTEX_POINT('',#48789);
#13440=VERTEX_POINT('',#48903);
#13441=VERTEX_POINT('',#48906);
#13442=VERTEX_POINT('',#49545);
#13443=VERTEX_POINT('',#49663);
#13444=VERTEX_POINT('',#49664);
#13445=VERTEX_POINT('',#49668);
#13446=VERTEX_POINT('',#49672);
#13447=VERTEX_POINT('',#49676);
#13448=VERTEX_POINT('',#49680);
#13449=VERTEX_POINT('',#49684);
#13450=VERTEX_POINT('',#49687);
#13451=VERTEX_POINT('',#49695);
#13452=VERTEX_POINT('',#49697);
#13453=VERTEX_POINT('',#49701);
#13454=VERTEX_POINT('',#49705);
#13455=VERTEX_POINT('',#49709);
#13456=VERTEX_POINT('',#49711);
#13457=VERTEX_POINT('',#49722);
#13458=VERTEX_POINT('',#49729);
#13459=VERTEX_POINT('',#49730);
#13460=VERTEX_POINT('',#49732);
#13461=VERTEX_POINT('',#49743);
#13462=VERTEX_POINT('',#49756);
#13463=VERTEX_POINT('',#49757);
#13464=VERTEX_POINT('',#49804);
#13465=VERTEX_POINT('',#49805);
#13466=VERTEX_POINT('',#49852);
#13467=VERTEX_POINT('',#49853);
#13468=VERTEX_POINT('',#49900);
#13469=VERTEX_POINT('',#49901);
#13470=VERTEX_POINT('',#49954);
#13471=VERTEX_POINT('',#49955);
#13472=VERTEX_POINT('',#50002);
#13473=VERTEX_POINT('',#50003);
#13474=VERTEX_POINT('',#50050);
#13475=VERTEX_POINT('',#50051);
#13476=VERTEX_POINT('',#50104);
#13477=VERTEX_POINT('',#50105);
#13478=VERTEX_POINT('',#50152);
#13479=VERTEX_POINT('',#50153);
#13480=VERTEX_POINT('',#50200);
#13481=VERTEX_POINT('',#50201);
#13482=VERTEX_POINT('',#50248);
#13483=VERTEX_POINT('',#50249);
#13484=VERTEX_POINT('',#50302);
#13485=VERTEX_POINT('',#50303);
#13486=VERTEX_POINT('',#50350);
#13487=VERTEX_POINT('',#50351);
#13488=VERTEX_POINT('',#50398);
#13489=VERTEX_POINT('',#50399);
#13490=VERTEX_POINT('',#50452);
#13491=VERTEX_POINT('',#50453);
#13492=VERTEX_POINT('',#50500);
#13493=VERTEX_POINT('',#50501);
#13494=VERTEX_POINT('',#50548);
#13495=VERTEX_POINT('',#50549);
#13496=VERTEX_POINT('',#50596);
#13497=VERTEX_POINT('',#50597);
#13498=VERTEX_POINT('',#50650);
#13499=VERTEX_POINT('',#50651);
#13500=VERTEX_POINT('',#50698);
#13501=VERTEX_POINT('',#50699);
#13502=VERTEX_POINT('',#50701);
#13503=VERTEX_POINT('',#50708);
#13504=VERTEX_POINT('',#50709);
#13505=VERTEX_POINT('',#50721);
#13506=VERTEX_POINT('',#50734);
#13507=VERTEX_POINT('',#50735);
#13508=VERTEX_POINT('',#50759);
#13509=VERTEX_POINT('',#50760);
#13510=VERTEX_POINT('',#50784);
#13511=VERTEX_POINT('',#50785);
#13512=VERTEX_POINT('',#50808);
#13513=VERTEX_POINT('',#50809);
#13514=VERTEX_POINT('',#50832);
#13515=VERTEX_POINT('',#50833);
#13516=VERTEX_POINT('',#50857);
#13517=VERTEX_POINT('',#50858);
#13518=VERTEX_POINT('',#50882);
#13519=VERTEX_POINT('',#50883);
#13520=VERTEX_POINT('',#50906);
#13521=VERTEX_POINT('',#50907);
#13522=VERTEX_POINT('',#50931);
#13523=VERTEX_POINT('',#50932);
#13524=VERTEX_POINT('',#50956);
#13525=VERTEX_POINT('',#50957);
#13526=VERTEX_POINT('',#50980);
#13527=VERTEX_POINT('',#50981);
#13528=VERTEX_POINT('',#51004);
#13529=VERTEX_POINT('',#51005);
#13530=VERTEX_POINT('',#51029);
#13531=VERTEX_POINT('',#51030);
#13532=VERTEX_POINT('',#51054);
#13533=VERTEX_POINT('',#51055);
#13534=VERTEX_POINT('',#51078);
#13535=VERTEX_POINT('',#51079);
#13536=VERTEX_POINT('',#51103);
#13537=VERTEX_POINT('',#51104);
#13538=VERTEX_POINT('',#51128);
#13539=VERTEX_POINT('',#51129);
#13540=VERTEX_POINT('',#51152);
#13541=VERTEX_POINT('',#51153);
#13542=VERTEX_POINT('',#51699);
#13543=VERTEX_POINT('',#51816);
#13544=VERTEX_POINT('',#51930);
#13545=VERTEX_POINT('',#51933);
#13546=VERTEX_POINT('',#52572);
#13547=VERTEX_POINT('',#52690);
#13548=VERTEX_POINT('',#52691);
#13549=VERTEX_POINT('',#52693);
#13550=VERTEX_POINT('',#52695);
#13551=VERTEX_POINT('',#52699);
#13552=VERTEX_POINT('',#52703);
#13553=VERTEX_POINT('',#52709);
#13554=VERTEX_POINT('',#52710);
#13555=VERTEX_POINT('',#52712);
#13556=VERTEX_POINT('',#52714);
#13557=VERTEX_POINT('',#52718);
#13558=VERTEX_POINT('',#52722);
#13559=VERTEX_POINT('',#52728);
#13560=VERTEX_POINT('',#52729);
#13561=VERTEX_POINT('',#52731);
#13562=VERTEX_POINT('',#52733);
#13563=VERTEX_POINT('',#52737);
#13564=VERTEX_POINT('',#52741);
#13565=VERTEX_POINT('',#52747);
#13566=VERTEX_POINT('',#52748);
#13567=VERTEX_POINT('',#52750);
#13568=VERTEX_POINT('',#52752);
#13569=VERTEX_POINT('',#52756);
#13570=VERTEX_POINT('',#52760);
#13571=VERTEX_POINT('',#52766);
#13572=VERTEX_POINT('',#52767);
#13573=VERTEX_POINT('',#52769);
#13574=VERTEX_POINT('',#52771);
#13575=VERTEX_POINT('',#52775);
#13576=VERTEX_POINT('',#52779);
#13577=VERTEX_POINT('',#52785);
#13578=VERTEX_POINT('',#52786);
#13579=VERTEX_POINT('',#52788);
#13580=VERTEX_POINT('',#52790);
#13581=VERTEX_POINT('',#52794);
#13582=VERTEX_POINT('',#52798);
#13583=VERTEX_POINT('',#52804);
#13584=VERTEX_POINT('',#52805);
#13585=VERTEX_POINT('',#52807);
#13586=VERTEX_POINT('',#52809);
#13587=VERTEX_POINT('',#52813);
#13588=VERTEX_POINT('',#52817);
#13589=VERTEX_POINT('',#52823);
#13590=VERTEX_POINT('',#52824);
#13591=VERTEX_POINT('',#52826);
#13592=VERTEX_POINT('',#52828);
#13593=VERTEX_POINT('',#52832);
#13594=VERTEX_POINT('',#52836);
#13595=VERTEX_POINT('',#52842);
#13596=VERTEX_POINT('',#52843);
#13597=VERTEX_POINT('',#52845);
#13598=VERTEX_POINT('',#52847);
#13599=VERTEX_POINT('',#52851);
#13600=VERTEX_POINT('',#52855);
#13601=VERTEX_POINT('',#52861);
#13602=VERTEX_POINT('',#52862);
#13603=VERTEX_POINT('',#52864);
#13604=VERTEX_POINT('',#52866);
#13605=VERTEX_POINT('',#52870);
#13606=VERTEX_POINT('',#52874);
#13607=VERTEX_POINT('',#52880);
#13608=VERTEX_POINT('',#52881);
#13609=VERTEX_POINT('',#52883);
#13610=VERTEX_POINT('',#52885);
#13611=VERTEX_POINT('',#52889);
#13612=VERTEX_POINT('',#52893);
#13613=VERTEX_POINT('',#52899);
#13614=VERTEX_POINT('',#52900);
#13615=VERTEX_POINT('',#52902);
#13616=VERTEX_POINT('',#52904);
#13617=VERTEX_POINT('',#52908);
#13618=VERTEX_POINT('',#52912);
#13619=VERTEX_POINT('',#52918);
#13620=VERTEX_POINT('',#52919);
#13621=VERTEX_POINT('',#52921);
#13622=VERTEX_POINT('',#52923);
#13623=VERTEX_POINT('',#52927);
#13624=VERTEX_POINT('',#52931);
#13625=VERTEX_POINT('',#52937);
#13626=VERTEX_POINT('',#52938);
#13627=VERTEX_POINT('',#52940);
#13628=VERTEX_POINT('',#52942);
#13629=VERTEX_POINT('',#52946);
#13630=VERTEX_POINT('',#52950);
#13631=VERTEX_POINT('',#52956);
#13632=VERTEX_POINT('',#52957);
#13633=VERTEX_POINT('',#52959);
#13634=VERTEX_POINT('',#52961);
#13635=VERTEX_POINT('',#52965);
#13636=VERTEX_POINT('',#52969);
#13637=VERTEX_POINT('',#52975);
#13638=VERTEX_POINT('',#52976);
#13639=VERTEX_POINT('',#52978);
#13640=VERTEX_POINT('',#52980);
#13641=VERTEX_POINT('',#52984);
#13642=VERTEX_POINT('',#52988);
#13643=VERTEX_POINT('',#52994);
#13644=VERTEX_POINT('',#52995);
#13645=VERTEX_POINT('',#52997);
#13646=VERTEX_POINT('',#52999);
#13647=VERTEX_POINT('',#53003);
#13648=VERTEX_POINT('',#53007);
#13649=VERTEX_POINT('',#53013);
#13650=VERTEX_POINT('',#53014);
#13651=VERTEX_POINT('',#53016);
#13652=VERTEX_POINT('',#53018);
#13653=VERTEX_POINT('',#53022);
#13654=VERTEX_POINT('',#53024);
#13655=VERTEX_POINT('',#53028);
#13656=VERTEX_POINT('',#53032);
#13657=VERTEX_POINT('',#53036);
#13658=VERTEX_POINT('',#53037);
#13659=VERTEX_POINT('',#53039);
#13660=VERTEX_POINT('',#53041);
#13661=VERTEX_POINT('',#53045);
#13662=VERTEX_POINT('',#53049);
#13663=VERTEX_POINT('',#53055);
#13664=VERTEX_POINT('',#53056);
#13665=VERTEX_POINT('',#53058);
#13666=VERTEX_POINT('',#53060);
#13667=VERTEX_POINT('',#53064);
#13668=VERTEX_POINT('',#53068);
#13669=VERTEX_POINT('',#53074);
#13670=VERTEX_POINT('',#53075);
#13671=VERTEX_POINT('',#53077);
#13672=VERTEX_POINT('',#53079);
#13673=VERTEX_POINT('',#53083);
#13674=VERTEX_POINT('',#53087);
#13675=VERTEX_POINT('',#53093);
#13676=VERTEX_POINT('',#53094);
#13677=VERTEX_POINT('',#53096);
#13678=VERTEX_POINT('',#53098);
#13679=VERTEX_POINT('',#53102);
#13680=VERTEX_POINT('',#53106);
#13681=VERTEX_POINT('',#53112);
#13682=VERTEX_POINT('',#53113);
#13683=VERTEX_POINT('',#53115);
#13684=VERTEX_POINT('',#53117);
#13685=VERTEX_POINT('',#53121);
#13686=VERTEX_POINT('',#53125);
#13687=VERTEX_POINT('',#53131);
#13688=VERTEX_POINT('',#53132);
#13689=VERTEX_POINT('',#53134);
#13690=VERTEX_POINT('',#53136);
#13691=VERTEX_POINT('',#53140);
#13692=VERTEX_POINT('',#53144);
#13693=VERTEX_POINT('',#53150);
#13694=VERTEX_POINT('',#53151);
#13695=VERTEX_POINT('',#53153);
#13696=VERTEX_POINT('',#53155);
#13697=VERTEX_POINT('',#53159);
#13698=VERTEX_POINT('',#53163);
#13699=VERTEX_POINT('',#53169);
#13700=VERTEX_POINT('',#53170);
#13701=VERTEX_POINT('',#53172);
#13702=VERTEX_POINT('',#53174);
#13703=VERTEX_POINT('',#53178);
#13704=VERTEX_POINT('',#53182);
#13705=VERTEX_POINT('',#53188);
#13706=VERTEX_POINT('',#53189);
#13707=VERTEX_POINT('',#53191);
#13708=VERTEX_POINT('',#53193);
#13709=VERTEX_POINT('',#53197);
#13710=VERTEX_POINT('',#53201);
#13711=VERTEX_POINT('',#53207);
#13712=VERTEX_POINT('',#53208);
#13713=VERTEX_POINT('',#53210);
#13714=VERTEX_POINT('',#53212);
#13715=VERTEX_POINT('',#53216);
#13716=VERTEX_POINT('',#53220);
#13717=VERTEX_POINT('',#53226);
#13718=VERTEX_POINT('',#53227);
#13719=VERTEX_POINT('',#53229);
#13720=VERTEX_POINT('',#53231);
#13721=VERTEX_POINT('',#53235);
#13722=VERTEX_POINT('',#53239);
#13723=VERTEX_POINT('',#53245);
#13724=VERTEX_POINT('',#53246);
#13725=VERTEX_POINT('',#53248);
#13726=VERTEX_POINT('',#53250);
#13727=VERTEX_POINT('',#53254);
#13728=VERTEX_POINT('',#53258);
#13729=VERTEX_POINT('',#53264);
#13730=VERTEX_POINT('',#53265);
#13731=VERTEX_POINT('',#53267);
#13732=VERTEX_POINT('',#53269);
#13733=VERTEX_POINT('',#53273);
#13734=VERTEX_POINT('',#53277);
#13735=VERTEX_POINT('',#53283);
#13736=VERTEX_POINT('',#53284);
#13737=VERTEX_POINT('',#53286);
#13738=VERTEX_POINT('',#53288);
#13739=VERTEX_POINT('',#53292);
#13740=VERTEX_POINT('',#53296);
#13741=VERTEX_POINT('',#53302);
#13742=VERTEX_POINT('',#53303);
#13743=VERTEX_POINT('',#53305);
#13744=VERTEX_POINT('',#53307);
#13745=VERTEX_POINT('',#53311);
#13746=VERTEX_POINT('',#53315);
#13747=VERTEX_POINT('',#53321);
#13748=VERTEX_POINT('',#53322);
#13749=VERTEX_POINT('',#53324);
#13750=VERTEX_POINT('',#53326);
#13751=VERTEX_POINT('',#53330);
#13752=VERTEX_POINT('',#53334);
#13753=VERTEX_POINT('',#53340);
#13754=VERTEX_POINT('',#53341);
#13755=VERTEX_POINT('',#53343);
#13756=VERTEX_POINT('',#53345);
#13757=VERTEX_POINT('',#53349);
#13758=VERTEX_POINT('',#53353);
#13759=VERTEX_POINT('',#53359);
#13760=VERTEX_POINT('',#53360);
#13761=VERTEX_POINT('',#53362);
#13762=VERTEX_POINT('',#53364);
#13763=VERTEX_POINT('',#53368);
#13764=VERTEX_POINT('',#53372);
#13765=VERTEX_POINT('',#53378);
#13766=VERTEX_POINT('',#53379);
#13767=VERTEX_POINT('',#53381);
#13768=VERTEX_POINT('',#53383);
#13769=VERTEX_POINT('',#53387);
#13770=VERTEX_POINT('',#53389);
#13771=VERTEX_POINT('',#53393);
#13772=VERTEX_POINT('',#53395);
#13773=VERTEX_POINT('',#53399);
#13774=VERTEX_POINT('',#53401);
#13775=VERTEX_POINT('',#53405);
#13776=VERTEX_POINT('',#53407);
#13777=VERTEX_POINT('',#53415);
#13778=VERTEX_POINT('',#53422);
#13779=VERTEX_POINT('',#53425);
#13780=VERTEX_POINT('',#53430);
#13781=VERTEX_POINT('',#53436);
#13782=VERTEX_POINT('',#53437);
#13783=VERTEX_POINT('',#53439);
#13784=VERTEX_POINT('',#53443);
#13785=VERTEX_POINT('',#53444);
#13786=VERTEX_POINT('',#53449);
#13787=VERTEX_POINT('',#53450);
#13788=VERTEX_POINT('',#53452);
#13789=VERTEX_POINT('',#53456);
#13790=VERTEX_POINT('',#53457);
#13791=VERTEX_POINT('',#53465);
#13792=VERTEX_POINT('',#53466);
#13793=VERTEX_POINT('',#53468);
#13794=VERTEX_POINT('',#53472);
#13795=VERTEX_POINT('',#53473);
#13796=VERTEX_POINT('',#53478);
#13797=VERTEX_POINT('',#53479);
#13798=VERTEX_POINT('',#53481);
#13799=VERTEX_POINT('',#53485);
#13800=VERTEX_POINT('',#53486);
#13801=VERTEX_POINT('',#53494);
#13802=VERTEX_POINT('',#53495);
#13803=VERTEX_POINT('',#53497);
#13804=VERTEX_POINT('',#53501);
#13805=VERTEX_POINT('',#53502);
#13806=VERTEX_POINT('',#53507);
#13807=VERTEX_POINT('',#53508);
#13808=VERTEX_POINT('',#53510);
#13809=VERTEX_POINT('',#53514);
#13810=VERTEX_POINT('',#53515);
#13811=VERTEX_POINT('',#53538);
#13812=VERTEX_POINT('',#53539);
#13813=VERTEX_POINT('',#53541);
#13814=VERTEX_POINT('',#53543);
#13815=VERTEX_POINT('',#53545);
#13816=VERTEX_POINT('',#53547);
#13817=VERTEX_POINT('',#53551);
#13818=VERTEX_POINT('',#53553);
#13819=VERTEX_POINT('',#53557);
#13820=VERTEX_POINT('',#53561);
#13821=VERTEX_POINT('',#53563);
#13822=VERTEX_POINT('',#53567);
#13823=VERTEX_POINT('',#53575);
#13824=VERTEX_POINT('',#53577);
#13825=VERTEX_POINT('',#53581);
#13826=VERTEX_POINT('',#53585);
#13827=VERTEX_POINT('',#53589);
#13828=VERTEX_POINT('',#53593);
#13829=VERTEX_POINT('',#53603);
#13830=VERTEX_POINT('',#53609);
#13831=VERTEX_POINT('',#53612);
#13832=VERTEX_POINT('',#53619);
#13833=VERTEX_POINT('',#53620);
#13834=VERTEX_POINT('',#53622);
#13835=VERTEX_POINT('',#53633);
#13836=VERTEX_POINT('',#53643);
#13837=VERTEX_POINT('',#53644);
#13838=VERTEX_POINT('',#53691);
#13839=VERTEX_POINT('',#53692);
#13840=VERTEX_POINT('',#53739);
#13841=VERTEX_POINT('',#53740);
#13842=VERTEX_POINT('',#53793);
#13843=VERTEX_POINT('',#53794);
#13844=VERTEX_POINT('',#53841);
#13845=VERTEX_POINT('',#53842);
#13846=VERTEX_POINT('',#53889);
#13847=VERTEX_POINT('',#53890);
#13848=VERTEX_POINT('',#53937);
#13849=VERTEX_POINT('',#53938);
#13850=VERTEX_POINT('',#53991);
#13851=VERTEX_POINT('',#53992);
#13852=VERTEX_POINT('',#54039);
#13853=VERTEX_POINT('',#54040);
#13854=VERTEX_POINT('',#54087);
#13855=VERTEX_POINT('',#54088);
#13856=VERTEX_POINT('',#54141);
#13857=VERTEX_POINT('',#54142);
#13858=VERTEX_POINT('',#54189);
#13859=VERTEX_POINT('',#54190);
#13860=VERTEX_POINT('',#54192);
#13861=VERTEX_POINT('',#54236);
#13862=VERTEX_POINT('',#54237);
#13863=VERTEX_POINT('',#54239);
#13864=VERTEX_POINT('',#54247);
#13865=VERTEX_POINT('',#54256);
#13866=VERTEX_POINT('',#54257);
#13867=VERTEX_POINT('',#54280);
#13868=VERTEX_POINT('',#54281);
#13869=VERTEX_POINT('',#54305);
#13870=VERTEX_POINT('',#54306);
#13871=VERTEX_POINT('',#54330);
#13872=VERTEX_POINT('',#54331);
#13873=VERTEX_POINT('',#54354);
#13874=VERTEX_POINT('',#54355);
#13875=VERTEX_POINT('',#54379);
#13876=VERTEX_POINT('',#54380);
#13877=VERTEX_POINT('',#54404);
#13878=VERTEX_POINT('',#54405);
#13879=VERTEX_POINT('',#54428);
#13880=VERTEX_POINT('',#54429);
#13881=VERTEX_POINT('',#54452);
#13882=VERTEX_POINT('',#54453);
#13883=VERTEX_POINT('',#54477);
#13884=VERTEX_POINT('',#54478);
#13885=VERTEX_POINT('',#54502);
#13886=VERTEX_POINT('',#54503);
#13887=VERTEX_POINT('',#54853);
#13888=VERTEX_POINT('',#54943);
#13889=VERTEX_POINT('',#55039);
#13890=VERTEX_POINT('',#55042);
#13891=VERTEX_POINT('',#55552);
#13892=VERTEX_POINT('',#55553);
#13893=VERTEX_POINT('',#55560);
#13894=VERTEX_POINT('',#55562);
#13895=VERTEX_POINT('',#55566);
#13896=VERTEX_POINT('',#55573);
#13897=VERTEX_POINT('',#55577);
#13898=VERTEX_POINT('',#55584);
#13899=VERTEX_POINT('',#55588);
#13900=VERTEX_POINT('',#55595);
#13901=VERTEX_POINT('',#55599);
#13902=VERTEX_POINT('',#55606);
#13903=VERTEX_POINT('',#55619);
#13904=VERTEX_POINT('',#55626);
#13905=EDGE_CURVE('',#11462,#11463,#10978,.F.);
#13906=EDGE_CURVE('',#11463,#11464,#10119,.T.);
#13907=EDGE_CURVE('',#11464,#11465,#10120,.T.);
#13908=EDGE_CURVE('',#11465,#11465,#10121,.T.);
#13909=EDGE_CURVE('',#11464,#11466,#10122,.T.);
#13910=EDGE_CURVE('',#11466,#11467,#10979,.F.);
#13911=EDGE_CURVE('',#11462,#11467,#10123,.T.);
#13912=EDGE_CURVE('',#11463,#11468,#1758,.T.);
#13913=EDGE_CURVE('',#11469,#11468,#10124,.T.);
#13914=EDGE_CURVE('',#11470,#11469,#10125,.T.);
#13915=EDGE_CURVE('',#11470,#11471,#10980,.T.);
#13916=EDGE_CURVE('',#11471,#11472,#1759,.T.);
#13917=EDGE_CURVE('',#11472,#11473,#10981,.T.);
#13918=EDGE_CURVE('',#11473,#11474,#10126,.T.);
#13919=EDGE_CURVE('',#11474,#11475,#10982,.T.);
#13920=EDGE_CURVE('',#11475,#11476,#1760,.T.);
#13921=EDGE_CURVE('',#11476,#11477,#10983,.T.);
#13922=EDGE_CURVE('',#11478,#11477,#10127,.T.);
#13923=EDGE_CURVE('',#11479,#11478,#10984,.F.);
#13924=EDGE_CURVE('',#11479,#11480,#1761,.T.);
#13925=EDGE_CURVE('',#11466,#11480,#10985,.F.);
#13926=EDGE_CURVE('',#11481,#11481,#10128,.T.);
#13927=EDGE_CURVE('',#11482,#11482,#10129,.T.);
#13928=EDGE_CURVE('',#11483,#11483,#10130,.T.);
#13929=EDGE_CURVE('',#11484,#11484,#10131,.T.);
#13930=EDGE_CURVE('',#11485,#11485,#10132,.T.);
#13931=EDGE_CURVE('',#11469,#11486,#10133,.T.);
#13932=EDGE_CURVE('',#11486,#11486,#10134,.T.);
#13933=EDGE_CURVE('',#11468,#11478,#10135,.T.);
#13934=EDGE_CURVE('',#11477,#11470,#10136,.T.);
#13935=EDGE_CURVE('',#11487,#11487,#10137,.T.);
#13936=EDGE_CURVE('',#11488,#11488,#10138,.T.);
#13937=EDGE_CURVE('',#11489,#11489,#10139,.T.);
#13938=EDGE_CURVE('',#11490,#11490,#10140,.T.);
#13939=EDGE_CURVE('',#11491,#11491,#10141,.T.);
#13940=EDGE_CURVE('',#11492,#11492,#10142,.T.);
#13941=EDGE_CURVE('',#11493,#11493,#10143,.T.);
#13942=EDGE_CURVE('',#11494,#11494,#10144,.T.);
#13943=EDGE_CURVE('',#11495,#11495,#10145,.T.);
#13944=EDGE_CURVE('',#11496,#11497,#10146,.T.);
#13945=EDGE_CURVE('',#11497,#11498,#1762,.T.);
#13946=EDGE_CURVE('',#11498,#11499,#10147,.T.);
#13947=EDGE_CURVE('',#11499,#11496,#1763,.T.);
#13948=EDGE_CURVE('',#11500,#11501,#10148,.T.);
#13949=EDGE_CURVE('',#11501,#11499,#10149,.T.);
#13950=EDGE_CURVE('',#11498,#11500,#10150,.T.);
#13951=EDGE_CURVE('',#11502,#11503,#10151,.T.);
#13952=EDGE_CURVE('',#11503,#11501,#1764,.T.);
#13953=EDGE_CURVE('',#11500,#11502,#1765,.T.);
#13954=EDGE_CURVE('',#11504,#11505,#10152,.T.);
#13955=EDGE_CURVE('',#11505,#11503,#10153,.T.);
#13956=EDGE_CURVE('',#11502,#11504,#10154,.T.);
#13957=EDGE_CURVE('',#11506,#11507,#10155,.T.);
#13958=EDGE_CURVE('',#11507,#11505,#1766,.T.);
#13959=EDGE_CURVE('',#11504,#11506,#1767,.T.);
#13960=EDGE_CURVE('',#11508,#11509,#10156,.T.);
#13961=EDGE_CURVE('',#11509,#11507,#10157,.T.);
#13962=EDGE_CURVE('',#11506,#11508,#10158,.T.);
#13963=EDGE_CURVE('',#11510,#11511,#10159,.T.);
#13964=EDGE_CURVE('',#11511,#11509,#1768,.T.);
#13965=EDGE_CURVE('',#11508,#11510,#1769,.T.);
#13966=EDGE_CURVE('',#11496,#11511,#10160,.T.);
#13967=EDGE_CURVE('',#11510,#11497,#10161,.T.);
#13968=EDGE_CURVE('',#11509,#11512,#1770,.T.);
#13969=EDGE_CURVE('',#11513,#11512,#10162,.T.);
#13970=EDGE_CURVE('',#11507,#11513,#1771,.T.);
#13971=EDGE_CURVE('',#11511,#11514,#1772,.T.);
#13972=EDGE_CURVE('',#11512,#11514,#1773,.T.);
#13973=EDGE_CURVE('',#11496,#11515,#1774,.T.);
#13974=EDGE_CURVE('',#11514,#11515,#10163,.T.);
#13975=EDGE_CURVE('',#11499,#11516,#1775,.T.);
#13976=EDGE_CURVE('',#11515,#11516,#1776,.T.);
#13977=EDGE_CURVE('',#11517,#11517,#10164,.T.);
#13978=EDGE_CURVE('',#11518,#11518,#10165,.T.);
#13979=EDGE_CURVE('',#11519,#11520,#10166,.T.);
#13980=EDGE_CURVE('',#11520,#11521,#1777,.T.);
#13981=EDGE_CURVE('',#11521,#11522,#10167,.T.);
#13982=EDGE_CURVE('',#11522,#11519,#1778,.T.);
#13983=EDGE_CURVE('',#11523,#11524,#10168,.T.);
#13984=EDGE_CURVE('',#11524,#11522,#10169,.T.);
#13985=EDGE_CURVE('',#11521,#11523,#10170,.T.);
#13986=EDGE_CURVE('',#11513,#11525,#10171,.T.);
#13987=EDGE_CURVE('',#11525,#11524,#1779,.T.);
#13988=EDGE_CURVE('',#11523,#11513,#1780,.T.);
#13989=EDGE_CURVE('',#11512,#11526,#10172,.T.);
#13990=EDGE_CURVE('',#11526,#11525,#10173,.T.);
#13991=EDGE_CURVE('',#11514,#11527,#10174,.T.);
#13992=EDGE_CURVE('',#11527,#11526,#1781,.T.);
#13993=EDGE_CURVE('',#11515,#11528,#10175,.T.);
#13994=EDGE_CURVE('',#11528,#11527,#10176,.T.);
#13995=EDGE_CURVE('',#11516,#11529,#10177,.T.);
#13996=EDGE_CURVE('',#11529,#11528,#1782,.T.);
#13997=EDGE_CURVE('',#11519,#11529,#10178,.T.);
#13998=EDGE_CURVE('',#11516,#11520,#10179,.T.);
#13999=EDGE_CURVE('',#11505,#11523,#1783,.T.);
#14000=EDGE_CURVE('',#11503,#11521,#1784,.T.);
#14001=EDGE_CURVE('',#11501,#11520,#1785,.T.);
#14002=EDGE_CURVE('',#11530,#11531,#10180,.T.);
#14003=EDGE_CURVE('',#11532,#11530,#1786,.T.);
#14004=EDGE_CURVE('',#11533,#11532,#10181,.T.);
#14005=EDGE_CURVE('',#11534,#11533,#1787,.T.);
#14006=EDGE_CURVE('',#11535,#11534,#10182,.T.);
#14007=EDGE_CURVE('',#11536,#11535,#1788,.T.);
#14008=EDGE_CURVE('',#11537,#11536,#10183,.T.);
#14009=EDGE_CURVE('',#11531,#11537,#1789,.T.);
#14010=EDGE_CURVE('',#11538,#11538,#10184,.T.);
#14011=EDGE_CURVE('',#11539,#11539,#10185,.T.);
#14012=EDGE_CURVE('',#11540,#11541,#10186,.T.);
#14013=EDGE_CURVE('',#11541,#11542,#1790,.T.);
#14014=EDGE_CURVE('',#11542,#11543,#10187,.T.);
#14015=EDGE_CURVE('',#11543,#11540,#1791,.T.);
#14016=EDGE_CURVE('',#11544,#11545,#10188,.T.);
#14017=EDGE_CURVE('',#11545,#11543,#10189,.T.);
#14018=EDGE_CURVE('',#11542,#11544,#10190,.T.);
#14019=EDGE_CURVE('',#11546,#11547,#10191,.T.);
#14020=EDGE_CURVE('',#11547,#11545,#1792,.T.);
#14021=EDGE_CURVE('',#11544,#11546,#1793,.T.);
#14022=EDGE_CURVE('',#11548,#11549,#10192,.T.);
#14023=EDGE_CURVE('',#11549,#11547,#10193,.T.);
#14024=EDGE_CURVE('',#11546,#11548,#10194,.T.);
#14025=EDGE_CURVE('',#11550,#11551,#10195,.T.);
#14026=EDGE_CURVE('',#11551,#11549,#1794,.T.);
#14027=EDGE_CURVE('',#11548,#11550,#1795,.T.);
#14028=EDGE_CURVE('',#11552,#11553,#10196,.T.);
#14029=EDGE_CURVE('',#11553,#11551,#10197,.T.);
#14030=EDGE_CURVE('',#11550,#11552,#10198,.T.);
#14031=EDGE_CURVE('',#11554,#11555,#10199,.T.);
#14032=EDGE_CURVE('',#11555,#11553,#1796,.T.);
#14033=EDGE_CURVE('',#11552,#11554,#1797,.T.);
#14034=EDGE_CURVE('',#11540,#11555,#10200,.T.);
#14035=EDGE_CURVE('',#11554,#11541,#10201,.T.);
#14036=EDGE_CURVE('',#11556,#11546,#1798,.T.);
#14037=EDGE_CURVE('',#11557,#11556,#10202,.T.);
#14038=EDGE_CURVE('',#11557,#11548,#1799,.T.);
#14039=EDGE_CURVE('',#11558,#11544,#1800,.T.);
#14040=EDGE_CURVE('',#11556,#11558,#1801,.T.);
#14041=EDGE_CURVE('',#11559,#11542,#1802,.T.);
#14042=EDGE_CURVE('',#11558,#11559,#10203,.T.);
#14043=EDGE_CURVE('',#11560,#11541,#1803,.T.);
#14044=EDGE_CURVE('',#11559,#11560,#1804,.T.);
#14045=EDGE_CURVE('',#11561,#11561,#10204,.T.);
#14046=EDGE_CURVE('',#11562,#11563,#10205,.T.);
#14047=EDGE_CURVE('',#11563,#11564,#1805,.T.);
#14048=EDGE_CURVE('',#11564,#11565,#10206,.T.);
#14049=EDGE_CURVE('',#11565,#11562,#1806,.T.);
#14050=EDGE_CURVE('',#11566,#11567,#10207,.T.);
#14051=EDGE_CURVE('',#11567,#11565,#10208,.T.);
#14052=EDGE_CURVE('',#11564,#11566,#10209,.T.);
#14053=EDGE_CURVE('',#11568,#11569,#10210,.T.);
#14054=EDGE_CURVE('',#11569,#11567,#1807,.T.);
#14055=EDGE_CURVE('',#11566,#11568,#1808,.T.);
#14056=EDGE_CURVE('',#11570,#11571,#10211,.T.);
#14057=EDGE_CURVE('',#11571,#11569,#10212,.T.);
#14058=EDGE_CURVE('',#11568,#11570,#10213,.T.);
#14059=EDGE_CURVE('',#11572,#11573,#10214,.T.);
#14060=EDGE_CURVE('',#11573,#11571,#1809,.T.);
#14061=EDGE_CURVE('',#11570,#11572,#1810,.T.);
#14062=EDGE_CURVE('',#11574,#11575,#10215,.T.);
#14063=EDGE_CURVE('',#11575,#11573,#10216,.T.);
#14064=EDGE_CURVE('',#11572,#11574,#10217,.T.);
#14065=EDGE_CURVE('',#11576,#11577,#10218,.T.);
#14066=EDGE_CURVE('',#11577,#11575,#1811,.T.);
#14067=EDGE_CURVE('',#11574,#11576,#1812,.T.);
#14068=EDGE_CURVE('',#11562,#11577,#10219,.T.);
#14069=EDGE_CURVE('',#11576,#11563,#10220,.T.);
#14070=EDGE_CURVE('',#11578,#11568,#1813,.T.);
#14071=EDGE_CURVE('',#11579,#11578,#10221,.T.);
#14072=EDGE_CURVE('',#11579,#11570,#1814,.T.);
#14073=EDGE_CURVE('',#11580,#11566,#1815,.T.);
#14074=EDGE_CURVE('',#11578,#11580,#1816,.T.);
#14075=EDGE_CURVE('',#11581,#11564,#1817,.T.);
#14076=EDGE_CURVE('',#11580,#11581,#10222,.T.);
#14077=EDGE_CURVE('',#11582,#11563,#1818,.T.);
#14078=EDGE_CURVE('',#11581,#11582,#1819,.T.);
#14079=EDGE_CURVE('',#11583,#11583,#10223,.T.);
#14080=EDGE_CURVE('',#11495,#11584,#10224,.T.);
#14081=EDGE_CURVE('',#11584,#11584,#10225,.T.);
#14082=EDGE_CURVE('',#11584,#11585,#1820,.T.);
#14083=EDGE_CURVE('',#11585,#11586,#10226,.T.);
#14084=EDGE_CURVE('',#11587,#11586,#1821,.T.);
#14085=EDGE_CURVE('',#11588,#11587,#10986,.F.);
#14086=EDGE_CURVE('',#11588,#11589,#10227,.T.);
#14087=EDGE_CURVE('',#11590,#11589,#10987,.F.);
#14088=EDGE_CURVE('',#11590,#11591,#1822,.T.);
#14089=EDGE_CURVE('',#11591,#11585,#10228,.T.);
#14090=EDGE_CURVE('',#11592,#11592,#10229,.T.);
#14091=EDGE_CURVE('',#11592,#11593,#10230,.T.);
#14092=EDGE_CURVE('',#11593,#11593,#10231,.T.);
#14093=EDGE_CURVE('',#11589,#11594,#1823,.T.);
#14094=EDGE_CURVE('',#11595,#11588,#1824,.T.);
#14095=EDGE_CURVE('',#11594,#11595,#10232,.T.);
#14096=EDGE_CURVE('',#11593,#11596,#1825,.T.);
#14097=EDGE_CURVE('',#11596,#11596,#10233,.T.);
#14098=EDGE_CURVE('',#11597,#11590,#1826,.T.);
#14099=EDGE_CURVE('',#11594,#11597,#10988,.T.);
#14100=EDGE_CURVE('',#11598,#11597,#10234,.T.);
#14101=EDGE_CURVE('',#11595,#11598,#10989,.T.);
#14102=EDGE_CURVE('',#11587,#11598,#1827,.T.);
#14103=EDGE_CURVE('',#11597,#11599,#1828,.T.);
#14104=EDGE_CURVE('',#11599,#11591,#1829,.T.);
#14105=EDGE_CURVE('',#11598,#11600,#1830,.T.);
#14106=EDGE_CURVE('',#11600,#11599,#10235,.T.);
#14107=EDGE_CURVE('',#11586,#11600,#1831,.T.);
#14108=EDGE_CURVE('',#11601,#11602,#10236,.T.);
#14109=EDGE_CURVE('',#11602,#11603,#10237,.T.);
#14110=EDGE_CURVE('',#11603,#11604,#10238,.T.);
#14111=EDGE_CURVE('',#11604,#11605,#10239,.T.);
#14112=EDGE_CURVE('',#11605,#11601,#10240,.T.);
#14113=EDGE_CURVE('',#11606,#11607,#10241,.T.);
#14114=EDGE_CURVE('',#11607,#11605,#10990,.T.);
#14115=EDGE_CURVE('',#11604,#11606,#10991,.T.);
#14116=EDGE_CURVE('',#11608,#11609,#10242,.T.);
#14117=EDGE_CURVE('',#11609,#11607,#10243,.T.);
#14118=EDGE_CURVE('',#11606,#11608,#10244,.T.);
#14119=EDGE_CURVE('',#11601,#11609,#10992,.T.);
#14120=EDGE_CURVE('',#11608,#11602,#10993,.T.);
#14121=EDGE_CURVE('',#11601,#11610,#1832,.T.);
#14122=EDGE_CURVE('',#11611,#11610,#10245,.T.);
#14123=EDGE_CURVE('',#11612,#11611,#1833,.T.);
#14124=EDGE_CURVE('',#11612,#11613,#10246,.T.);
#14125=EDGE_CURVE('',#11613,#11609,#1834,.T.);
#14126=EDGE_CURVE('',#11605,#11614,#1835,.T.);
#14127=EDGE_CURVE('',#11610,#11614,#1836,.T.);
#14128=EDGE_CURVE('',#11603,#11615,#1837,.T.);
#14129=EDGE_CURVE('',#11615,#11615,#10247,.T.);
#14130=EDGE_CURVE('',#11480,#11616,#1838,.T.);
#14131=EDGE_CURVE('',#11616,#11617,#10248,.T.);
#14132=EDGE_CURVE('',#11617,#11467,#1839,.T.);
#14133=EDGE_CURVE('',#11618,#11619,#10249,.T.);
#14134=EDGE_CURVE('',#11619,#11620,#1840,.T.);
#14135=EDGE_CURVE('',#11620,#11621,#10250,.T.);
#14136=EDGE_CURVE('',#11621,#11618,#1841,.T.);
#14137=EDGE_CURVE('',#11622,#11623,#10251,.T.);
#14138=EDGE_CURVE('',#11623,#11621,#10252,.T.);
#14139=EDGE_CURVE('',#11620,#11622,#10253,.T.);
#14140=EDGE_CURVE('',#11478,#11623,#1842,.T.);
#14141=EDGE_CURVE('',#11622,#11479,#1843,.T.);
#14142=EDGE_CURVE('',#11618,#11617,#10254,.T.);
#14143=EDGE_CURVE('',#11616,#11619,#10255,.T.);
#14144=EDGE_CURVE('',#11623,#11624,#1844,.T.);
#14145=EDGE_CURVE('',#11625,#11624,#10256,.T.);
#14146=EDGE_CURVE('',#11626,#11625,#1845,.T.);
#14147=EDGE_CURVE('',#11627,#11626,#10994,.T.);
#14148=EDGE_CURVE('',#11621,#11627,#1846,.T.);
#14149=EDGE_CURVE('',#11468,#11612,#1847,.T.);
#14150=EDGE_CURVE('',#11624,#11611,#1848,.T.);
#14151=EDGE_CURVE('',#11628,#11629,#10257,.T.);
#14152=EDGE_CURVE('',#11629,#11625,#1849,.T.);
#14153=EDGE_CURVE('',#11625,#11630,#10258,.T.);
#14154=EDGE_CURVE('',#11630,#11628,#1850,.T.);
#14155=EDGE_CURVE('',#11624,#11631,#10259,.T.);
#14156=EDGE_CURVE('',#11631,#11630,#10260,.T.);
#14157=EDGE_CURVE('',#11611,#11632,#10261,.T.);
#14158=EDGE_CURVE('',#11632,#11631,#1851,.T.);
#14159=EDGE_CURVE('',#11610,#11633,#10262,.T.);
#14160=EDGE_CURVE('',#11633,#11632,#10263,.T.);
#14161=EDGE_CURVE('',#11614,#11634,#10264,.T.);
#14162=EDGE_CURVE('',#11634,#11633,#1852,.T.);
#14163=EDGE_CURVE('',#11635,#11636,#10265,.T.);
#14164=EDGE_CURVE('',#11636,#11634,#10266,.T.);
#14165=EDGE_CURVE('',#11614,#11635,#10267,.T.);
#14166=EDGE_CURVE('',#11637,#11638,#10268,.T.);
#14167=EDGE_CURVE('',#11638,#11636,#1853,.T.);
#14168=EDGE_CURVE('',#11635,#11637,#1854,.T.);
#14169=EDGE_CURVE('',#11628,#11638,#10269,.T.);
#14170=EDGE_CURVE('',#11637,#11629,#10270,.T.);
#14171=EDGE_CURVE('',#11639,#11629,#1855,.T.);
#14172=EDGE_CURVE('',#11626,#11639,#10271,.T.);
#14173=EDGE_CURVE('',#11560,#11640,#10272,.T.);
#14174=EDGE_CURVE('',#11640,#11641,#1856,.T.);
#14175=EDGE_CURVE('',#11641,#11642,#10273,.T.);
#14176=EDGE_CURVE('',#11642,#11557,#1857,.T.);
#14177=EDGE_CURVE('',#11582,#11643,#10274,.T.);
#14178=EDGE_CURVE('',#11643,#11644,#1858,.T.);
#14179=EDGE_CURVE('',#11644,#11645,#10275,.T.);
#14180=EDGE_CURVE('',#11645,#11579,#1859,.T.);
#14181=EDGE_CURVE('',#11646,#11646,#10276,.T.);
#14182=EDGE_CURVE('',#11639,#11647,#10277,.T.);
#14183=EDGE_CURVE('',#11647,#11648,#10278,.T.);
#14184=EDGE_CURVE('',#11648,#11649,#10279,.T.);
#14185=EDGE_CURVE('',#11649,#11626,#10280,.T.);
#14186=EDGE_CURVE('',#11650,#11627,#10281,.T.);
#14187=EDGE_CURVE('',#11649,#11650,#10995,.T.);
#14188=EDGE_CURVE('',#11651,#11652,#10282,.T.);
#14189=EDGE_CURVE('',#11652,#11627,#10283,.T.);
#14190=EDGE_CURVE('',#11650,#11651,#10284,.T.);
#14191=EDGE_CURVE('',#11639,#11652,#10996,.T.);
#14192=EDGE_CURVE('',#11651,#11647,#10997,.T.);
#14193=EDGE_CURVE('',#11618,#11652,#1860,.T.);
#14194=EDGE_CURVE('',#11617,#11637,#1861,.T.);
#14195=EDGE_CURVE('',#11648,#11653,#1862,.T.);
#14196=EDGE_CURVE('',#11653,#11653,#10285,.T.);
#14197=EDGE_CURVE('',#11539,#11518,#1863,.T.);
#14198=EDGE_CURVE('',#11538,#11517,#1864,.T.);
#14199=EDGE_CURVE('',#11561,#11654,#1865,.T.);
#14200=EDGE_CURVE('',#11654,#11654,#10286,.T.);
#14201=EDGE_CURVE('',#11583,#11655,#1866,.T.);
#14202=EDGE_CURVE('',#11655,#11655,#10287,.T.);
#14203=EDGE_CURVE('',#11646,#11656,#1867,.T.);
#14204=EDGE_CURVE('',#11656,#11656,#10288,.T.);
#14205=EDGE_CURVE('',#11613,#11657,#1868,.T.);
#14206=EDGE_CURVE('',#11657,#11607,#1869,.T.);
#14207=EDGE_CURVE('',#11481,#11658,#1870,.T.);
#14208=EDGE_CURVE('',#11658,#11658,#10289,.T.);
#14209=EDGE_CURVE('',#11482,#11659,#1871,.T.);
#14210=EDGE_CURVE('',#11659,#11659,#10290,.T.);
#14211=EDGE_CURVE('',#11483,#11660,#1872,.T.);
#14212=EDGE_CURVE('',#11660,#11660,#10291,.T.);
#14213=EDGE_CURVE('',#11484,#11661,#1873,.T.);
#14214=EDGE_CURVE('',#11661,#11661,#10292,.T.);
#14215=EDGE_CURVE('',#11487,#11662,#1874,.T.);
#14216=EDGE_CURVE('',#11662,#11662,#10293,.T.);
#14217=EDGE_CURVE('',#11488,#11663,#1875,.T.);
#14218=EDGE_CURVE('',#11663,#11663,#10294,.T.);
#14219=EDGE_CURVE('',#11489,#11664,#1876,.T.);
#14220=EDGE_CURVE('',#11664,#11664,#10295,.T.);
#14221=EDGE_CURVE('',#11490,#11665,#1877,.T.);
#14222=EDGE_CURVE('',#11665,#11665,#10296,.T.);
#14223=EDGE_CURVE('',#11491,#11666,#1878,.T.);
#14224=EDGE_CURVE('',#11666,#11666,#10297,.T.);
#14225=EDGE_CURVE('',#11492,#11667,#1879,.T.);
#14226=EDGE_CURVE('',#11667,#11667,#10298,.T.);
#14227=EDGE_CURVE('',#11493,#11668,#1880,.T.);
#14228=EDGE_CURVE('',#11668,#11668,#10299,.T.);
#14229=EDGE_CURVE('',#11494,#11669,#1881,.T.);
#14230=EDGE_CURVE('',#11669,#11669,#10300,.T.);
#14231=EDGE_CURVE('',#11670,#11670,#10301,.T.);
#14232=EDGE_CURVE('',#11670,#11485,#1882,.T.);
#14233=EDGE_CURVE('',#11643,#11576,#1883,.T.);
#14234=EDGE_CURVE('',#11644,#11574,#1884,.T.);
#14235=EDGE_CURVE('',#11645,#11572,#1885,.T.);
#14236=EDGE_CURVE('',#11640,#11554,#1886,.T.);
#14237=EDGE_CURVE('',#11641,#11552,#1887,.T.);
#14238=EDGE_CURVE('',#11642,#11550,#1888,.T.);
#14239=EDGE_CURVE('',#11530,#11470,#1889,.T.);
#14240=EDGE_CURVE('',#11531,#11471,#1890,.T.);
#14241=EDGE_CURVE('',#11532,#11477,#1891,.T.);
#14242=EDGE_CURVE('',#11533,#11476,#1892,.T.);
#14243=EDGE_CURVE('',#11534,#11475,#1893,.T.);
#14244=EDGE_CURVE('',#11535,#11474,#1894,.T.);
#14245=EDGE_CURVE('',#11536,#11473,#1895,.T.);
#14246=EDGE_CURVE('',#11537,#11472,#1896,.T.);
#14247=EDGE_CURVE('',#11462,#11671,#1897,.T.);
#14248=EDGE_CURVE('',#11657,#11671,#10302,.T.);
#14249=EDGE_CURVE('',#11671,#11635,#1898,.T.);
#14250=EDGE_CURVE('',#11672,#11673,#10998,.T.);
#14251=EDGE_CURVE('',#11674,#11673,#10999,.T.);
#14252=EDGE_CURVE('',#11674,#11675,#11000,.T.);
#14253=EDGE_CURVE('',#11675,#11672,#1899,.T.);
#14254=EDGE_CURVE('',#11673,#11676,#11001,.T.);
#14255=EDGE_CURVE('',#11676,#11677,#1900,.T.);
#14256=EDGE_CURVE('',#11677,#11674,#11002,.T.);
#14257=EDGE_CURVE('',#11678,#11679,#1901,.F.);
#14258=EDGE_CURVE('',#11679,#11677,#1902,.T.);
#14259=EDGE_CURVE('',#11676,#11678,#1903,.T.);
#14260=EDGE_CURVE('',#11680,#11675,#1904,.T.);
#14261=EDGE_CURVE('',#11681,#11680,#1905,.T.);
#14262=EDGE_CURVE('',#11682,#11681,#1906,.T.);
#14263=EDGE_CURVE('',#11683,#11682,#10303,.T.);
#14264=EDGE_CURVE('',#11684,#11683,#10304,.T.);
#14265=EDGE_CURVE('',#11672,#11684,#1907,.T.);
#14266=EDGE_CURVE('',#11677,#11685,#1908,.T.);
#14267=EDGE_CURVE('',#11686,#11685,#11003,.T.);
#14268=EDGE_CURVE('',#11680,#11686,#11004,.T.);
#14269=EDGE_CURVE('',#11687,#11679,#1909,.T.);
#14270=EDGE_CURVE('',#11685,#11687,#1910,.T.);
#14271=EDGE_CURVE('',#11688,#11686,#11005,.T.);
#14272=EDGE_CURVE('',#11688,#11681,#11006,.T.);
#14273=EDGE_CURVE('',#11685,#11689,#1911,.T.);
#14274=EDGE_CURVE('',#11689,#11688,#11007,.T.);
#14275=EDGE_CURVE('',#11687,#11690,#1912,.F.);
#14276=EDGE_CURVE('',#11690,#11689,#1913,.T.);
#14277=EDGE_CURVE('',#11689,#11691,#1914,.T.);
#14278=EDGE_CURVE('',#11691,#11682,#11008,.F.);
#14279=EDGE_CURVE('',#11692,#11690,#1915,.T.);
#14280=EDGE_CURVE('',#11691,#11692,#1916,.T.);
#14281=EDGE_CURVE('',#11693,#11694,#11009,.T.);
#14282=EDGE_CURVE('',#11695,#11694,#11010,.T.);
#14283=EDGE_CURVE('',#11695,#11696,#11011,.T.);
#14284=EDGE_CURVE('',#11696,#11693,#1917,.T.);
#14285=EDGE_CURVE('',#11694,#11697,#11012,.T.);
#14286=EDGE_CURVE('',#11697,#11698,#1918,.T.);
#14287=EDGE_CURVE('',#11698,#11695,#11013,.T.);
#14288=EDGE_CURVE('',#11699,#11700,#1919,.F.);
#14289=EDGE_CURVE('',#11700,#11698,#1920,.T.);
#14290=EDGE_CURVE('',#11697,#11699,#1921,.T.);
#14291=EDGE_CURVE('',#11701,#11696,#1922,.T.);
#14292=EDGE_CURVE('',#11702,#11701,#1923,.T.);
#14293=EDGE_CURVE('',#11703,#11702,#10305,.T.);
#14294=EDGE_CURVE('',#11693,#11703,#1924,.T.);
#14295=EDGE_CURVE('',#11698,#11704,#1925,.T.);
#14296=EDGE_CURVE('',#11704,#11701,#10306,.T.);
#14297=EDGE_CURVE('',#11705,#11700,#1926,.T.);
#14298=EDGE_CURVE('',#11704,#11705,#1927,.T.);
#14299=EDGE_CURVE('',#11706,#11707,#11014,.T.);
#14300=EDGE_CURVE('',#11708,#11707,#11015,.T.);
#14301=EDGE_CURVE('',#11708,#11709,#11016,.T.);
#14302=EDGE_CURVE('',#11709,#11706,#1928,.T.);
#14303=EDGE_CURVE('',#11707,#11710,#11017,.T.);
#14304=EDGE_CURVE('',#11710,#11711,#1929,.T.);
#14305=EDGE_CURVE('',#11711,#11708,#11018,.T.);
#14306=EDGE_CURVE('',#11712,#11713,#1930,.F.);
#14307=EDGE_CURVE('',#11713,#11711,#1931,.T.);
#14308=EDGE_CURVE('',#11710,#11712,#1932,.T.);
#14309=EDGE_CURVE('',#11714,#11709,#1933,.T.);
#14310=EDGE_CURVE('',#11715,#11714,#1934,.T.);
#14311=EDGE_CURVE('',#11716,#11715,#1935,.T.);
#14312=EDGE_CURVE('',#11717,#11716,#10307,.T.);
#14313=EDGE_CURVE('',#11706,#11717,#1936,.T.);
#14314=EDGE_CURVE('',#11711,#11718,#1937,.T.);
#14315=EDGE_CURVE('',#11719,#11718,#11019,.T.);
#14316=EDGE_CURVE('',#11714,#11719,#11020,.T.);
#14317=EDGE_CURVE('',#11720,#11713,#1938,.T.);
#14318=EDGE_CURVE('',#11718,#11720,#1939,.T.);
#14319=EDGE_CURVE('',#11721,#11719,#11021,.T.);
#14320=EDGE_CURVE('',#11721,#11715,#11022,.T.);
#14321=EDGE_CURVE('',#11718,#11722,#1940,.T.);
#14322=EDGE_CURVE('',#11722,#11721,#11023,.T.);
#14323=EDGE_CURVE('',#11720,#11723,#1941,.F.);
#14324=EDGE_CURVE('',#11723,#11722,#1942,.T.);
#14325=EDGE_CURVE('',#11722,#11724,#1943,.T.);
#14326=EDGE_CURVE('',#11724,#11716,#11024,.F.);
#14327=EDGE_CURVE('',#11725,#11723,#1944,.T.);
#14328=EDGE_CURVE('',#11724,#11725,#1945,.T.);
#14329=EDGE_CURVE('',#11726,#11727,#11025,.T.);
#14330=EDGE_CURVE('',#11728,#11727,#11026,.T.);
#14331=EDGE_CURVE('',#11728,#11729,#11027,.T.);
#14332=EDGE_CURVE('',#11729,#11726,#1946,.T.);
#14333=EDGE_CURVE('',#11727,#11730,#11028,.T.);
#14334=EDGE_CURVE('',#11730,#11731,#1947,.T.);
#14335=EDGE_CURVE('',#11731,#11728,#11029,.T.);
#14336=EDGE_CURVE('',#11732,#11733,#1948,.F.);
#14337=EDGE_CURVE('',#11733,#11731,#1949,.T.);
#14338=EDGE_CURVE('',#11730,#11732,#1950,.T.);
#14339=EDGE_CURVE('',#11734,#11729,#1951,.T.);
#14340=EDGE_CURVE('',#11735,#11734,#1952,.T.);
#14341=EDGE_CURVE('',#11736,#11735,#1953,.T.);
#14342=EDGE_CURVE('',#11737,#11736,#10308,.T.);
#14343=EDGE_CURVE('',#11726,#11737,#1954,.T.);
#14344=EDGE_CURVE('',#11731,#11738,#1955,.T.);
#14345=EDGE_CURVE('',#11739,#11738,#11030,.T.);
#14346=EDGE_CURVE('',#11734,#11739,#11031,.T.);
#14347=EDGE_CURVE('',#11740,#11733,#1956,.T.);
#14348=EDGE_CURVE('',#11738,#11740,#1957,.T.);
#14349=EDGE_CURVE('',#11741,#11739,#11032,.T.);
#14350=EDGE_CURVE('',#11741,#11735,#11033,.T.);
#14351=EDGE_CURVE('',#11738,#11742,#1958,.T.);
#14352=EDGE_CURVE('',#11742,#11741,#11034,.T.);
#14353=EDGE_CURVE('',#11740,#11743,#1959,.F.);
#14354=EDGE_CURVE('',#11743,#11742,#1960,.T.);
#14355=EDGE_CURVE('',#11742,#11744,#1961,.T.);
#14356=EDGE_CURVE('',#11744,#11736,#11035,.F.);
#14357=EDGE_CURVE('',#11745,#11743,#1962,.T.);
#14358=EDGE_CURVE('',#11744,#11745,#1963,.T.);
#14359=EDGE_CURVE('',#11746,#11746,#10309,.T.);
#14360=EDGE_CURVE('',#11746,#11747,#10310,.T.);
#14361=EDGE_CURVE('',#11747,#11747,#10311,.T.);
#14362=EDGE_CURVE('',#11747,#11748,#1964,.T.);
#14363=EDGE_CURVE('',#11748,#11748,#10312,.T.);
#14364=EDGE_CURVE('',#11749,#11749,#10313,.T.);
#14365=EDGE_CURVE('',#11749,#11746,#1965,.T.);
#14366=EDGE_CURVE('',#11748,#11750,#10314,.T.);
#14367=EDGE_CURVE('',#11750,#11750,#10315,.T.);
#14368=EDGE_CURVE('',#11751,#11751,#10316,.T.);
#14369=EDGE_CURVE('',#11752,#11752,#10317,.T.);
#14370=EDGE_CURVE('',#11753,#11753,#10318,.T.);
#14371=EDGE_CURVE('',#11754,#11754,#10319,.T.);
#14372=EDGE_CURVE('',#11755,#11755,#10320,.T.);
#14373=EDGE_CURVE('',#11756,#11756,#10321,.T.);
#14374=EDGE_CURVE('',#11757,#11757,#10322,.T.);
#14375=EDGE_CURVE('',#11758,#11758,#10323,.T.);
#14376=EDGE_CURVE('',#11678,#11759,#1966,.T.);
#14377=EDGE_CURVE('',#11759,#11760,#10324,.T.);
#14378=EDGE_CURVE('',#11760,#11761,#1967,.T.);
#14379=EDGE_CURVE('',#11705,#11761,#10325,.F.);
#14380=EDGE_CURVE('',#11699,#11762,#1968,.T.);
#14381=EDGE_CURVE('',#11762,#11725,#10326,.T.);
#14382=EDGE_CURVE('',#11712,#11763,#1969,.T.);
#14383=EDGE_CURVE('',#11763,#11745,#10327,.T.);
#14384=EDGE_CURVE('',#11732,#11764,#1970,.T.);
#14385=EDGE_CURVE('',#11764,#11692,#10328,.T.);
#14386=EDGE_CURVE('',#11737,#11765,#11036,.F.);
#14387=EDGE_CURVE('',#11765,#11730,#1971,.T.);
#14388=EDGE_CURVE('',#11764,#11765,#1972,.T.);
#14389=EDGE_CURVE('',#11717,#11766,#11037,.F.);
#14390=EDGE_CURVE('',#11766,#11710,#1973,.T.);
#14391=EDGE_CURVE('',#11763,#11766,#1974,.T.);
#14392=EDGE_CURVE('',#11767,#11767,#10329,.T.);
#14393=EDGE_CURVE('',#11767,#11749,#10330,.T.);
#14394=EDGE_CURVE('',#11768,#11769,#10331,.T.);
#14395=EDGE_CURVE('',#11768,#11770,#10332,.T.);
#14396=EDGE_CURVE('',#11770,#11771,#10333,.T.);
#14397=EDGE_CURVE('',#11772,#11771,#10334,.T.);
#14398=EDGE_CURVE('',#11772,#11773,#10335,.T.);
#14399=EDGE_CURVE('',#11773,#11774,#10336,.T.);
#14400=EDGE_CURVE('',#11775,#11774,#10337,.T.);
#14401=EDGE_CURVE('',#11775,#11776,#10338,.T.);
#14402=EDGE_CURVE('',#11776,#11777,#10339,.T.);
#14403=EDGE_CURVE('',#11778,#11777,#10340,.T.);
#14404=EDGE_CURVE('',#11778,#11779,#10341,.T.);
#14405=EDGE_CURVE('',#11779,#11780,#10342,.T.);
#14406=EDGE_CURVE('',#11781,#11780,#10343,.T.);
#14407=EDGE_CURVE('',#11781,#11782,#10344,.T.);
#14408=EDGE_CURVE('',#11782,#11783,#10345,.T.);
#14409=EDGE_CURVE('',#11784,#11783,#10346,.T.);
#14410=EDGE_CURVE('',#11784,#11785,#10347,.T.);
#14411=EDGE_CURVE('',#11785,#11786,#10348,.T.);
#14412=EDGE_CURVE('',#11787,#11786,#10349,.T.);
#14413=EDGE_CURVE('',#11788,#11787,#10350,.T.);
#14414=EDGE_CURVE('',#11788,#11789,#10351,.T.);
#14415=EDGE_CURVE('',#11789,#11790,#10352,.T.);
#14416=EDGE_CURVE('',#11791,#11790,#10353,.T.);
#14417=EDGE_CURVE('',#11791,#11792,#10354,.T.);
#14418=EDGE_CURVE('',#11792,#11769,#10355,.T.);
#14419=EDGE_CURVE('',#11793,#11793,#10356,.T.);
#14420=EDGE_CURVE('',#11793,#11794,#10357,.T.);
#14421=EDGE_CURVE('',#11794,#11794,#10358,.T.);
#14422=EDGE_CURVE('',#11795,#11795,#10359,.T.);
#14423=EDGE_CURVE('',#11795,#11793,#1975,.T.);
#14424=EDGE_CURVE('',#11796,#11797,#11038,.T.);
#14425=EDGE_CURVE('',#11797,#11798,#11039,.T.);
#14426=EDGE_CURVE('',#11798,#11799,#11040,.T.);
#14427=EDGE_CURVE('',#11799,#11800,#1976,.T.);
#14428=EDGE_CURVE('',#11800,#11801,#11041,.T.);
#14429=EDGE_CURVE('',#11801,#11802,#11042,.T.);
#14430=EDGE_CURVE('',#11802,#11803,#11043,.T.);
#14431=EDGE_CURVE('',#11803,#11804,#11044,.T.);
#14432=EDGE_CURVE('',#11804,#11805,#11045,.T.);
#14433=EDGE_CURVE('',#11805,#11806,#11046,.T.);
#14434=EDGE_CURVE('',#11806,#11807,#11047,.T.);
#14435=EDGE_CURVE('',#11807,#11808,#11048,.T.);
#14436=EDGE_CURVE('',#11808,#11809,#11049,.T.);
#14437=EDGE_CURVE('',#11809,#11810,#11050,.T.);
#14438=EDGE_CURVE('',#11810,#11811,#11051,.T.);
#14439=EDGE_CURVE('',#11811,#11812,#11052,.T.);
#14440=EDGE_CURVE('',#11812,#11813,#11053,.T.);
#14441=EDGE_CURVE('',#11813,#11814,#11054,.T.);
#14442=EDGE_CURVE('',#11814,#11815,#11055,.T.);
#14443=EDGE_CURVE('',#11815,#11816,#11056,.T.);
#14444=EDGE_CURVE('',#11816,#11817,#11057,.T.);
#14445=EDGE_CURVE('',#11817,#11818,#11058,.T.);
#14446=EDGE_CURVE('',#11818,#11819,#1977,.T.);
#14447=EDGE_CURVE('',#11819,#11820,#11059,.T.);
#14448=EDGE_CURVE('',#11820,#11821,#11060,.T.);
#14449=EDGE_CURVE('',#11821,#11822,#11061,.T.);
#14450=EDGE_CURVE('',#11822,#11823,#11062,.T.);
#14451=EDGE_CURVE('',#11823,#11824,#11063,.T.);
#14452=EDGE_CURVE('',#11824,#11825,#11064,.T.);
#14453=EDGE_CURVE('',#11825,#11826,#11065,.T.);
#14454=EDGE_CURVE('',#11826,#11827,#11066,.T.);
#14455=EDGE_CURVE('',#11827,#11828,#11067,.T.);
#14456=EDGE_CURVE('',#11828,#11829,#11068,.T.);
#14457=EDGE_CURVE('',#11829,#11830,#11069,.T.);
#14458=EDGE_CURVE('',#11830,#11796,#11070,.T.);
#14459=EDGE_CURVE('',#11831,#11832,#1978,.T.);
#14460=EDGE_CURVE('',#11832,#11833,#1979,.T.);
#14461=EDGE_CURVE('',#11833,#11834,#1980,.T.);
#14462=EDGE_CURVE('',#11834,#11835,#1981,.T.);
#14463=EDGE_CURVE('',#11835,#11836,#1982,.T.);
#14464=EDGE_CURVE('',#11836,#11837,#1983,.T.);
#14465=EDGE_CURVE('',#11837,#11838,#1984,.T.);
#14466=EDGE_CURVE('',#11838,#11839,#11071,.T.);
#14467=EDGE_CURVE('',#11839,#11840,#11072,.T.);
#14468=EDGE_CURVE('',#11840,#11841,#1985,.T.);
#14469=EDGE_CURVE('',#11841,#11831,#1986,.T.);
#14470=EDGE_CURVE('',#11842,#11843,#1987,.T.);
#14471=EDGE_CURVE('',#11843,#11844,#1988,.T.);
#14472=EDGE_CURVE('',#11844,#11845,#1989,.T.);
#14473=EDGE_CURVE('',#11845,#11846,#1990,.T.);
#14474=EDGE_CURVE('',#11846,#11847,#1991,.T.);
#14475=EDGE_CURVE('',#11847,#11848,#1992,.T.);
#14476=EDGE_CURVE('',#11848,#11849,#1993,.T.);
#14477=EDGE_CURVE('',#11849,#11850,#1994,.T.);
#14478=EDGE_CURVE('',#11850,#11851,#1995,.T.);
#14479=EDGE_CURVE('',#11851,#11852,#1996,.T.);
#14480=EDGE_CURVE('',#11853,#11852,#1997,.T.);
#14481=EDGE_CURVE('',#11842,#11853,#1998,.T.);
#14482=EDGE_CURVE('',#11854,#11855,#1999,.T.);
#14483=EDGE_CURVE('',#11855,#11856,#11073,.T.);
#14484=EDGE_CURVE('',#11856,#11857,#11074,.T.);
#14485=EDGE_CURVE('',#11857,#11858,#11075,.T.);
#14486=EDGE_CURVE('',#11858,#11859,#11076,.T.);
#14487=EDGE_CURVE('',#11859,#11860,#11077,.T.);
#14488=EDGE_CURVE('',#11860,#11861,#11078,.T.);
#14489=EDGE_CURVE('',#11861,#11862,#11079,.T.);
#14490=EDGE_CURVE('',#11862,#11863,#11080,.T.);
#14491=EDGE_CURVE('',#11863,#11864,#11081,.T.);
#14492=EDGE_CURVE('',#11864,#11865,#11082,.T.);
#14493=EDGE_CURVE('',#11865,#11866,#11083,.T.);
#14494=EDGE_CURVE('',#11867,#11866,#2000,.T.);
#14495=EDGE_CURVE('',#11854,#11867,#2001,.T.);
#14496=EDGE_CURVE('',#11868,#11869,#2002,.T.);
#14497=EDGE_CURVE('',#11869,#11870,#11084,.T.);
#14498=EDGE_CURVE('',#11870,#11871,#11085,.T.);
#14499=EDGE_CURVE('',#11871,#11872,#11086,.T.);
#14500=EDGE_CURVE('',#11872,#11873,#11087,.T.);
#14501=EDGE_CURVE('',#11873,#11874,#11088,.T.);
#14502=EDGE_CURVE('',#11874,#11875,#11089,.T.);
#14503=EDGE_CURVE('',#11875,#11876,#11090,.T.);
#14504=EDGE_CURVE('',#11876,#11877,#2003,.T.);
#14505=EDGE_CURVE('',#11878,#11877,#2004,.T.);
#14506=EDGE_CURVE('',#11879,#11878,#2005,.T.);
#14507=EDGE_CURVE('',#11880,#11879,#2006,.T.);
#14508=EDGE_CURVE('',#11880,#11881,#2007,.T.);
#14509=EDGE_CURVE('',#11881,#11882,#2008,.T.);
#14510=EDGE_CURVE('',#11882,#11883,#2009,.T.);
#14511=EDGE_CURVE('',#11883,#11884,#2010,.T.);
#14512=EDGE_CURVE('',#11884,#11885,#2011,.T.);
#14513=EDGE_CURVE('',#11885,#11886,#2012,.T.);
#14514=EDGE_CURVE('',#11886,#11887,#11091,.T.);
#14515=EDGE_CURVE('',#11887,#11888,#11092,.T.);
#14516=EDGE_CURVE('',#11888,#11889,#11093,.T.);
#14517=EDGE_CURVE('',#11889,#11890,#11094,.T.);
#14518=EDGE_CURVE('',#11890,#11891,#2013,.T.);
#14519=EDGE_CURVE('',#11891,#11892,#2014,.T.);
#14520=EDGE_CURVE('',#11893,#11892,#2015,.T.);
#14521=EDGE_CURVE('',#11868,#11893,#2016,.T.);
#14522=EDGE_CURVE('',#11703,#11894,#11095,.F.);
#14523=EDGE_CURVE('',#11894,#11697,#2017,.T.);
#14524=EDGE_CURVE('',#11895,#11704,#10360,.T.);
#14525=EDGE_CURVE('',#11761,#11895,#2018,.T.);
#14526=EDGE_CURVE('',#11895,#11701,#10361,.T.);
#14527=EDGE_CURVE('',#11895,#11896,#2019,.T.);
#14528=EDGE_CURVE('',#11896,#11702,#11096,.F.);
#14529=EDGE_CURVE('',#11896,#11760,#2020,.T.);
#14530=EDGE_CURVE('',#11897,#11897,#10362,.T.);
#14531=EDGE_CURVE('',#11897,#11795,#10363,.T.);
#14532=EDGE_CURVE('',#11759,#11898,#2021,.T.);
#14533=EDGE_CURVE('',#11684,#11898,#11097,.F.);
#14534=EDGE_CURVE('',#11683,#11897,#2022,.T.);
#14535=EDGE_CURVE('',#11762,#11894,#2023,.T.);
#14536=EDGE_CURVE('',#11898,#11676,#2024,.T.);
#14537=EDGE_CURVE('',#11899,#11900,#10364,.T.);
#14538=EDGE_CURVE('',#11900,#11901,#11098,.T.);
#14539=EDGE_CURVE('',#11901,#11902,#10365,.T.);
#14540=EDGE_CURVE('',#11902,#11899,#11099,.T.);
#14541=EDGE_CURVE('',#11900,#11903,#2025,.T.);
#14542=EDGE_CURVE('',#11903,#11904,#11100,.F.);
#14543=EDGE_CURVE('',#11904,#11901,#2026,.T.);
#14544=EDGE_CURVE('',#11902,#11905,#2027,.T.);
#14545=EDGE_CURVE('',#11905,#11906,#11101,.F.);
#14546=EDGE_CURVE('',#11906,#11899,#2028,.T.);
#14547=EDGE_CURVE('',#11906,#11903,#10366,.T.);
#14548=EDGE_CURVE('',#11907,#11908,#10367,.T.);
#14549=EDGE_CURVE('',#11908,#11907,#10368,.T.);
#14550=EDGE_CURVE('',#11907,#11909,#10369,.T.);
#14551=EDGE_CURVE('',#11909,#11909,#10370,.T.);
#14552=EDGE_CURVE('',#11905,#11910,#2029,.T.);
#14553=EDGE_CURVE('',#11910,#11911,#10371,.T.);
#14554=EDGE_CURVE('',#11911,#11908,#2030,.T.);
#14555=EDGE_CURVE('',#11911,#11912,#10372,.T.);
#14556=EDGE_CURVE('',#11904,#11912,#2031,.T.);
#14557=EDGE_CURVE('',#11777,#11775,#11102,.T.);
#14558=EDGE_CURVE('',#11774,#11772,#11103,.T.);
#14559=EDGE_CURVE('',#11771,#11768,#11104,.T.);
#14560=EDGE_CURVE('',#11769,#11791,#11105,.T.);
#14561=EDGE_CURVE('',#11790,#11788,#11106,.T.);
#14562=EDGE_CURVE('',#11787,#11913,#10373,.T.);
#14563=EDGE_CURVE('',#11913,#11914,#10374,.T.);
#14564=EDGE_CURVE('',#11914,#11913,#10375,.T.);
#14565=EDGE_CURVE('',#11786,#11784,#11107,.T.);
#14566=EDGE_CURVE('',#11783,#11781,#11108,.T.);
#14567=EDGE_CURVE('',#11780,#11778,#11109,.T.);
#14568=EDGE_CURVE('',#11752,#11770,#2032,.T.);
#14569=EDGE_CURVE('',#11757,#11773,#2033,.T.);
#14570=EDGE_CURVE('',#11751,#11776,#2034,.T.);
#14571=EDGE_CURVE('',#11758,#11779,#2035,.T.);
#14572=EDGE_CURVE('',#11915,#11915,#10376,.T.);
#14573=EDGE_CURVE('',#11915,#11914,#2036,.T.);
#14574=EDGE_CURVE('',#11868,#11916,#10377,.T.);
#14575=EDGE_CURVE('',#11893,#11917,#10378,.F.);
#14576=EDGE_CURVE('',#11917,#11916,#2037,.T.);
#14577=EDGE_CURVE('',#11854,#11918,#10379,.T.);
#14578=EDGE_CURVE('',#11867,#11919,#10380,.F.);
#14579=EDGE_CURVE('',#11919,#11918,#2038,.T.);
#14580=EDGE_CURVE('',#11842,#11920,#10381,.T.);
#14581=EDGE_CURVE('',#11853,#11921,#10382,.F.);
#14582=EDGE_CURVE('',#11921,#11920,#2039,.T.);
#14583=EDGE_CURVE('',#11878,#11922,#197,.T.);
#14584=EDGE_CURVE('',#11877,#11923,#198,.T.);
#14585=EDGE_CURVE('',#11923,#11924,#199,.F.);
#14586=EDGE_CURVE('',#11924,#11922,#2040,.T.);
#14587=EDGE_CURVE('',#11880,#11925,#200,.T.);
#14588=EDGE_CURVE('',#11879,#11926,#201,.F.);
#14589=EDGE_CURVE('',#11926,#11925,#2041,.T.);
#14590=EDGE_CURVE('',#11882,#11927,#2042,.T.);
#14591=EDGE_CURVE('',#11927,#11928,#2043,.T.);
#14592=EDGE_CURVE('',#11883,#11928,#2044,.T.);
#14593=EDGE_CURVE('',#11881,#11929,#2045,.T.);
#14594=EDGE_CURVE('',#11929,#11927,#2046,.T.);
#14595=EDGE_CURVE('',#11925,#11929,#2047,.T.);
#14596=EDGE_CURVE('',#11922,#11926,#2048,.T.);
#14597=EDGE_CURVE('',#11884,#11930,#2049,.T.);
#14598=EDGE_CURVE('',#11930,#11924,#2050,.T.);
#14599=EDGE_CURVE('',#11923,#11931,#2051,.T.);
#14600=EDGE_CURVE('',#11931,#11932,#2052,.T.);
#14601=EDGE_CURVE('',#11885,#11932,#2053,.T.);
#14602=EDGE_CURVE('',#11928,#11930,#2054,.T.);
#14603=EDGE_CURVE('',#11850,#11933,#2055,.T.);
#14604=EDGE_CURVE('',#11933,#11934,#2056,.T.);
#14605=EDGE_CURVE('',#11851,#11934,#2057,.T.);
#14606=EDGE_CURVE('',#11849,#11935,#2058,.T.);
#14607=EDGE_CURVE('',#11935,#11933,#2059,.T.);
#14608=EDGE_CURVE('',#11848,#11936,#2060,.T.);
#14609=EDGE_CURVE('',#11936,#11935,#2061,.T.);
#14610=EDGE_CURVE('',#11847,#11937,#2062,.T.);
#14611=EDGE_CURVE('',#11937,#11936,#2063,.T.);
#14612=EDGE_CURVE('',#11846,#11938,#2064,.T.);
#14613=EDGE_CURVE('',#11938,#11937,#2065,.T.);
#14614=EDGE_CURVE('',#11845,#11939,#2066,.T.);
#14615=EDGE_CURVE('',#11939,#11938,#2067,.T.);
#14616=EDGE_CURVE('',#11844,#11940,#2068,.T.);
#14617=EDGE_CURVE('',#11940,#11939,#2069,.T.);
#14618=EDGE_CURVE('',#11843,#11941,#2070,.T.);
#14619=EDGE_CURVE('',#11941,#11940,#2071,.T.);
#14620=EDGE_CURVE('',#11920,#11941,#2072,.T.);
#14621=EDGE_CURVE('',#11852,#11942,#2073,.T.);
#14622=EDGE_CURVE('',#11942,#11921,#2074,.T.);
#14623=EDGE_CURVE('',#11934,#11942,#2075,.T.);
#14624=EDGE_CURVE('',#11864,#11943,#2076,.T.);
#14625=EDGE_CURVE('',#11943,#11944,#11110,.T.);
#14626=EDGE_CURVE('',#11865,#11944,#2077,.T.);
#14627=EDGE_CURVE('',#11863,#11945,#2078,.T.);
#14628=EDGE_CURVE('',#11945,#11943,#11111,.T.);
#14629=EDGE_CURVE('',#11862,#11946,#2079,.T.);
#14630=EDGE_CURVE('',#11946,#11945,#11112,.T.);
#14631=EDGE_CURVE('',#11861,#11947,#2080,.T.);
#14632=EDGE_CURVE('',#11947,#11946,#11113,.T.);
#14633=EDGE_CURVE('',#11860,#11948,#2081,.T.);
#14634=EDGE_CURVE('',#11948,#11947,#11114,.T.);
#14635=EDGE_CURVE('',#11859,#11949,#2082,.T.);
#14636=EDGE_CURVE('',#11949,#11948,#11115,.T.);
#14637=EDGE_CURVE('',#11858,#11950,#2083,.T.);
#14638=EDGE_CURVE('',#11950,#11949,#11116,.T.);
#14639=EDGE_CURVE('',#11857,#11951,#2084,.T.);
#14640=EDGE_CURVE('',#11951,#11950,#11117,.T.);
#14641=EDGE_CURVE('',#11856,#11952,#2085,.T.);
#14642=EDGE_CURVE('',#11952,#11951,#11118,.T.);
#14643=EDGE_CURVE('',#11855,#11953,#2086,.T.);
#14644=EDGE_CURVE('',#11953,#11952,#11119,.T.);
#14645=EDGE_CURVE('',#11918,#11953,#2087,.T.);
#14646=EDGE_CURVE('',#11866,#11954,#2088,.T.);
#14647=EDGE_CURVE('',#11954,#11919,#2089,.T.);
#14648=EDGE_CURVE('',#11944,#11954,#11120,.T.);
#14649=EDGE_CURVE('',#11796,#11955,#2090,.T.);
#14650=EDGE_CURVE('',#11955,#11956,#11121,.T.);
#14651=EDGE_CURVE('',#11797,#11956,#2091,.T.);
#14652=EDGE_CURVE('',#11830,#11957,#2092,.T.);
#14653=EDGE_CURVE('',#11957,#11955,#11122,.T.);
#14654=EDGE_CURVE('',#11829,#11958,#2093,.T.);
#14655=EDGE_CURVE('',#11958,#11957,#11123,.T.);
#14656=EDGE_CURVE('',#11828,#11959,#2094,.T.);
#14657=EDGE_CURVE('',#11959,#11958,#11124,.T.);
#14658=EDGE_CURVE('',#11827,#11960,#2095,.T.);
#14659=EDGE_CURVE('',#11960,#11959,#11125,.T.);
#14660=EDGE_CURVE('',#11826,#11961,#2096,.T.);
#14661=EDGE_CURVE('',#11961,#11960,#11126,.T.);
#14662=EDGE_CURVE('',#11825,#11962,#2097,.T.);
#14663=EDGE_CURVE('',#11962,#11961,#11127,.T.);
#14664=EDGE_CURVE('',#11824,#11963,#2098,.T.);
#14665=EDGE_CURVE('',#11963,#11962,#11128,.T.);
#14666=EDGE_CURVE('',#11823,#11964,#2099,.T.);
#14667=EDGE_CURVE('',#11964,#11963,#11129,.T.);
#14668=EDGE_CURVE('',#11822,#11965,#2100,.T.);
#14669=EDGE_CURVE('',#11965,#11964,#11130,.T.);
#14670=EDGE_CURVE('',#11821,#11966,#2101,.T.);
#14671=EDGE_CURVE('',#11966,#11965,#11131,.T.);
#14672=EDGE_CURVE('',#11820,#11967,#2102,.T.);
#14673=EDGE_CURVE('',#11967,#11966,#11132,.T.);
#14674=EDGE_CURVE('',#11819,#11968,#2103,.T.);
#14675=EDGE_CURVE('',#11968,#11967,#11133,.T.);
#14676=EDGE_CURVE('',#11818,#11969,#2104,.T.);
#14677=EDGE_CURVE('',#11969,#11968,#2105,.T.);
#14678=EDGE_CURVE('',#11817,#11970,#2106,.T.);
#14679=EDGE_CURVE('',#11970,#11969,#11134,.T.);
#14680=EDGE_CURVE('',#11816,#11971,#2107,.T.);
#14681=EDGE_CURVE('',#11971,#11970,#11135,.T.);
#14682=EDGE_CURVE('',#11815,#11972,#2108,.T.);
#14683=EDGE_CURVE('',#11972,#11971,#11136,.T.);
#14684=EDGE_CURVE('',#11814,#11973,#2109,.T.);
#14685=EDGE_CURVE('',#11973,#11972,#11137,.T.);
#14686=EDGE_CURVE('',#11813,#11974,#2110,.T.);
#14687=EDGE_CURVE('',#11974,#11973,#11138,.T.);
#14688=EDGE_CURVE('',#11812,#11975,#2111,.T.);
#14689=EDGE_CURVE('',#11975,#11974,#11139,.T.);
#14690=EDGE_CURVE('',#11811,#11976,#2112,.T.);
#14691=EDGE_CURVE('',#11976,#11975,#11140,.T.);
#14692=EDGE_CURVE('',#11810,#11977,#2113,.T.);
#14693=EDGE_CURVE('',#11977,#11976,#11141,.T.);
#14694=EDGE_CURVE('',#11809,#11978,#2114,.T.);
#14695=EDGE_CURVE('',#11978,#11977,#11142,.T.);
#14696=EDGE_CURVE('',#11808,#11979,#2115,.T.);
#14697=EDGE_CURVE('',#11979,#11978,#11143,.T.);
#14698=EDGE_CURVE('',#11807,#11980,#2116,.T.);
#14699=EDGE_CURVE('',#11980,#11979,#11144,.T.);
#14700=EDGE_CURVE('',#11806,#11981,#2117,.T.);
#14701=EDGE_CURVE('',#11981,#11980,#11145,.T.);
#14702=EDGE_CURVE('',#11805,#11982,#2118,.T.);
#14703=EDGE_CURVE('',#11982,#11981,#11146,.T.);
#14704=EDGE_CURVE('',#11804,#11983,#2119,.T.);
#14705=EDGE_CURVE('',#11983,#11982,#11147,.T.);
#14706=EDGE_CURVE('',#11803,#11984,#2120,.T.);
#14707=EDGE_CURVE('',#11984,#11983,#11148,.T.);
#14708=EDGE_CURVE('',#11802,#11985,#2121,.T.);
#14709=EDGE_CURVE('',#11985,#11984,#11149,.T.);
#14710=EDGE_CURVE('',#11801,#11986,#2122,.T.);
#14711=EDGE_CURVE('',#11986,#11985,#11150,.T.);
#14712=EDGE_CURVE('',#11800,#11987,#2123,.T.);
#14713=EDGE_CURVE('',#11987,#11986,#11151,.T.);
#14714=EDGE_CURVE('',#11799,#11988,#2124,.T.);
#14715=EDGE_CURVE('',#11988,#11987,#2125,.T.);
#14716=EDGE_CURVE('',#11798,#11989,#2126,.T.);
#14717=EDGE_CURVE('',#11989,#11988,#11152,.T.);
#14718=EDGE_CURVE('',#11956,#11989,#11153,.T.);
#14719=EDGE_CURVE('',#11890,#11990,#2127,.T.);
#14720=EDGE_CURVE('',#11990,#11991,#2128,.T.);
#14721=EDGE_CURVE('',#11891,#11991,#2129,.T.);
#14722=EDGE_CURVE('',#11889,#11992,#2130,.T.);
#14723=EDGE_CURVE('',#11992,#11990,#11154,.T.);
#14724=EDGE_CURVE('',#11888,#11993,#2131,.T.);
#14725=EDGE_CURVE('',#11993,#11992,#11155,.T.);
#14726=EDGE_CURVE('',#11887,#11994,#2132,.T.);
#14727=EDGE_CURVE('',#11994,#11993,#11156,.T.);
#14728=EDGE_CURVE('',#11886,#11995,#2133,.T.);
#14729=EDGE_CURVE('',#11995,#11994,#11157,.T.);
#14730=EDGE_CURVE('',#11932,#11995,#2134,.T.);
#14731=EDGE_CURVE('',#11876,#11996,#2135,.T.);
#14732=EDGE_CURVE('',#11996,#11931,#2136,.T.);
#14733=EDGE_CURVE('',#11875,#11997,#2137,.T.);
#14734=EDGE_CURVE('',#11997,#11996,#11158,.T.);
#14735=EDGE_CURVE('',#11874,#11998,#2138,.T.);
#14736=EDGE_CURVE('',#11998,#11997,#11159,.T.);
#14737=EDGE_CURVE('',#11873,#11999,#2139,.T.);
#14738=EDGE_CURVE('',#11999,#11998,#11160,.T.);
#14739=EDGE_CURVE('',#11872,#12000,#2140,.T.);
#14740=EDGE_CURVE('',#12000,#11999,#11161,.T.);
#14741=EDGE_CURVE('',#11871,#12001,#2141,.T.);
#14742=EDGE_CURVE('',#12001,#12000,#11162,.T.);
#14743=EDGE_CURVE('',#11870,#12002,#2142,.T.);
#14744=EDGE_CURVE('',#12002,#12001,#11163,.T.);
#14745=EDGE_CURVE('',#11869,#12003,#2143,.T.);
#14746=EDGE_CURVE('',#12003,#12002,#11164,.T.);
#14747=EDGE_CURVE('',#11916,#12003,#2144,.T.);
#14748=EDGE_CURVE('',#11892,#12004,#2145,.T.);
#14749=EDGE_CURVE('',#12004,#11917,#2146,.T.);
#14750=EDGE_CURVE('',#11991,#12004,#2147,.T.);
#14751=EDGE_CURVE('',#11831,#12005,#2148,.T.);
#14752=EDGE_CURVE('',#12005,#12006,#2149,.T.);
#14753=EDGE_CURVE('',#11832,#12006,#2150,.T.);
#14754=EDGE_CURVE('',#11841,#12007,#2151,.T.);
#14755=EDGE_CURVE('',#12007,#12005,#2152,.T.);
#14756=EDGE_CURVE('',#11840,#12008,#2153,.T.);
#14757=EDGE_CURVE('',#12008,#12007,#2154,.T.);
#14758=EDGE_CURVE('',#11839,#12009,#2155,.T.);
#14759=EDGE_CURVE('',#12009,#12008,#11165,.T.);
#14760=EDGE_CURVE('',#11838,#12010,#2156,.T.);
#14761=EDGE_CURVE('',#12010,#12009,#11166,.T.);
#14762=EDGE_CURVE('',#11837,#12011,#2157,.T.);
#14763=EDGE_CURVE('',#12011,#12010,#2158,.T.);
#14764=EDGE_CURVE('',#11836,#12012,#2159,.T.);
#14765=EDGE_CURVE('',#12012,#12011,#2160,.T.);
#14766=EDGE_CURVE('',#11835,#12013,#2161,.T.);
#14767=EDGE_CURVE('',#12013,#12012,#2162,.T.);
#14768=EDGE_CURVE('',#11834,#12014,#2163,.T.);
#14769=EDGE_CURVE('',#12014,#12013,#2164,.T.);
#14770=EDGE_CURVE('',#11833,#12015,#2165,.T.);
#14771=EDGE_CURVE('',#12015,#12014,#2166,.T.);
#14772=EDGE_CURVE('',#12006,#12015,#2167,.T.);
#14773=EDGE_CURVE('',#11753,#11792,#2168,.T.);
#14774=EDGE_CURVE('',#11754,#11785,#2169,.T.);
#14775=EDGE_CURVE('',#11755,#11789,#2170,.T.);
#14776=EDGE_CURVE('',#11756,#11782,#2171,.T.);
#14777=EDGE_CURVE('',#11901,#12016,#2172,.T.);
#14778=EDGE_CURVE('',#12016,#12017,#10383,.T.);
#14779=EDGE_CURVE('',#11902,#12017,#2173,.T.);
#14780=EDGE_CURVE('',#11912,#12016,#2174,.T.);
#14781=EDGE_CURVE('',#12017,#11910,#2175,.T.);
#14782=EDGE_CURVE('',#12018,#12018,#10384,.T.);
#14783=EDGE_CURVE('',#12018,#12019,#2176,.T.);
#14784=EDGE_CURVE('',#12019,#12019,#10385,.T.);
#14785=EDGE_CURVE('',#12020,#12020,#10386,.T.);
#14786=EDGE_CURVE('',#12020,#12019,#2177,.T.);
#14787=EDGE_CURVE('',#12021,#12022,#10387,.T.);
#14788=EDGE_CURVE('',#12023,#12022,#2178,.T.);
#14789=EDGE_CURVE('',#12023,#12024,#10388,.T.);
#14790=EDGE_CURVE('',#12025,#12024,#2179,.T.);
#14791=EDGE_CURVE('',#12025,#12026,#10389,.T.);
#14792=EDGE_CURVE('',#12027,#12026,#2180,.T.);
#14793=EDGE_CURVE('',#12027,#12028,#10390,.T.);
#14794=EDGE_CURVE('',#12021,#12028,#2181,.T.);
#14795=EDGE_CURVE('',#12020,#12029,#2182,.T.);
#14796=EDGE_CURVE('',#12029,#12029,#10391,.T.);
#14797=EDGE_CURVE('',#12030,#12030,#10392,.T.);
#14798=EDGE_CURVE('',#12031,#12031,#10393,.T.);
#14799=EDGE_CURVE('',#12031,#12032,#2183,.T.);
#14800=EDGE_CURVE('',#12032,#12032,#10394,.T.);
#14801=EDGE_CURVE('',#12033,#12034,#10395,.T.);
#14802=EDGE_CURVE('',#12034,#12035,#2184,.T.);
#14803=EDGE_CURVE('',#12035,#12036,#10396,.T.);
#14804=EDGE_CURVE('',#12036,#12037,#2185,.T.);
#14805=EDGE_CURVE('',#12037,#12038,#10397,.T.);
#14806=EDGE_CURVE('',#12038,#12039,#2186,.T.);
#14807=EDGE_CURVE('',#12040,#12039,#2187,.T.);
#14808=EDGE_CURVE('',#12039,#12041,#2188,.T.);
#14809=EDGE_CURVE('',#12041,#12042,#10398,.T.);
#14810=EDGE_CURVE('',#12042,#12033,#2189,.T.);
#14811=EDGE_CURVE('',#12043,#12043,#10399,.T.);
#14812=EDGE_CURVE('',#12044,#12045,#2190,.T.);
#14813=EDGE_CURVE('',#12046,#12044,#10400,.T.);
#14814=EDGE_CURVE('',#12047,#12046,#2191,.T.);
#14815=EDGE_CURVE('',#12048,#12047,#10401,.T.);
#14816=EDGE_CURVE('',#12049,#12048,#2192,.T.);
#14817=EDGE_CURVE('',#12050,#12049,#10402,.T.);
#14818=EDGE_CURVE('',#12051,#12050,#2193,.T.);
#14819=EDGE_CURVE('',#12045,#12051,#10403,.T.);
#14820=EDGE_CURVE('',#12032,#12052,#2194,.T.);
#14821=EDGE_CURVE('',#12052,#12052,#10404,.T.);
#14822=EDGE_CURVE('',#12043,#12053,#2195,.T.);
#14823=EDGE_CURVE('',#12053,#12053,#10405,.T.);
#14824=EDGE_CURVE('',#12053,#12054,#2196,.T.);
#14825=EDGE_CURVE('',#12054,#12054,#10406,.T.);
#14826=EDGE_CURVE('',#12055,#12056,#2197,.T.);
#14827=EDGE_CURVE('',#12056,#12057,#10407,.T.);
#14828=EDGE_CURVE('',#12057,#12058,#2198,.T.);
#14829=EDGE_CURVE('',#12058,#12055,#10408,.T.);
#14830=EDGE_CURVE('',#12055,#12058,#11167,.T.);
#14831=EDGE_CURVE('',#12057,#12059,#11168,.T.);
#14832=EDGE_CURVE('',#12059,#12056,#11169,.T.);
#14833=EDGE_CURVE('',#12060,#12058,#2199,.T.);
#14834=EDGE_CURVE('',#12061,#12060,#10409,.T.);
#14835=EDGE_CURVE('',#12025,#12061,#2200,.T.);
#14836=EDGE_CURVE('',#12024,#12062,#2201,.T.);
#14837=EDGE_CURVE('',#12063,#12062,#10410,.T.);
#14838=EDGE_CURVE('',#12063,#12064,#2202,.T.);
#14839=EDGE_CURVE('',#12065,#12064,#10411,.T.);
#14840=EDGE_CURVE('',#12065,#12066,#2203,.T.);
#14841=EDGE_CURVE('',#12066,#12067,#2204,.T.);
#14842=EDGE_CURVE('',#12067,#12068,#2205,.T.);
#14843=EDGE_CURVE('',#12055,#12068,#2206,.T.);
#14844=EDGE_CURVE('',#12069,#12070,#2207,.T.);
#14845=EDGE_CURVE('',#12071,#12069,#10412,.T.);
#14846=EDGE_CURVE('',#12072,#12071,#2208,.T.);
#14847=EDGE_CURVE('',#12073,#12072,#10413,.T.);
#14848=EDGE_CURVE('',#12074,#12073,#2209,.T.);
#14849=EDGE_CURVE('',#12075,#12074,#10414,.T.);
#14850=EDGE_CURVE('',#12076,#12075,#2210,.T.);
#14851=EDGE_CURVE('',#12070,#12076,#10415,.T.);
#14852=EDGE_CURVE('',#12077,#12077,#10416,.T.);
#14853=EDGE_CURVE('',#12077,#12059,#2211,.T.);
#14854=EDGE_CURVE('',#12062,#12078,#2212,.T.);
#14855=EDGE_CURVE('',#12078,#12079,#10417,.T.);
#14856=EDGE_CURVE('',#12079,#12080,#10418,.T.);
#14857=EDGE_CURVE('',#12080,#12063,#2213,.T.);
#14858=EDGE_CURVE('',#12062,#12063,#11170,.T.);
#14859=EDGE_CURVE('',#12080,#12078,#11171,.T.);
#14860=EDGE_CURVE('',#12023,#12081,#2214,.T.);
#14861=EDGE_CURVE('',#12081,#12066,#10419,.T.);
#14862=EDGE_CURVE('',#12064,#12065,#11172,.T.);
#14863=EDGE_CURVE('',#12082,#12082,#10420,.T.);
#14864=EDGE_CURVE('',#12082,#12079,#2215,.T.);
#14865=EDGE_CURVE('',#12060,#12083,#2216,.T.);
#14866=EDGE_CURVE('',#12083,#12084,#10421,.T.);
#14867=EDGE_CURVE('',#12084,#12061,#2217,.T.);
#14868=EDGE_CURVE('',#12060,#12061,#11173,.T.);
#14869=EDGE_CURVE('',#12084,#12085,#11174,.T.);
#14870=EDGE_CURVE('',#12085,#12083,#11175,.T.);
#14871=EDGE_CURVE('',#12086,#12086,#10422,.T.);
#14872=EDGE_CURVE('',#12086,#12085,#2218,.T.);
#14873=EDGE_CURVE('',#12064,#12087,#2219,.T.);
#14874=EDGE_CURVE('',#12087,#12088,#10423,.T.);
#14875=EDGE_CURVE('',#12088,#12089,#10424,.T.);
#14876=EDGE_CURVE('',#12089,#12065,#2220,.T.);
#14877=EDGE_CURVE('',#12089,#12087,#11176,.T.);
#14878=EDGE_CURVE('',#12090,#12090,#10425,.T.);
#14879=EDGE_CURVE('',#12090,#12088,#2221,.T.);
#14880=EDGE_CURVE('',#12091,#12091,#10426,.T.);
#14881=EDGE_CURVE('',#12091,#12090,#2222,.T.);
#14882=EDGE_CURVE('',#12092,#12093,#2223,.T.);
#14883=EDGE_CURVE('',#12092,#12094,#2224,.T.);
#14884=EDGE_CURVE('',#12094,#12095,#155,.T.);
#14885=EDGE_CURVE('',#12096,#12095,#11177,.F.);
#14886=EDGE_CURVE('',#12096,#12097,#2225,.T.);
#14887=EDGE_CURVE('',#12098,#12097,#11178,.F.);
#14888=EDGE_CURVE('',#12098,#12099,#156,.T.);
#14889=EDGE_CURVE('',#12093,#12099,#2226,.T.);
#14890=EDGE_CURVE('',#12100,#12100,#10427,.T.);
#14891=EDGE_CURVE('',#12101,#12101,#10428,.T.);
#14892=EDGE_CURVE('',#12102,#12103,#2227,.T.);
#14893=EDGE_CURVE('',#12104,#12102,#10429,.T.);
#14894=EDGE_CURVE('',#12105,#12104,#2228,.T.);
#14895=EDGE_CURVE('',#12106,#12105,#10430,.T.);
#14896=EDGE_CURVE('',#12107,#12106,#2229,.T.);
#14897=EDGE_CURVE('',#12108,#12107,#10431,.T.);
#14898=EDGE_CURVE('',#12109,#12108,#2230,.T.);
#14899=EDGE_CURVE('',#12103,#12109,#10432,.T.);
#14900=EDGE_CURVE('',#12110,#12110,#10433,.T.);
#14901=EDGE_CURVE('',#12100,#12086,#2231,.T.);
#14902=EDGE_CURVE('',#12110,#12082,#2232,.T.);
#14903=EDGE_CURVE('',#12101,#12077,#2233,.T.);
#14904=EDGE_CURVE('',#12111,#12111,#10434,.T.);
#14905=EDGE_CURVE('',#12111,#12112,#2234,.T.);
#14906=EDGE_CURVE('',#12112,#12112,#10435,.T.);
#14907=EDGE_CURVE('',#12113,#12113,#10436,.T.);
#14908=EDGE_CURVE('',#12114,#12114,#10437,.T.);
#14909=EDGE_CURVE('',#12115,#12115,#10438,.T.);
#14910=EDGE_CURVE('',#12116,#12116,#10439,.T.);
#14911=EDGE_CURVE('',#12117,#12117,#10440,.T.);
#14912=EDGE_CURVE('',#12118,#12118,#10441,.T.);
#14913=EDGE_CURVE('',#12118,#12112,#2235,.T.);
#14914=EDGE_CURVE('',#12114,#12119,#2236,.T.);
#14915=EDGE_CURVE('',#12119,#12119,#10442,.T.);
#14916=EDGE_CURVE('',#12120,#12120,#10443,.T.);
#14917=EDGE_CURVE('',#12120,#12119,#2237,.T.);
#14918=EDGE_CURVE('',#12117,#12121,#2238,.T.);
#14919=EDGE_CURVE('',#12121,#12121,#10444,.T.);
#14920=EDGE_CURVE('',#12122,#12122,#10445,.T.);
#14921=EDGE_CURVE('',#12122,#12121,#2239,.T.);
#14922=EDGE_CURVE('',#12115,#12123,#2240,.T.);
#14923=EDGE_CURVE('',#12123,#12123,#10446,.T.);
#14924=EDGE_CURVE('',#12124,#12124,#10447,.T.);
#14925=EDGE_CURVE('',#12124,#12123,#2241,.T.);
#14926=EDGE_CURVE('',#12125,#12125,#10448,.T.);
#14927=EDGE_CURVE('',#12125,#12054,#2242,.T.);
#14928=EDGE_CURVE('',#12126,#12127,#2243,.T.);
#14929=EDGE_CURVE('',#12128,#12126,#10449,.T.);
#14930=EDGE_CURVE('',#12129,#12128,#2244,.T.);
#14931=EDGE_CURVE('',#12130,#12129,#10450,.T.);
#14932=EDGE_CURVE('',#12131,#12130,#2245,.T.);
#14933=EDGE_CURVE('',#12132,#12131,#10451,.T.);
#14934=EDGE_CURVE('',#12133,#12132,#2246,.T.);
#14935=EDGE_CURVE('',#12127,#12133,#10452,.T.);
#14936=EDGE_CURVE('',#12134,#12134,#10453,.T.);
#14937=EDGE_CURVE('',#12134,#12052,#2247,.T.);
#14938=EDGE_CURVE('',#12135,#12135,#10454,.T.);
#14939=EDGE_CURVE('',#12135,#12136,#10455,.T.);
#14940=EDGE_CURVE('',#12136,#12136,#10456,.T.);
#14941=EDGE_CURVE('',#12135,#12137,#2248,.T.);
#14942=EDGE_CURVE('',#12137,#12137,#10457,.T.);
#14943=EDGE_CURVE('',#12138,#12138,#10458,.T.);
#14944=EDGE_CURVE('',#12139,#12139,#10459,.T.);
#14945=EDGE_CURVE('',#12140,#12140,#10460,.T.);
#14946=EDGE_CURVE('',#12141,#12141,#10461,.T.);
#14947=EDGE_CURVE('',#12142,#12142,#10462,.T.);
#14948=EDGE_CURVE('',#12137,#12143,#10463,.T.);
#14949=EDGE_CURVE('',#12143,#12143,#10464,.T.);
#14950=EDGE_CURVE('',#12144,#12144,#10465,.T.);
#14951=EDGE_CURVE('',#12145,#12145,#10466,.T.);
#14952=EDGE_CURVE('',#12146,#12146,#10467,.T.);
#14953=EDGE_CURVE('',#12147,#12147,#10468,.T.);
#14954=EDGE_CURVE('',#12148,#12148,#10469,.T.);
#14955=EDGE_CURVE('',#12149,#12149,#10470,.T.);
#14956=EDGE_CURVE('',#12149,#12150,#10471,.T.);
#14957=EDGE_CURVE('',#12150,#12150,#10472,.T.);
#14958=EDGE_CURVE('',#12150,#12151,#2249,.T.);
#14959=EDGE_CURVE('',#12151,#12151,#10473,.T.);
#14960=EDGE_CURVE('',#12040,#12040,#10474,.T.);
#14961=EDGE_CURVE('',#12040,#12149,#2250,.T.);
#14962=EDGE_CURVE('',#12151,#12152,#10475,.T.);
#14963=EDGE_CURVE('',#12152,#12152,#10476,.T.);
#14964=EDGE_CURVE('',#12152,#12153,#2251,.T.);
#14965=EDGE_CURVE('',#12153,#12154,#10477,.T.);
#14966=EDGE_CURVE('',#12154,#12155,#11179,.T.);
#14967=EDGE_CURVE('',#12156,#12155,#157,.T.);
#14968=EDGE_CURVE('',#12156,#12099,#11180,.T.);
#14969=EDGE_CURVE('',#12095,#12098,#10478,.T.);
#14970=EDGE_CURVE('',#12094,#12157,#11181,.T.);
#14971=EDGE_CURVE('',#12158,#12157,#158,.T.);
#14972=EDGE_CURVE('',#12159,#12158,#10479,.T.);
#14973=EDGE_CURVE('',#12160,#12159,#159,.T.);
#14974=EDGE_CURVE('',#12160,#12161,#11182,.T.);
#14975=EDGE_CURVE('',#12162,#12161,#160,.T.);
#14976=EDGE_CURVE('',#12163,#12162,#10480,.T.);
#14977=EDGE_CURVE('',#12164,#12163,#161,.T.);
#14978=EDGE_CURVE('',#12164,#12165,#11183,.T.);
#14979=EDGE_CURVE('',#12166,#12165,#162,.T.);
#14980=EDGE_CURVE('',#12166,#12167,#11184,.T.);
#14981=EDGE_CURVE('',#12167,#12153,#10481,.T.);
#14982=EDGE_CURVE('',#12162,#12168,#11185,.F.);
#14983=EDGE_CURVE('',#12168,#12169,#10482,.T.);
#14984=EDGE_CURVE('',#12169,#12163,#11186,.F.);
#14985=EDGE_CURVE('',#12169,#12168,#2252,.T.);
#14986=EDGE_CURVE('',#12158,#12170,#11187,.F.);
#14987=EDGE_CURVE('',#12170,#12171,#10483,.T.);
#14988=EDGE_CURVE('',#12171,#12159,#11188,.F.);
#14989=EDGE_CURVE('',#12171,#12170,#2253,.T.);
#14990=EDGE_CURVE('',#12097,#12096,#10484,.T.);
#14991=EDGE_CURVE('',#12172,#12126,#10485,.T.);
#14992=EDGE_CURVE('',#12127,#12173,#10486,.T.);
#14993=EDGE_CURVE('',#12173,#12172,#2254,.T.);
#14994=EDGE_CURVE('',#12133,#12174,#10487,.T.);
#14995=EDGE_CURVE('',#12174,#12173,#10488,.T.);
#14996=EDGE_CURVE('',#12132,#12175,#10489,.T.);
#14997=EDGE_CURVE('',#12175,#12174,#2255,.T.);
#14998=EDGE_CURVE('',#12131,#12176,#10490,.T.);
#14999=EDGE_CURVE('',#12176,#12175,#10491,.T.);
#15000=EDGE_CURVE('',#12130,#12177,#10492,.T.);
#15001=EDGE_CURVE('',#12177,#12176,#2256,.T.);
#15002=EDGE_CURVE('',#12129,#12178,#10493,.T.);
#15003=EDGE_CURVE('',#12178,#12177,#10494,.T.);
#15004=EDGE_CURVE('',#12128,#12179,#10495,.T.);
#15005=EDGE_CURVE('',#12179,#12178,#2257,.T.);
#15006=EDGE_CURVE('',#12172,#12179,#10496,.T.);
#15007=EDGE_CURVE('',#12178,#12038,#2258,.T.);
#15008=EDGE_CURVE('',#12177,#12037,#2259,.T.);
#15009=EDGE_CURVE('',#12179,#12041,#2260,.T.);
#15010=EDGE_CURVE('',#12172,#12042,#2261,.T.);
#15011=EDGE_CURVE('',#12173,#12033,#2262,.T.);
#15012=EDGE_CURVE('',#12113,#12180,#10497,.T.);
#15013=EDGE_CURVE('',#12180,#12180,#10498,.T.);
#15014=EDGE_CURVE('',#12180,#12039,#2263,.T.);
#15015=EDGE_CURVE('',#12040,#12039,#2264,.T.);
#15016=EDGE_CURVE('',#12067,#12181,#10499,.T.);
#15017=EDGE_CURVE('',#12181,#12182,#10500,.T.);
#15018=EDGE_CURVE('',#12182,#12182,#10501,.T.);
#15019=EDGE_CURVE('',#12181,#12183,#10502,.T.);
#15020=EDGE_CURVE('',#12183,#12184,#10503,.T.);
#15021=EDGE_CURVE('',#12184,#12067,#10504,.T.);
#15022=EDGE_CURVE('',#12185,#12183,#2265,.T.);
#15023=EDGE_CURVE('',#12186,#12185,#10505,.T.);
#15024=EDGE_CURVE('',#12184,#12186,#2266,.T.);
#15025=EDGE_CURVE('',#12187,#12181,#2267,.T.);
#15026=EDGE_CURVE('',#12188,#12187,#10506,.T.);
#15027=EDGE_CURVE('',#12183,#12188,#2268,.T.);
#15028=EDGE_CURVE('',#12181,#12081,#2269,.T.);
#15029=EDGE_CURVE('',#12189,#12184,#2270,.T.);
#15030=EDGE_CURVE('',#12068,#12189,#10507,.T.);
#15031=EDGE_CURVE('',#12190,#12190,#10508,.T.);
#15032=EDGE_CURVE('',#12190,#12182,#2271,.T.);
#15033=EDGE_CURVE('',#12116,#12191,#10509,.T.);
#15034=EDGE_CURVE('',#12191,#12192,#10510,.T.);
#15035=EDGE_CURVE('',#12192,#12191,#10511,.T.);
#15036=EDGE_CURVE('',#12193,#12193,#10512,.T.);
#15037=EDGE_CURVE('',#12193,#12192,#2272,.T.);
#15038=EDGE_CURVE('',#12190,#12194,#10513,.T.);
#15039=EDGE_CURVE('',#12194,#12194,#10514,.T.);
#15040=EDGE_CURVE('',#12195,#12196,#10515,.T.);
#15041=EDGE_CURVE('',#12196,#12197,#2273,.T.);
#15042=EDGE_CURVE('',#12197,#12198,#10516,.T.);
#15043=EDGE_CURVE('',#12198,#12195,#2274,.T.);
#15044=EDGE_CURVE('',#12199,#12200,#10517,.T.);
#15045=EDGE_CURVE('',#12200,#12198,#10518,.T.);
#15046=EDGE_CURVE('',#12197,#12199,#10519,.T.);
#15047=EDGE_CURVE('',#12201,#12202,#10520,.T.);
#15048=EDGE_CURVE('',#12202,#12200,#2275,.T.);
#15049=EDGE_CURVE('',#12199,#12201,#2276,.T.);
#15050=EDGE_CURVE('',#12203,#12204,#10521,.T.);
#15051=EDGE_CURVE('',#12204,#12202,#10522,.T.);
#15052=EDGE_CURVE('',#12201,#12203,#10523,.T.);
#15053=EDGE_CURVE('',#12205,#12206,#10524,.T.);
#15054=EDGE_CURVE('',#12206,#12204,#2277,.T.);
#15055=EDGE_CURVE('',#12203,#12205,#2278,.T.);
#15056=EDGE_CURVE('',#12207,#12208,#10525,.T.);
#15057=EDGE_CURVE('',#12208,#12206,#10526,.T.);
#15058=EDGE_CURVE('',#12205,#12207,#10527,.T.);
#15059=EDGE_CURVE('',#12209,#12210,#10528,.T.);
#15060=EDGE_CURVE('',#12210,#12208,#2279,.T.);
#15061=EDGE_CURVE('',#12207,#12209,#2280,.T.);
#15062=EDGE_CURVE('',#12195,#12210,#10529,.T.);
#15063=EDGE_CURVE('',#12209,#12196,#10530,.T.);
#15064=EDGE_CURVE('',#12201,#12211,#2281,.T.);
#15065=EDGE_CURVE('',#12212,#12211,#10531,.T.);
#15066=EDGE_CURVE('',#12203,#12212,#2282,.T.);
#15067=EDGE_CURVE('',#12199,#12213,#2283,.T.);
#15068=EDGE_CURVE('',#12211,#12213,#2284,.T.);
#15069=EDGE_CURVE('',#12197,#12214,#2285,.T.);
#15070=EDGE_CURVE('',#12213,#12214,#10532,.T.);
#15071=EDGE_CURVE('',#12196,#12215,#2286,.T.);
#15072=EDGE_CURVE('',#12214,#12215,#2287,.T.);
#15073=EDGE_CURVE('',#12216,#12217,#2288,.T.);
#15074=EDGE_CURVE('',#12216,#12164,#2289,.T.);
#15075=EDGE_CURVE('',#12217,#12161,#2290,.T.);
#15076=EDGE_CURVE('',#12218,#12214,#10533,.T.);
#15077=EDGE_CURVE('',#12215,#12219,#10534,.T.);
#15078=EDGE_CURVE('',#12219,#12218,#2291,.T.);
#15079=EDGE_CURVE('',#12220,#12221,#10535,.T.);
#15080=EDGE_CURVE('',#12221,#12219,#10536,.T.);
#15081=EDGE_CURVE('',#12215,#12220,#10537,.T.);
#15082=EDGE_CURVE('',#12222,#12223,#10538,.T.);
#15083=EDGE_CURVE('',#12223,#12221,#2292,.T.);
#15084=EDGE_CURVE('',#12220,#12222,#2293,.T.);
#15085=EDGE_CURVE('',#12224,#12225,#10539,.T.);
#15086=EDGE_CURVE('',#12225,#12223,#10540,.T.);
#15087=EDGE_CURVE('',#12222,#12224,#10541,.T.);
#15088=EDGE_CURVE('',#12212,#12226,#10542,.T.);
#15089=EDGE_CURVE('',#12226,#12225,#2294,.T.);
#15090=EDGE_CURVE('',#12224,#12212,#2295,.T.);
#15091=EDGE_CURVE('',#12211,#12227,#10543,.T.);
#15092=EDGE_CURVE('',#12227,#12226,#10544,.T.);
#15093=EDGE_CURVE('',#12213,#12228,#10545,.T.);
#15094=EDGE_CURVE('',#12228,#12227,#2296,.T.);
#15095=EDGE_CURVE('',#12218,#12228,#10546,.T.);
#15096=EDGE_CURVE('',#12205,#12224,#2297,.T.);
#15097=EDGE_CURVE('',#12207,#12222,#2298,.T.);
#15098=EDGE_CURVE('',#12209,#12220,#2299,.T.);
#15099=EDGE_CURVE('',#12028,#12185,#2300,.T.);
#15100=EDGE_CURVE('',#12021,#12188,#2301,.T.);
#15101=EDGE_CURVE('',#12229,#12092,#10547,.T.);
#15102=EDGE_CURVE('',#12093,#12230,#10548,.T.);
#15103=EDGE_CURVE('',#12230,#12229,#2302,.T.);
#15104=EDGE_CURVE('',#12231,#12232,#10549,.T.);
#15105=EDGE_CURVE('',#12232,#12230,#10550,.T.);
#15106=EDGE_CURVE('',#12093,#12231,#10551,.T.);
#15107=EDGE_CURVE('',#12233,#12234,#10552,.T.);
#15108=EDGE_CURVE('',#12234,#12232,#2303,.T.);
#15109=EDGE_CURVE('',#12231,#12233,#2304,.T.);
#15110=EDGE_CURVE('',#12216,#12235,#10553,.T.);
#15111=EDGE_CURVE('',#12235,#12234,#10554,.T.);
#15112=EDGE_CURVE('',#12233,#12216,#10555,.T.);
#15113=EDGE_CURVE('',#12217,#12236,#10556,.T.);
#15114=EDGE_CURVE('',#12236,#12235,#2305,.T.);
#15115=EDGE_CURVE('',#12237,#12238,#10557,.T.);
#15116=EDGE_CURVE('',#12238,#12236,#10558,.T.);
#15117=EDGE_CURVE('',#12217,#12237,#10559,.T.);
#15118=EDGE_CURVE('',#12239,#12240,#10560,.T.);
#15119=EDGE_CURVE('',#12240,#12238,#2306,.T.);
#15120=EDGE_CURVE('',#12237,#12239,#2307,.T.);
#15121=EDGE_CURVE('',#12239,#12092,#10561,.T.);
#15122=EDGE_CURVE('',#12229,#12240,#10562,.T.);
#15123=EDGE_CURVE('',#12233,#12165,#2308,.T.);
#15124=EDGE_CURVE('',#12231,#12156,#2309,.T.);
#15125=EDGE_CURVE('',#12155,#12241,#10563,.T.);
#15126=EDGE_CURVE('',#12241,#12242,#2310,.T.);
#15127=EDGE_CURVE('',#12242,#12243,#10564,.T.);
#15128=EDGE_CURVE('',#12243,#12244,#2311,.T.);
#15129=EDGE_CURVE('',#12244,#12245,#10565,.T.);
#15130=EDGE_CURVE('',#12245,#12246,#2312,.T.);
#15131=EDGE_CURVE('',#12246,#12166,#10566,.T.);
#15132=EDGE_CURVE('',#12247,#12247,#10567,.T.);
#15133=EDGE_CURVE('',#12103,#12248,#10568,.T.);
#15134=EDGE_CURVE('',#12248,#12249,#2313,.T.);
#15135=EDGE_CURVE('',#12249,#12102,#10569,.T.);
#15136=EDGE_CURVE('',#12250,#12104,#10570,.T.);
#15137=EDGE_CURVE('',#12249,#12250,#10571,.T.);
#15138=EDGE_CURVE('',#12251,#12105,#10572,.T.);
#15139=EDGE_CURVE('',#12250,#12251,#2314,.T.);
#15140=EDGE_CURVE('',#12252,#12106,#10573,.T.);
#15141=EDGE_CURVE('',#12251,#12252,#10574,.T.);
#15142=EDGE_CURVE('',#12253,#12107,#10575,.T.);
#15143=EDGE_CURVE('',#12252,#12253,#2315,.T.);
#15144=EDGE_CURVE('',#12254,#12108,#10576,.T.);
#15145=EDGE_CURVE('',#12253,#12254,#10577,.T.);
#15146=EDGE_CURVE('',#12255,#12109,#10578,.T.);
#15147=EDGE_CURVE('',#12254,#12255,#2316,.T.);
#15148=EDGE_CURVE('',#12255,#12248,#10579,.T.);
#15149=EDGE_CURVE('',#12251,#12256,#2317,.T.);
#15150=EDGE_CURVE('',#12257,#12256,#10580,.T.);
#15151=EDGE_CURVE('',#12252,#12257,#2318,.T.);
#15152=EDGE_CURVE('',#12250,#12258,#2319,.T.);
#15153=EDGE_CURVE('',#12256,#12258,#2320,.T.);
#15154=EDGE_CURVE('',#12249,#12259,#2321,.T.);
#15155=EDGE_CURVE('',#12258,#12259,#10581,.T.);
#15156=EDGE_CURVE('',#12248,#12260,#2322,.T.);
#15157=EDGE_CURVE('',#12259,#12260,#2323,.T.);
#15158=EDGE_CURVE('',#12070,#12259,#10582,.T.);
#15159=EDGE_CURVE('',#12260,#12069,#10583,.T.);
#15160=EDGE_CURVE('',#12261,#12071,#10584,.T.);
#15161=EDGE_CURVE('',#12260,#12261,#10585,.T.);
#15162=EDGE_CURVE('',#12262,#12072,#10586,.T.);
#15163=EDGE_CURVE('',#12261,#12262,#2324,.T.);
#15164=EDGE_CURVE('',#12263,#12073,#10587,.T.);
#15165=EDGE_CURVE('',#12262,#12263,#10588,.T.);
#15166=EDGE_CURVE('',#12257,#12074,#10589,.T.);
#15167=EDGE_CURVE('',#12263,#12257,#2325,.T.);
#15168=EDGE_CURVE('',#12256,#12075,#10590,.T.);
#15169=EDGE_CURVE('',#12258,#12076,#10591,.T.);
#15170=EDGE_CURVE('',#12253,#12263,#2326,.T.);
#15171=EDGE_CURVE('',#12254,#12262,#2327,.T.);
#15172=EDGE_CURVE('',#12255,#12261,#2328,.T.);
#15173=EDGE_CURVE('',#12138,#12148,#2329,.T.);
#15174=EDGE_CURVE('',#12139,#12147,#2330,.T.);
#15175=EDGE_CURVE('',#12140,#12146,#2331,.T.);
#15176=EDGE_CURVE('',#12141,#12145,#2332,.T.);
#15177=EDGE_CURVE('',#12264,#12264,#10592,.T.);
#15178=EDGE_CURVE('',#12265,#12265,#10593,.T.);
#15179=EDGE_CURVE('',#12264,#12030,#2333,.T.);
#15180=EDGE_CURVE('',#12266,#12266,#10594,.T.);
#15181=EDGE_CURVE('',#12267,#12267,#10595,.T.);
#15182=EDGE_CURVE('',#12266,#12265,#2334,.T.);
#15183=EDGE_CURVE('',#12027,#12186,#2335,.T.);
#15184=EDGE_CURVE('',#12026,#12189,#2336,.T.);
#15185=EDGE_CURVE('',#12022,#12187,#2337,.T.);
#15186=EDGE_CURVE('',#12176,#12036,#2338,.T.);
#15187=EDGE_CURVE('',#12175,#12035,#2339,.T.);
#15188=EDGE_CURVE('',#12174,#12034,#2340,.T.);
#15189=EDGE_CURVE('',#12044,#12243,#2341,.T.);
#15190=EDGE_CURVE('',#12045,#12244,#2342,.T.);
#15191=EDGE_CURVE('',#12046,#12242,#2343,.T.);
#15192=EDGE_CURVE('',#12047,#12241,#2344,.T.);
#15193=EDGE_CURVE('',#12048,#12154,#2345,.T.);
#15194=EDGE_CURVE('',#12049,#12167,#2346,.T.);
#15195=EDGE_CURVE('',#12050,#12246,#2347,.T.);
#15196=EDGE_CURVE('',#12051,#12245,#2348,.T.);
#15197=EDGE_CURVE('',#12237,#12160,#2349,.T.);
#15198=EDGE_CURVE('',#12239,#12157,#2350,.T.);
#15199=EDGE_CURVE('',#12267,#12144,#2351,.T.);
#15200=EDGE_CURVE('',#12247,#12142,#2352,.T.);
#15201=EDGE_CURVE('',#12268,#12269,#202,.T.);
#15202=EDGE_CURVE('',#12269,#12270,#2353,.T.);
#15203=EDGE_CURVE('',#12270,#12271,#2354,.F.);
#15204=EDGE_CURVE('',#12271,#12268,#2355,.T.);
#15205=EDGE_CURVE('',#12272,#12269,#2356,.T.);
#15206=EDGE_CURVE('',#12272,#12273,#2357,.T.);
#15207=EDGE_CURVE('',#12270,#12273,#2358,.T.);
#15208=EDGE_CURVE('',#12274,#12268,#10596,.T.);
#15209=EDGE_CURVE('',#12275,#12274,#203,.T.);
#15210=EDGE_CURVE('',#12275,#12276,#2359,.T.);
#15211=EDGE_CURVE('',#12276,#12277,#10597,.T.);
#15212=EDGE_CURVE('',#12277,#12278,#2360,.T.);
#15213=EDGE_CURVE('',#12279,#12278,#204,.T.);
#15214=EDGE_CURVE('',#12280,#12279,#10598,.T.);
#15215=EDGE_CURVE('',#12281,#12280,#205,.T.);
#15216=EDGE_CURVE('',#12281,#12282,#2361,.T.);
#15217=EDGE_CURVE('',#12282,#12283,#10599,.T.);
#15218=EDGE_CURVE('',#12283,#12284,#2362,.T.);
#15219=EDGE_CURVE('',#12285,#12284,#206,.T.);
#15220=EDGE_CURVE('',#12286,#12285,#10600,.T.);
#15221=EDGE_CURVE('',#12286,#12287,#2363,.T.);
#15222=EDGE_CURVE('',#12287,#12288,#10601,.T.);
#15223=EDGE_CURVE('',#12289,#12288,#207,.T.);
#15224=EDGE_CURVE('',#12289,#12290,#2364,.T.);
#15225=EDGE_CURVE('',#12290,#12291,#10602,.T.);
#15226=EDGE_CURVE('',#12291,#12292,#2365,.T.);
#15227=EDGE_CURVE('',#12293,#12292,#208,.T.);
#15228=EDGE_CURVE('',#12293,#12294,#10603,.T.);
#15229=EDGE_CURVE('',#12295,#12294,#209,.T.);
#15230=EDGE_CURVE('',#12295,#12296,#2366,.T.);
#15231=EDGE_CURVE('',#12296,#12297,#10604,.T.);
#15232=EDGE_CURVE('',#12297,#12298,#2367,.T.);
#15233=EDGE_CURVE('',#12299,#12298,#210,.T.);
#15234=EDGE_CURVE('',#12299,#12300,#10605,.T.);
#15235=EDGE_CURVE('',#12301,#12300,#211,.T.);
#15236=EDGE_CURVE('',#12301,#12302,#2368,.T.);
#15237=EDGE_CURVE('',#12302,#12303,#10606,.T.);
#15238=EDGE_CURVE('',#12303,#12304,#2369,.T.);
#15239=EDGE_CURVE('',#12305,#12304,#212,.T.);
#15240=EDGE_CURVE('',#12305,#12306,#10607,.T.);
#15241=EDGE_CURVE('',#12307,#12306,#213,.T.);
#15242=EDGE_CURVE('',#12307,#12308,#2370,.T.);
#15243=EDGE_CURVE('',#12308,#12309,#10608,.T.);
#15244=EDGE_CURVE('',#12309,#12310,#2371,.T.);
#15245=EDGE_CURVE('',#12311,#12310,#214,.T.);
#15246=EDGE_CURVE('',#12311,#12312,#10609,.T.);
#15247=EDGE_CURVE('',#12313,#12312,#215,.T.);
#15248=EDGE_CURVE('',#12313,#12314,#2372,.T.);
#15249=EDGE_CURVE('',#12314,#12315,#10610,.T.);
#15250=EDGE_CURVE('',#12315,#12316,#2373,.T.);
#15251=EDGE_CURVE('',#12317,#12316,#216,.T.);
#15252=EDGE_CURVE('',#12317,#12318,#10611,.T.);
#15253=EDGE_CURVE('',#12319,#12318,#217,.T.);
#15254=EDGE_CURVE('',#12319,#12320,#2374,.T.);
#15255=EDGE_CURVE('',#12320,#12321,#10612,.T.);
#15256=EDGE_CURVE('',#12321,#12322,#2375,.T.);
#15257=EDGE_CURVE('',#12323,#12322,#218,.T.);
#15258=EDGE_CURVE('',#12323,#12324,#10613,.T.);
#15259=EDGE_CURVE('',#12325,#12324,#219,.T.);
#15260=EDGE_CURVE('',#12325,#12326,#2376,.T.);
#15261=EDGE_CURVE('',#12326,#12327,#10614,.T.);
#15262=EDGE_CURVE('',#12327,#12328,#2377,.T.);
#15263=EDGE_CURVE('',#12329,#12328,#220,.T.);
#15264=EDGE_CURVE('',#12329,#12330,#10615,.T.);
#15265=EDGE_CURVE('',#12331,#12330,#221,.T.);
#15266=EDGE_CURVE('',#12331,#12332,#2378,.T.);
#15267=EDGE_CURVE('',#12332,#12333,#10616,.T.);
#15268=EDGE_CURVE('',#12333,#12334,#2379,.T.);
#15269=EDGE_CURVE('',#12335,#12334,#222,.T.);
#15270=EDGE_CURVE('',#12335,#12336,#10617,.T.);
#15271=EDGE_CURVE('',#12337,#12336,#223,.T.);
#15272=EDGE_CURVE('',#12337,#12338,#2380,.T.);
#15273=EDGE_CURVE('',#12338,#12339,#10618,.T.);
#15274=EDGE_CURVE('',#12339,#12340,#2381,.T.);
#15275=EDGE_CURVE('',#12341,#12340,#224,.T.);
#15276=EDGE_CURVE('',#12341,#12342,#10619,.T.);
#15277=EDGE_CURVE('',#12343,#12342,#225,.T.);
#15278=EDGE_CURVE('',#12343,#12344,#2382,.T.);
#15279=EDGE_CURVE('',#12344,#12345,#10620,.T.);
#15280=EDGE_CURVE('',#12345,#12346,#2383,.T.);
#15281=EDGE_CURVE('',#12347,#12346,#226,.T.);
#15282=EDGE_CURVE('',#12347,#12348,#10621,.T.);
#15283=EDGE_CURVE('',#12349,#12348,#227,.T.);
#15284=EDGE_CURVE('',#12349,#12350,#2384,.T.);
#15285=EDGE_CURVE('',#12350,#12351,#10622,.T.);
#15286=EDGE_CURVE('',#12351,#12352,#2385,.T.);
#15287=EDGE_CURVE('',#12353,#12352,#228,.T.);
#15288=EDGE_CURVE('',#12353,#12354,#10623,.T.);
#15289=EDGE_CURVE('',#12355,#12354,#229,.T.);
#15290=EDGE_CURVE('',#12355,#12356,#2386,.T.);
#15291=EDGE_CURVE('',#12356,#12357,#10624,.T.);
#15292=EDGE_CURVE('',#12357,#12358,#2387,.T.);
#15293=EDGE_CURVE('',#12359,#12358,#230,.T.);
#15294=EDGE_CURVE('',#12359,#12360,#10625,.T.);
#15295=EDGE_CURVE('',#12361,#12360,#231,.T.);
#15296=EDGE_CURVE('',#12361,#12362,#2388,.T.);
#15297=EDGE_CURVE('',#12362,#12363,#10626,.T.);
#15298=EDGE_CURVE('',#12363,#12364,#2389,.T.);
#15299=EDGE_CURVE('',#12365,#12364,#232,.T.);
#15300=EDGE_CURVE('',#12365,#12366,#10627,.T.);
#15301=EDGE_CURVE('',#12367,#12366,#233,.T.);
#15302=EDGE_CURVE('',#12367,#12368,#2390,.T.);
#15303=EDGE_CURVE('',#12368,#12369,#10628,.T.);
#15304=EDGE_CURVE('',#12369,#12370,#2391,.T.);
#15305=EDGE_CURVE('',#12371,#12370,#234,.T.);
#15306=EDGE_CURVE('',#12371,#12372,#10629,.T.);
#15307=EDGE_CURVE('',#12373,#12372,#235,.T.);
#15308=EDGE_CURVE('',#12373,#12374,#2392,.T.);
#15309=EDGE_CURVE('',#12374,#12375,#10630,.T.);
#15310=EDGE_CURVE('',#12375,#12376,#2393,.T.);
#15311=EDGE_CURVE('',#12377,#12376,#236,.T.);
#15312=EDGE_CURVE('',#12377,#12378,#10631,.T.);
#15313=EDGE_CURVE('',#12379,#12378,#237,.T.);
#15314=EDGE_CURVE('',#12379,#12380,#2394,.T.);
#15315=EDGE_CURVE('',#12380,#12381,#10632,.T.);
#15316=EDGE_CURVE('',#12381,#12382,#2395,.T.);
#15317=EDGE_CURVE('',#12383,#12382,#238,.T.);
#15318=EDGE_CURVE('',#12383,#12384,#10633,.T.);
#15319=EDGE_CURVE('',#12385,#12384,#239,.T.);
#15320=EDGE_CURVE('',#12385,#12386,#2396,.T.);
#15321=EDGE_CURVE('',#12386,#12387,#10634,.T.);
#15322=EDGE_CURVE('',#12387,#12388,#2397,.T.);
#15323=EDGE_CURVE('',#12389,#12388,#240,.T.);
#15324=EDGE_CURVE('',#12389,#12390,#10635,.T.);
#15325=EDGE_CURVE('',#12391,#12390,#241,.T.);
#15326=EDGE_CURVE('',#12391,#12392,#2398,.T.);
#15327=EDGE_CURVE('',#12392,#12393,#10636,.T.);
#15328=EDGE_CURVE('',#12393,#12394,#2399,.T.);
#15329=EDGE_CURVE('',#12395,#12394,#242,.T.);
#15330=EDGE_CURVE('',#12395,#12396,#10637,.T.);
#15331=EDGE_CURVE('',#12397,#12396,#243,.T.);
#15332=EDGE_CURVE('',#12397,#12398,#2400,.T.);
#15333=EDGE_CURVE('',#12398,#12399,#10638,.T.);
#15334=EDGE_CURVE('',#12399,#12400,#2401,.T.);
#15335=EDGE_CURVE('',#12401,#12400,#244,.T.);
#15336=EDGE_CURVE('',#12401,#12402,#10639,.T.);
#15337=EDGE_CURVE('',#12403,#12402,#245,.T.);
#15338=EDGE_CURVE('',#12403,#12404,#2402,.T.);
#15339=EDGE_CURVE('',#12404,#12405,#10640,.T.);
#15340=EDGE_CURVE('',#12405,#12406,#2403,.T.);
#15341=EDGE_CURVE('',#12407,#12406,#246,.T.);
#15342=EDGE_CURVE('',#12407,#12408,#10641,.T.);
#15343=EDGE_CURVE('',#12409,#12408,#247,.T.);
#15344=EDGE_CURVE('',#12409,#12410,#2404,.T.);
#15345=EDGE_CURVE('',#12410,#12411,#10642,.T.);
#15346=EDGE_CURVE('',#12411,#12412,#2405,.T.);
#15347=EDGE_CURVE('',#12413,#12412,#248,.T.);
#15348=EDGE_CURVE('',#12413,#12414,#10643,.T.);
#15349=EDGE_CURVE('',#12415,#12414,#249,.T.);
#15350=EDGE_CURVE('',#12415,#12416,#2406,.T.);
#15351=EDGE_CURVE('',#12416,#12417,#10644,.T.);
#15352=EDGE_CURVE('',#12417,#12418,#2407,.T.);
#15353=EDGE_CURVE('',#12419,#12418,#250,.T.);
#15354=EDGE_CURVE('',#12419,#12420,#10645,.T.);
#15355=EDGE_CURVE('',#12421,#12420,#251,.T.);
#15356=EDGE_CURVE('',#12421,#12422,#2408,.T.);
#15357=EDGE_CURVE('',#12422,#12423,#10646,.T.);
#15358=EDGE_CURVE('',#12423,#12424,#2409,.T.);
#15359=EDGE_CURVE('',#12425,#12424,#252,.T.);
#15360=EDGE_CURVE('',#12425,#12426,#10647,.T.);
#15361=EDGE_CURVE('',#12427,#12426,#253,.T.);
#15362=EDGE_CURVE('',#12427,#12428,#2410,.T.);
#15363=EDGE_CURVE('',#12428,#12429,#10648,.T.);
#15364=EDGE_CURVE('',#12429,#12430,#2411,.T.);
#15365=EDGE_CURVE('',#12431,#12430,#254,.T.);
#15366=EDGE_CURVE('',#12431,#12432,#10649,.T.);
#15367=EDGE_CURVE('',#12433,#12432,#255,.T.);
#15368=EDGE_CURVE('',#12433,#12434,#2412,.T.);
#15369=EDGE_CURVE('',#12434,#12435,#10650,.T.);
#15370=EDGE_CURVE('',#12435,#12436,#2413,.T.);
#15371=EDGE_CURVE('',#12437,#12436,#256,.T.);
#15372=EDGE_CURVE('',#12437,#12438,#10651,.T.);
#15373=EDGE_CURVE('',#12439,#12438,#257,.T.);
#15374=EDGE_CURVE('',#12439,#12440,#2414,.T.);
#15375=EDGE_CURVE('',#12440,#12441,#10652,.T.);
#15376=EDGE_CURVE('',#12441,#12442,#2415,.T.);
#15377=EDGE_CURVE('',#12443,#12442,#258,.T.);
#15378=EDGE_CURVE('',#12443,#12444,#10653,.T.);
#15379=EDGE_CURVE('',#12445,#12444,#259,.T.);
#15380=EDGE_CURVE('',#12445,#12446,#2416,.T.);
#15381=EDGE_CURVE('',#12446,#12447,#10654,.T.);
#15382=EDGE_CURVE('',#12447,#12448,#2417,.T.);
#15383=EDGE_CURVE('',#12449,#12448,#260,.T.);
#15384=EDGE_CURVE('',#12449,#12450,#10655,.T.);
#15385=EDGE_CURVE('',#12451,#12450,#261,.T.);
#15386=EDGE_CURVE('',#12451,#12452,#2418,.T.);
#15387=EDGE_CURVE('',#12452,#12453,#10656,.T.);
#15388=EDGE_CURVE('',#12453,#12454,#2419,.T.);
#15389=EDGE_CURVE('',#12455,#12454,#262,.T.);
#15390=EDGE_CURVE('',#12455,#12456,#10657,.T.);
#15391=EDGE_CURVE('',#12457,#12456,#263,.T.);
#15392=EDGE_CURVE('',#12457,#12458,#2420,.T.);
#15393=EDGE_CURVE('',#12458,#12459,#10658,.T.);
#15394=EDGE_CURVE('',#12459,#12460,#2421,.T.);
#15395=EDGE_CURVE('',#12461,#12460,#264,.T.);
#15396=EDGE_CURVE('',#12461,#12462,#10659,.T.);
#15397=EDGE_CURVE('',#12463,#12462,#265,.T.);
#15398=EDGE_CURVE('',#12463,#12464,#2422,.T.);
#15399=EDGE_CURVE('',#12464,#12465,#10660,.T.);
#15400=EDGE_CURVE('',#12465,#12466,#2423,.T.);
#15401=EDGE_CURVE('',#12467,#12466,#266,.T.);
#15402=EDGE_CURVE('',#12467,#12287,#10661,.T.);
#15403=EDGE_CURVE('',#12468,#12286,#10662,.T.);
#15404=EDGE_CURVE('',#12469,#12468,#267,.T.);
#15405=EDGE_CURVE('',#12469,#12470,#2424,.T.);
#15406=EDGE_CURVE('',#12470,#12471,#10663,.T.);
#15407=EDGE_CURVE('',#12471,#12472,#2425,.T.);
#15408=EDGE_CURVE('',#12473,#12472,#268,.T.);
#15409=EDGE_CURVE('',#12474,#12473,#10664,.T.);
#15410=EDGE_CURVE('',#12475,#12474,#269,.T.);
#15411=EDGE_CURVE('',#12475,#12476,#2426,.T.);
#15412=EDGE_CURVE('',#12476,#12477,#10665,.T.);
#15413=EDGE_CURVE('',#12477,#12478,#2427,.T.);
#15414=EDGE_CURVE('',#12479,#12478,#270,.T.);
#15415=EDGE_CURVE('',#12480,#12479,#10666,.T.);
#15416=EDGE_CURVE('',#12481,#12480,#271,.T.);
#15417=EDGE_CURVE('',#12481,#12482,#2428,.T.);
#15418=EDGE_CURVE('',#12482,#12483,#10667,.T.);
#15419=EDGE_CURVE('',#12483,#12484,#2429,.T.);
#15420=EDGE_CURVE('',#12485,#12484,#272,.T.);
#15421=EDGE_CURVE('',#12486,#12485,#10668,.T.);
#15422=EDGE_CURVE('',#12487,#12486,#273,.T.);
#15423=EDGE_CURVE('',#12487,#12488,#2430,.T.);
#15424=EDGE_CURVE('',#12488,#12489,#10669,.T.);
#15425=EDGE_CURVE('',#12489,#12490,#2431,.T.);
#15426=EDGE_CURVE('',#12491,#12490,#274,.T.);
#15427=EDGE_CURVE('',#12492,#12491,#10670,.T.);
#15428=EDGE_CURVE('',#12493,#12492,#275,.T.);
#15429=EDGE_CURVE('',#12493,#12494,#2432,.T.);
#15430=EDGE_CURVE('',#12494,#12495,#10671,.T.);
#15431=EDGE_CURVE('',#12495,#12496,#2433,.T.);
#15432=EDGE_CURVE('',#12497,#12496,#276,.T.);
#15433=EDGE_CURVE('',#12498,#12497,#10672,.T.);
#15434=EDGE_CURVE('',#12499,#12498,#277,.T.);
#15435=EDGE_CURVE('',#12499,#12500,#2434,.T.);
#15436=EDGE_CURVE('',#12500,#12501,#10673,.T.);
#15437=EDGE_CURVE('',#12501,#12502,#2435,.T.);
#15438=EDGE_CURVE('',#12503,#12502,#278,.T.);
#15439=EDGE_CURVE('',#12504,#12503,#10674,.T.);
#15440=EDGE_CURVE('',#12505,#12504,#279,.T.);
#15441=EDGE_CURVE('',#12505,#12506,#2436,.T.);
#15442=EDGE_CURVE('',#12506,#12507,#10675,.T.);
#15443=EDGE_CURVE('',#12507,#12508,#2437,.T.);
#15444=EDGE_CURVE('',#12509,#12508,#280,.T.);
#15445=EDGE_CURVE('',#12510,#12509,#10676,.T.);
#15446=EDGE_CURVE('',#12511,#12510,#281,.T.);
#15447=EDGE_CURVE('',#12511,#12512,#2438,.T.);
#15448=EDGE_CURVE('',#12512,#12513,#10677,.T.);
#15449=EDGE_CURVE('',#12513,#12514,#2439,.T.);
#15450=EDGE_CURVE('',#12515,#12514,#282,.T.);
#15451=EDGE_CURVE('',#12516,#12515,#10678,.T.);
#15452=EDGE_CURVE('',#12517,#12516,#283,.T.);
#15453=EDGE_CURVE('',#12517,#12518,#2440,.T.);
#15454=EDGE_CURVE('',#12518,#12519,#10679,.T.);
#15455=EDGE_CURVE('',#12519,#12520,#2441,.T.);
#15456=EDGE_CURVE('',#12521,#12520,#284,.T.);
#15457=EDGE_CURVE('',#12522,#12521,#10680,.T.);
#15458=EDGE_CURVE('',#12523,#12522,#285,.T.);
#15459=EDGE_CURVE('',#12523,#12524,#2442,.T.);
#15460=EDGE_CURVE('',#12524,#12525,#10681,.T.);
#15461=EDGE_CURVE('',#12525,#12526,#2443,.T.);
#15462=EDGE_CURVE('',#12527,#12526,#286,.T.);
#15463=EDGE_CURVE('',#12528,#12527,#10682,.T.);
#15464=EDGE_CURVE('',#12529,#12528,#287,.T.);
#15465=EDGE_CURVE('',#12529,#12530,#2444,.T.);
#15466=EDGE_CURVE('',#12530,#12531,#10683,.T.);
#15467=EDGE_CURVE('',#12531,#12532,#2445,.T.);
#15468=EDGE_CURVE('',#12533,#12532,#288,.T.);
#15469=EDGE_CURVE('',#12534,#12533,#10684,.T.);
#15470=EDGE_CURVE('',#12535,#12534,#289,.T.);
#15471=EDGE_CURVE('',#12535,#12536,#2446,.T.);
#15472=EDGE_CURVE('',#12536,#12537,#10685,.T.);
#15473=EDGE_CURVE('',#12537,#12538,#2447,.T.);
#15474=EDGE_CURVE('',#12539,#12538,#290,.T.);
#15475=EDGE_CURVE('',#12540,#12539,#10686,.T.);
#15476=EDGE_CURVE('',#12541,#12540,#291,.T.);
#15477=EDGE_CURVE('',#12541,#12542,#2448,.T.);
#15478=EDGE_CURVE('',#12542,#12543,#10687,.T.);
#15479=EDGE_CURVE('',#12543,#12544,#2449,.T.);
#15480=EDGE_CURVE('',#12545,#12544,#292,.T.);
#15481=EDGE_CURVE('',#12546,#12545,#10688,.T.);
#15482=EDGE_CURVE('',#12547,#12546,#293,.T.);
#15483=EDGE_CURVE('',#12547,#12548,#2450,.T.);
#15484=EDGE_CURVE('',#12548,#12549,#10689,.T.);
#15485=EDGE_CURVE('',#12549,#12550,#2451,.T.);
#15486=EDGE_CURVE('',#12551,#12550,#294,.T.);
#15487=EDGE_CURVE('',#12552,#12551,#10690,.T.);
#15488=EDGE_CURVE('',#12553,#12552,#295,.T.);
#15489=EDGE_CURVE('',#12553,#12554,#2452,.T.);
#15490=EDGE_CURVE('',#12554,#12555,#10691,.T.);
#15491=EDGE_CURVE('',#12555,#12556,#2453,.T.);
#15492=EDGE_CURVE('',#12557,#12556,#296,.T.);
#15493=EDGE_CURVE('',#12558,#12557,#10692,.T.);
#15494=EDGE_CURVE('',#12559,#12558,#297,.T.);
#15495=EDGE_CURVE('',#12559,#12560,#2454,.T.);
#15496=EDGE_CURVE('',#12560,#12561,#10693,.T.);
#15497=EDGE_CURVE('',#12561,#12562,#2455,.T.);
#15498=EDGE_CURVE('',#12563,#12562,#298,.T.);
#15499=EDGE_CURVE('',#12564,#12563,#10694,.T.);
#15500=EDGE_CURVE('',#12565,#12564,#299,.T.);
#15501=EDGE_CURVE('',#12565,#12566,#2456,.T.);
#15502=EDGE_CURVE('',#12566,#12567,#10695,.T.);
#15503=EDGE_CURVE('',#12567,#12568,#2457,.T.);
#15504=EDGE_CURVE('',#12569,#12568,#300,.T.);
#15505=EDGE_CURVE('',#12570,#12569,#10696,.T.);
#15506=EDGE_CURVE('',#12571,#12570,#301,.T.);
#15507=EDGE_CURVE('',#12571,#12572,#2458,.T.);
#15508=EDGE_CURVE('',#12572,#12573,#10697,.T.);
#15509=EDGE_CURVE('',#12573,#12574,#2459,.T.);
#15510=EDGE_CURVE('',#12575,#12574,#302,.T.);
#15511=EDGE_CURVE('',#12576,#12575,#10698,.T.);
#15512=EDGE_CURVE('',#12577,#12576,#303,.T.);
#15513=EDGE_CURVE('',#12577,#12578,#2460,.T.);
#15514=EDGE_CURVE('',#12578,#12579,#10699,.T.);
#15515=EDGE_CURVE('',#12579,#12580,#2461,.T.);
#15516=EDGE_CURVE('',#12581,#12580,#304,.T.);
#15517=EDGE_CURVE('',#12582,#12581,#10700,.T.);
#15518=EDGE_CURVE('',#12583,#12582,#305,.T.);
#15519=EDGE_CURVE('',#12583,#12584,#2462,.T.);
#15520=EDGE_CURVE('',#12584,#12585,#10701,.T.);
#15521=EDGE_CURVE('',#12585,#12586,#2463,.T.);
#15522=EDGE_CURVE('',#12587,#12586,#306,.T.);
#15523=EDGE_CURVE('',#12588,#12587,#10702,.T.);
#15524=EDGE_CURVE('',#12589,#12588,#307,.T.);
#15525=EDGE_CURVE('',#12589,#12590,#2464,.T.);
#15526=EDGE_CURVE('',#12590,#12591,#10703,.T.);
#15527=EDGE_CURVE('',#12591,#12592,#2465,.T.);
#15528=EDGE_CURVE('',#12593,#12592,#308,.T.);
#15529=EDGE_CURVE('',#12594,#12593,#10704,.T.);
#15530=EDGE_CURVE('',#12595,#12594,#309,.T.);
#15531=EDGE_CURVE('',#12595,#12596,#2466,.T.);
#15532=EDGE_CURVE('',#12596,#12597,#10705,.T.);
#15533=EDGE_CURVE('',#12597,#12598,#2467,.T.);
#15534=EDGE_CURVE('',#12599,#12598,#310,.T.);
#15535=EDGE_CURVE('',#12600,#12599,#10706,.T.);
#15536=EDGE_CURVE('',#12601,#12600,#311,.T.);
#15537=EDGE_CURVE('',#12601,#12602,#2468,.T.);
#15538=EDGE_CURVE('',#12602,#12603,#10707,.T.);
#15539=EDGE_CURVE('',#12603,#12604,#2469,.T.);
#15540=EDGE_CURVE('',#12605,#12604,#312,.T.);
#15541=EDGE_CURVE('',#12606,#12605,#10708,.T.);
#15542=EDGE_CURVE('',#12607,#12606,#313,.T.);
#15543=EDGE_CURVE('',#12607,#12608,#2470,.T.);
#15544=EDGE_CURVE('',#12608,#12609,#10709,.T.);
#15545=EDGE_CURVE('',#12609,#12610,#2471,.T.);
#15546=EDGE_CURVE('',#12611,#12610,#314,.T.);
#15547=EDGE_CURVE('',#12612,#12611,#10710,.T.);
#15548=EDGE_CURVE('',#12613,#12612,#315,.T.);
#15549=EDGE_CURVE('',#12613,#12614,#2472,.T.);
#15550=EDGE_CURVE('',#12614,#12615,#10711,.T.);
#15551=EDGE_CURVE('',#12615,#12616,#2473,.T.);
#15552=EDGE_CURVE('',#12617,#12616,#316,.T.);
#15553=EDGE_CURVE('',#12618,#12617,#10712,.T.);
#15554=EDGE_CURVE('',#12619,#12618,#317,.T.);
#15555=EDGE_CURVE('',#12619,#12620,#2474,.T.);
#15556=EDGE_CURVE('',#12620,#12621,#10713,.T.);
#15557=EDGE_CURVE('',#12621,#12622,#2475,.T.);
#15558=EDGE_CURVE('',#12623,#12622,#318,.T.);
#15559=EDGE_CURVE('',#12624,#12623,#10714,.T.);
#15560=EDGE_CURVE('',#12625,#12624,#319,.T.);
#15561=EDGE_CURVE('',#12625,#12626,#2476,.T.);
#15562=EDGE_CURVE('',#12626,#12627,#10715,.T.);
#15563=EDGE_CURVE('',#12627,#12628,#2477,.T.);
#15564=EDGE_CURVE('',#12629,#12628,#320,.T.);
#15565=EDGE_CURVE('',#12630,#12629,#10716,.T.);
#15566=EDGE_CURVE('',#12631,#12630,#321,.T.);
#15567=EDGE_CURVE('',#12631,#12632,#2478,.T.);
#15568=EDGE_CURVE('',#12632,#12272,#10717,.T.);
#15569=EDGE_CURVE('',#12633,#12275,#2479,.T.);
#15570=EDGE_CURVE('',#12274,#12634,#2480,.T.);
#15571=EDGE_CURVE('',#12634,#12633,#2481,.T.);
#15572=EDGE_CURVE('',#12634,#12635,#2482,.T.);
#15573=EDGE_CURVE('',#12635,#12636,#2483,.T.);
#15574=EDGE_CURVE('',#12636,#12633,#2484,.T.);
#15575=EDGE_CURVE('',#12635,#12279,#2485,.T.);
#15576=EDGE_CURVE('',#12278,#12636,#2486,.T.);
#15577=EDGE_CURVE('',#12633,#12637,#2487,.T.);
#15578=EDGE_CURVE('',#12637,#12276,#2488,.T.);
#15579=EDGE_CURVE('',#12636,#12638,#2489,.T.);
#15580=EDGE_CURVE('',#12638,#12637,#2490,.T.);
#15581=EDGE_CURVE('',#12277,#12638,#2491,.T.);
#15582=EDGE_CURVE('',#12639,#12281,#2492,.T.);
#15583=EDGE_CURVE('',#12280,#12640,#2493,.T.);
#15584=EDGE_CURVE('',#12640,#12639,#2494,.T.);
#15585=EDGE_CURVE('',#12640,#12641,#2495,.T.);
#15586=EDGE_CURVE('',#12641,#12642,#2496,.T.);
#15587=EDGE_CURVE('',#12642,#12639,#2497,.T.);
#15588=EDGE_CURVE('',#12641,#12285,#2498,.T.);
#15589=EDGE_CURVE('',#12284,#12642,#2499,.T.);
#15590=EDGE_CURVE('',#12639,#12643,#2500,.T.);
#15591=EDGE_CURVE('',#12643,#12282,#2501,.T.);
#15592=EDGE_CURVE('',#12642,#12644,#2502,.T.);
#15593=EDGE_CURVE('',#12644,#12643,#2503,.T.);
#15594=EDGE_CURVE('',#12283,#12644,#2504,.T.);
#15595=EDGE_CURVE('',#12645,#12469,#2505,.T.);
#15596=EDGE_CURVE('',#12468,#12646,#2506,.T.);
#15597=EDGE_CURVE('',#12646,#12645,#2507,.T.);
#15598=EDGE_CURVE('',#12646,#12647,#2508,.T.);
#15599=EDGE_CURVE('',#12647,#12648,#2509,.T.);
#15600=EDGE_CURVE('',#12648,#12645,#2510,.T.);
#15601=EDGE_CURVE('',#12647,#12473,#2511,.T.);
#15602=EDGE_CURVE('',#12472,#12648,#2512,.T.);
#15603=EDGE_CURVE('',#12645,#12649,#2513,.T.);
#15604=EDGE_CURVE('',#12649,#12470,#2514,.T.);
#15605=EDGE_CURVE('',#12648,#12650,#2515,.T.);
#15606=EDGE_CURVE('',#12650,#12649,#2516,.T.);
#15607=EDGE_CURVE('',#12471,#12650,#2517,.T.);
#15608=EDGE_CURVE('',#12651,#12475,#2518,.T.);
#15609=EDGE_CURVE('',#12474,#12652,#2519,.T.);
#15610=EDGE_CURVE('',#12652,#12651,#2520,.T.);
#15611=EDGE_CURVE('',#12652,#12653,#2521,.T.);
#15612=EDGE_CURVE('',#12653,#12654,#2522,.F.);
#15613=EDGE_CURVE('',#12654,#12651,#2523,.T.);
#15614=EDGE_CURVE('',#12651,#12655,#2524,.T.);
#15615=EDGE_CURVE('',#12655,#12476,#2525,.T.);
#15616=EDGE_CURVE('',#12654,#12656,#2526,.T.);
#15617=EDGE_CURVE('',#12656,#12655,#2527,.T.);
#15618=EDGE_CURVE('',#12478,#12654,#2528,.T.);
#15619=EDGE_CURVE('',#12653,#12479,#2529,.T.);
#15620=EDGE_CURVE('',#12657,#12271,#2530,.T.);
#15621=EDGE_CURVE('',#12630,#12657,#2531,.T.);
#15622=EDGE_CURVE('',#12658,#12629,#2532,.T.);
#15623=EDGE_CURVE('',#12659,#12658,#2533,.T.);
#15624=EDGE_CURVE('',#12624,#12659,#2534,.T.);
#15625=EDGE_CURVE('',#12660,#12623,#2535,.T.);
#15626=EDGE_CURVE('',#12661,#12660,#2536,.T.);
#15627=EDGE_CURVE('',#12618,#12661,#2537,.T.);
#15628=EDGE_CURVE('',#12662,#12617,#2538,.T.);
#15629=EDGE_CURVE('',#12663,#12662,#2539,.T.);
#15630=EDGE_CURVE('',#12612,#12663,#2540,.T.);
#15631=EDGE_CURVE('',#12664,#12611,#2541,.T.);
#15632=EDGE_CURVE('',#12665,#12664,#2542,.T.);
#15633=EDGE_CURVE('',#12606,#12665,#2543,.T.);
#15634=EDGE_CURVE('',#12666,#12605,#2544,.T.);
#15635=EDGE_CURVE('',#12667,#12666,#2545,.T.);
#15636=EDGE_CURVE('',#12600,#12667,#2546,.T.);
#15637=EDGE_CURVE('',#12668,#12599,#2547,.T.);
#15638=EDGE_CURVE('',#12669,#12668,#2548,.T.);
#15639=EDGE_CURVE('',#12594,#12669,#2549,.T.);
#15640=EDGE_CURVE('',#12670,#12593,#2550,.T.);
#15641=EDGE_CURVE('',#12671,#12670,#2551,.T.);
#15642=EDGE_CURVE('',#12588,#12671,#2552,.T.);
#15643=EDGE_CURVE('',#12672,#12587,#2553,.T.);
#15644=EDGE_CURVE('',#12673,#12672,#2554,.T.);
#15645=EDGE_CURVE('',#12582,#12673,#2555,.T.);
#15646=EDGE_CURVE('',#12674,#12581,#2556,.T.);
#15647=EDGE_CURVE('',#12675,#12674,#2557,.T.);
#15648=EDGE_CURVE('',#12576,#12675,#2558,.T.);
#15649=EDGE_CURVE('',#12676,#12575,#2559,.T.);
#15650=EDGE_CURVE('',#12677,#12676,#2560,.T.);
#15651=EDGE_CURVE('',#12570,#12677,#2561,.T.);
#15652=EDGE_CURVE('',#12678,#12569,#2562,.T.);
#15653=EDGE_CURVE('',#12679,#12678,#2563,.T.);
#15654=EDGE_CURVE('',#12564,#12679,#2564,.T.);
#15655=EDGE_CURVE('',#12680,#12563,#2565,.T.);
#15656=EDGE_CURVE('',#12681,#12680,#2566,.T.);
#15657=EDGE_CURVE('',#12558,#12681,#2567,.T.);
#15658=EDGE_CURVE('',#12682,#12557,#2568,.T.);
#15659=EDGE_CURVE('',#12683,#12682,#2569,.T.);
#15660=EDGE_CURVE('',#12552,#12683,#2570,.T.);
#15661=EDGE_CURVE('',#12684,#12551,#2571,.T.);
#15662=EDGE_CURVE('',#12685,#12684,#2572,.T.);
#15663=EDGE_CURVE('',#12546,#12685,#2573,.T.);
#15664=EDGE_CURVE('',#12686,#12545,#2574,.T.);
#15665=EDGE_CURVE('',#12687,#12686,#2575,.T.);
#15666=EDGE_CURVE('',#12540,#12687,#2576,.T.);
#15667=EDGE_CURVE('',#12688,#12539,#2577,.T.);
#15668=EDGE_CURVE('',#12689,#12688,#2578,.T.);
#15669=EDGE_CURVE('',#12534,#12689,#2579,.T.);
#15670=EDGE_CURVE('',#12690,#12533,#2580,.T.);
#15671=EDGE_CURVE('',#12691,#12690,#2581,.T.);
#15672=EDGE_CURVE('',#12528,#12691,#2582,.T.);
#15673=EDGE_CURVE('',#12692,#12527,#2583,.T.);
#15674=EDGE_CURVE('',#12693,#12692,#2584,.T.);
#15675=EDGE_CURVE('',#12522,#12693,#2585,.T.);
#15676=EDGE_CURVE('',#12694,#12521,#2586,.T.);
#15677=EDGE_CURVE('',#12695,#12694,#2587,.T.);
#15678=EDGE_CURVE('',#12516,#12695,#2588,.T.);
#15679=EDGE_CURVE('',#12696,#12515,#2589,.T.);
#15680=EDGE_CURVE('',#12697,#12696,#2590,.T.);
#15681=EDGE_CURVE('',#12510,#12697,#2591,.T.);
#15682=EDGE_CURVE('',#12698,#12509,#2592,.T.);
#15683=EDGE_CURVE('',#12699,#12698,#2593,.T.);
#15684=EDGE_CURVE('',#12504,#12699,#2594,.T.);
#15685=EDGE_CURVE('',#12700,#12503,#2595,.T.);
#15686=EDGE_CURVE('',#12701,#12700,#2596,.T.);
#15687=EDGE_CURVE('',#12498,#12701,#2597,.T.);
#15688=EDGE_CURVE('',#12702,#12497,#2598,.T.);
#15689=EDGE_CURVE('',#12703,#12702,#2599,.T.);
#15690=EDGE_CURVE('',#12492,#12703,#2600,.T.);
#15691=EDGE_CURVE('',#12704,#12491,#2601,.T.);
#15692=EDGE_CURVE('',#12705,#12704,#2602,.T.);
#15693=EDGE_CURVE('',#12486,#12705,#2603,.T.);
#15694=EDGE_CURVE('',#12706,#12485,#2604,.T.);
#15695=EDGE_CURVE('',#12707,#12706,#2605,.T.);
#15696=EDGE_CURVE('',#12480,#12707,#2606,.T.);
#15697=EDGE_CURVE('',#12708,#12709,#2607,.T.);
#15698=EDGE_CURVE('',#12710,#12708,#10718,.T.);
#15699=EDGE_CURVE('',#12711,#12710,#2608,.T.);
#15700=EDGE_CURVE('',#12712,#12711,#2609,.T.);
#15701=EDGE_CURVE('',#12713,#12712,#2610,.T.);
#15702=EDGE_CURVE('',#12714,#12713,#10719,.T.);
#15703=EDGE_CURVE('',#12715,#12714,#2611,.T.);
#15704=EDGE_CURVE('',#12709,#12715,#2612,.T.);
#15705=EDGE_CURVE('',#12716,#12481,#2613,.T.);
#15706=EDGE_CURVE('',#12707,#12716,#2614,.T.);
#15707=EDGE_CURVE('',#12706,#12717,#2615,.T.);
#15708=EDGE_CURVE('',#12717,#12716,#2616,.T.);
#15709=EDGE_CURVE('',#12484,#12717,#2617,.T.);
#15710=EDGE_CURVE('',#12718,#12487,#2618,.T.);
#15711=EDGE_CURVE('',#12705,#12718,#2619,.T.);
#15712=EDGE_CURVE('',#12704,#12719,#2620,.T.);
#15713=EDGE_CURVE('',#12719,#12718,#2621,.T.);
#15714=EDGE_CURVE('',#12490,#12719,#2622,.T.);
#15715=EDGE_CURVE('',#12720,#12493,#2623,.T.);
#15716=EDGE_CURVE('',#12703,#12720,#2624,.T.);
#15717=EDGE_CURVE('',#12702,#12721,#2625,.T.);
#15718=EDGE_CURVE('',#12721,#12720,#2626,.T.);
#15719=EDGE_CURVE('',#12496,#12721,#2627,.T.);
#15720=EDGE_CURVE('',#12722,#12499,#2628,.T.);
#15721=EDGE_CURVE('',#12701,#12722,#2629,.T.);
#15722=EDGE_CURVE('',#12700,#12723,#2630,.T.);
#15723=EDGE_CURVE('',#12723,#12722,#2631,.T.);
#15724=EDGE_CURVE('',#12502,#12723,#2632,.T.);
#15725=EDGE_CURVE('',#12724,#12505,#2633,.T.);
#15726=EDGE_CURVE('',#12699,#12724,#2634,.T.);
#15727=EDGE_CURVE('',#12698,#12725,#2635,.T.);
#15728=EDGE_CURVE('',#12725,#12724,#2636,.T.);
#15729=EDGE_CURVE('',#12508,#12725,#2637,.T.);
#15730=EDGE_CURVE('',#12726,#12511,#2638,.T.);
#15731=EDGE_CURVE('',#12697,#12726,#2639,.T.);
#15732=EDGE_CURVE('',#12696,#12727,#2640,.T.);
#15733=EDGE_CURVE('',#12727,#12726,#2641,.T.);
#15734=EDGE_CURVE('',#12514,#12727,#2642,.T.);
#15735=EDGE_CURVE('',#12270,#12728,#2643,.T.);
#15736=EDGE_CURVE('',#12728,#12657,#2644,.F.);
#15737=EDGE_CURVE('',#12273,#12729,#2645,.T.);
#15738=EDGE_CURVE('',#12728,#12729,#2646,.T.);
#15739=EDGE_CURVE('',#12728,#12631,#2647,.T.);
#15740=EDGE_CURVE('',#12730,#12625,#2648,.T.);
#15741=EDGE_CURVE('',#12659,#12730,#2649,.T.);
#15742=EDGE_CURVE('',#12731,#12730,#2650,.T.);
#15743=EDGE_CURVE('',#12658,#12731,#2651,.T.);
#15744=EDGE_CURVE('',#12628,#12731,#2652,.T.);
#15745=EDGE_CURVE('',#12730,#12732,#2653,.T.);
#15746=EDGE_CURVE('',#12732,#12626,#2654,.T.);
#15747=EDGE_CURVE('',#12731,#12733,#2655,.T.);
#15748=EDGE_CURVE('',#12733,#12732,#2656,.T.);
#15749=EDGE_CURVE('',#12627,#12733,#2657,.T.);
#15750=EDGE_CURVE('',#12734,#12619,#2658,.T.);
#15751=EDGE_CURVE('',#12661,#12734,#2659,.T.);
#15752=EDGE_CURVE('',#12735,#12734,#2660,.T.);
#15753=EDGE_CURVE('',#12660,#12735,#2661,.T.);
#15754=EDGE_CURVE('',#12622,#12735,#2662,.T.);
#15755=EDGE_CURVE('',#12734,#12736,#2663,.T.);
#15756=EDGE_CURVE('',#12736,#12620,#2664,.T.);
#15757=EDGE_CURVE('',#12735,#12737,#2665,.T.);
#15758=EDGE_CURVE('',#12737,#12736,#2666,.T.);
#15759=EDGE_CURVE('',#12621,#12737,#2667,.T.);
#15760=EDGE_CURVE('',#12738,#12613,#2668,.T.);
#15761=EDGE_CURVE('',#12663,#12738,#2669,.T.);
#15762=EDGE_CURVE('',#12739,#12738,#2670,.T.);
#15763=EDGE_CURVE('',#12662,#12739,#2671,.T.);
#15764=EDGE_CURVE('',#12616,#12739,#2672,.T.);
#15765=EDGE_CURVE('',#12738,#12740,#2673,.T.);
#15766=EDGE_CURVE('',#12740,#12614,#2674,.T.);
#15767=EDGE_CURVE('',#12739,#12741,#2675,.T.);
#15768=EDGE_CURVE('',#12741,#12740,#2676,.T.);
#15769=EDGE_CURVE('',#12615,#12741,#2677,.T.);
#15770=EDGE_CURVE('',#12742,#12607,#2678,.T.);
#15771=EDGE_CURVE('',#12665,#12742,#2679,.T.);
#15772=EDGE_CURVE('',#12743,#12742,#2680,.T.);
#15773=EDGE_CURVE('',#12664,#12743,#2681,.T.);
#15774=EDGE_CURVE('',#12610,#12743,#2682,.T.);
#15775=EDGE_CURVE('',#12742,#12744,#2683,.T.);
#15776=EDGE_CURVE('',#12744,#12608,#2684,.T.);
#15777=EDGE_CURVE('',#12743,#12745,#2685,.T.);
#15778=EDGE_CURVE('',#12745,#12744,#2686,.T.);
#15779=EDGE_CURVE('',#12609,#12745,#2687,.T.);
#15780=EDGE_CURVE('',#12746,#12601,#2688,.T.);
#15781=EDGE_CURVE('',#12667,#12746,#2689,.T.);
#15782=EDGE_CURVE('',#12747,#12746,#2690,.T.);
#15783=EDGE_CURVE('',#12666,#12747,#2691,.T.);
#15784=EDGE_CURVE('',#12604,#12747,#2692,.T.);
#15785=EDGE_CURVE('',#12746,#12748,#2693,.T.);
#15786=EDGE_CURVE('',#12748,#12602,#2694,.T.);
#15787=EDGE_CURVE('',#12747,#12749,#2695,.T.);
#15788=EDGE_CURVE('',#12749,#12748,#2696,.T.);
#15789=EDGE_CURVE('',#12603,#12749,#2697,.T.);
#15790=EDGE_CURVE('',#12750,#12595,#2698,.T.);
#15791=EDGE_CURVE('',#12669,#12750,#2699,.T.);
#15792=EDGE_CURVE('',#12751,#12750,#2700,.T.);
#15793=EDGE_CURVE('',#12668,#12751,#2701,.T.);
#15794=EDGE_CURVE('',#12598,#12751,#2702,.T.);
#15795=EDGE_CURVE('',#12750,#12752,#2703,.T.);
#15796=EDGE_CURVE('',#12752,#12596,#2704,.T.);
#15797=EDGE_CURVE('',#12751,#12753,#2705,.T.);
#15798=EDGE_CURVE('',#12753,#12752,#2706,.T.);
#15799=EDGE_CURVE('',#12597,#12753,#2707,.T.);
#15800=EDGE_CURVE('',#12592,#12754,#2708,.T.);
#15801=EDGE_CURVE('',#12754,#12670,#2709,.F.);
#15802=EDGE_CURVE('',#12591,#12755,#2710,.T.);
#15803=EDGE_CURVE('',#12754,#12755,#2711,.T.);
#15804=EDGE_CURVE('',#12756,#12589,#2712,.T.);
#15805=EDGE_CURVE('',#12671,#12756,#2713,.T.);
#15806=EDGE_CURVE('',#12754,#12756,#2714,.T.);
#15807=EDGE_CURVE('',#12756,#12757,#2715,.T.);
#15808=EDGE_CURVE('',#12757,#12590,#2716,.T.);
#15809=EDGE_CURVE('',#12755,#12757,#2717,.T.);
#15810=EDGE_CURVE('',#12758,#12583,#2718,.T.);
#15811=EDGE_CURVE('',#12673,#12758,#2719,.T.);
#15812=EDGE_CURVE('',#12759,#12758,#2720,.T.);
#15813=EDGE_CURVE('',#12672,#12759,#2721,.T.);
#15814=EDGE_CURVE('',#12586,#12759,#2722,.T.);
#15815=EDGE_CURVE('',#12758,#12760,#2723,.T.);
#15816=EDGE_CURVE('',#12760,#12584,#2724,.T.);
#15817=EDGE_CURVE('',#12759,#12761,#2725,.T.);
#15818=EDGE_CURVE('',#12761,#12760,#2726,.T.);
#15819=EDGE_CURVE('',#12585,#12761,#2727,.T.);
#15820=EDGE_CURVE('',#12762,#12577,#2728,.T.);
#15821=EDGE_CURVE('',#12675,#12762,#2729,.T.);
#15822=EDGE_CURVE('',#12763,#12762,#2730,.T.);
#15823=EDGE_CURVE('',#12674,#12763,#2731,.T.);
#15824=EDGE_CURVE('',#12580,#12763,#2732,.T.);
#15825=EDGE_CURVE('',#12762,#12764,#2733,.T.);
#15826=EDGE_CURVE('',#12764,#12578,#2734,.T.);
#15827=EDGE_CURVE('',#12763,#12765,#2735,.T.);
#15828=EDGE_CURVE('',#12765,#12764,#2736,.T.);
#15829=EDGE_CURVE('',#12579,#12765,#2737,.T.);
#15830=EDGE_CURVE('',#12766,#12571,#2738,.T.);
#15831=EDGE_CURVE('',#12677,#12766,#2739,.T.);
#15832=EDGE_CURVE('',#12767,#12766,#2740,.T.);
#15833=EDGE_CURVE('',#12676,#12767,#2741,.T.);
#15834=EDGE_CURVE('',#12574,#12767,#2742,.T.);
#15835=EDGE_CURVE('',#12766,#12768,#2743,.T.);
#15836=EDGE_CURVE('',#12768,#12572,#2744,.T.);
#15837=EDGE_CURVE('',#12767,#12769,#2745,.T.);
#15838=EDGE_CURVE('',#12769,#12768,#2746,.T.);
#15839=EDGE_CURVE('',#12573,#12769,#2747,.T.);
#15840=EDGE_CURVE('',#12770,#12565,#2748,.T.);
#15841=EDGE_CURVE('',#12679,#12770,#2749,.T.);
#15842=EDGE_CURVE('',#12771,#12770,#2750,.T.);
#15843=EDGE_CURVE('',#12678,#12771,#2751,.T.);
#15844=EDGE_CURVE('',#12568,#12771,#2752,.T.);
#15845=EDGE_CURVE('',#12770,#12772,#2753,.T.);
#15846=EDGE_CURVE('',#12772,#12566,#2754,.T.);
#15847=EDGE_CURVE('',#12771,#12773,#2755,.T.);
#15848=EDGE_CURVE('',#12773,#12772,#2756,.T.);
#15849=EDGE_CURVE('',#12567,#12773,#2757,.T.);
#15850=EDGE_CURVE('',#12774,#12559,#2758,.T.);
#15851=EDGE_CURVE('',#12681,#12774,#2759,.T.);
#15852=EDGE_CURVE('',#12775,#12774,#2760,.T.);
#15853=EDGE_CURVE('',#12680,#12775,#2761,.T.);
#15854=EDGE_CURVE('',#12562,#12775,#2762,.T.);
#15855=EDGE_CURVE('',#12774,#12776,#2763,.T.);
#15856=EDGE_CURVE('',#12776,#12560,#2764,.T.);
#15857=EDGE_CURVE('',#12775,#12777,#2765,.T.);
#15858=EDGE_CURVE('',#12777,#12776,#2766,.T.);
#15859=EDGE_CURVE('',#12561,#12777,#2767,.T.);
#15860=EDGE_CURVE('',#12778,#12553,#2768,.T.);
#15861=EDGE_CURVE('',#12683,#12778,#2769,.T.);
#15862=EDGE_CURVE('',#12779,#12778,#2770,.T.);
#15863=EDGE_CURVE('',#12682,#12779,#2771,.T.);
#15864=EDGE_CURVE('',#12556,#12779,#2772,.T.);
#15865=EDGE_CURVE('',#12778,#12780,#2773,.T.);
#15866=EDGE_CURVE('',#12780,#12554,#2774,.T.);
#15867=EDGE_CURVE('',#12779,#12781,#2775,.T.);
#15868=EDGE_CURVE('',#12781,#12780,#2776,.T.);
#15869=EDGE_CURVE('',#12555,#12781,#2777,.T.);
#15870=EDGE_CURVE('',#12782,#12547,#2778,.T.);
#15871=EDGE_CURVE('',#12685,#12782,#2779,.T.);
#15872=EDGE_CURVE('',#12783,#12782,#2780,.T.);
#15873=EDGE_CURVE('',#12684,#12783,#2781,.T.);
#15874=EDGE_CURVE('',#12550,#12783,#2782,.T.);
#15875=EDGE_CURVE('',#12782,#12784,#2783,.T.);
#15876=EDGE_CURVE('',#12784,#12548,#2784,.T.);
#15877=EDGE_CURVE('',#12783,#12785,#2785,.T.);
#15878=EDGE_CURVE('',#12785,#12784,#2786,.T.);
#15879=EDGE_CURVE('',#12549,#12785,#2787,.T.);
#15880=EDGE_CURVE('',#12786,#12541,#2788,.T.);
#15881=EDGE_CURVE('',#12687,#12786,#2789,.T.);
#15882=EDGE_CURVE('',#12787,#12786,#2790,.T.);
#15883=EDGE_CURVE('',#12686,#12787,#2791,.T.);
#15884=EDGE_CURVE('',#12544,#12787,#2792,.T.);
#15885=EDGE_CURVE('',#12786,#12788,#2793,.T.);
#15886=EDGE_CURVE('',#12788,#12542,#2794,.T.);
#15887=EDGE_CURVE('',#12787,#12789,#2795,.T.);
#15888=EDGE_CURVE('',#12789,#12788,#2796,.T.);
#15889=EDGE_CURVE('',#12543,#12789,#2797,.T.);
#15890=EDGE_CURVE('',#12790,#12535,#2798,.T.);
#15891=EDGE_CURVE('',#12689,#12790,#2799,.T.);
#15892=EDGE_CURVE('',#12791,#12790,#2800,.T.);
#15893=EDGE_CURVE('',#12688,#12791,#2801,.T.);
#15894=EDGE_CURVE('',#12538,#12791,#2802,.T.);
#15895=EDGE_CURVE('',#12790,#12792,#2803,.T.);
#15896=EDGE_CURVE('',#12792,#12536,#2804,.T.);
#15897=EDGE_CURVE('',#12791,#12793,#2805,.T.);
#15898=EDGE_CURVE('',#12793,#12792,#2806,.T.);
#15899=EDGE_CURVE('',#12537,#12793,#2807,.T.);
#15900=EDGE_CURVE('',#12794,#12529,#2808,.T.);
#15901=EDGE_CURVE('',#12691,#12794,#2809,.T.);
#15902=EDGE_CURVE('',#12795,#12794,#2810,.T.);
#15903=EDGE_CURVE('',#12690,#12795,#2811,.T.);
#15904=EDGE_CURVE('',#12532,#12795,#2812,.T.);
#15905=EDGE_CURVE('',#12794,#12796,#2813,.T.);
#15906=EDGE_CURVE('',#12796,#12530,#2814,.T.);
#15907=EDGE_CURVE('',#12795,#12797,#2815,.T.);
#15908=EDGE_CURVE('',#12797,#12796,#2816,.T.);
#15909=EDGE_CURVE('',#12531,#12797,#2817,.T.);
#15910=EDGE_CURVE('',#12798,#12523,#2818,.T.);
#15911=EDGE_CURVE('',#12693,#12798,#2819,.T.);
#15912=EDGE_CURVE('',#12799,#12798,#2820,.T.);
#15913=EDGE_CURVE('',#12692,#12799,#2821,.T.);
#15914=EDGE_CURVE('',#12526,#12799,#2822,.T.);
#15915=EDGE_CURVE('',#12798,#12800,#2823,.T.);
#15916=EDGE_CURVE('',#12800,#12524,#2824,.T.);
#15917=EDGE_CURVE('',#12799,#12801,#2825,.T.);
#15918=EDGE_CURVE('',#12801,#12800,#2826,.T.);
#15919=EDGE_CURVE('',#12525,#12801,#2827,.T.);
#15920=EDGE_CURVE('',#12802,#12517,#2828,.T.);
#15921=EDGE_CURVE('',#12695,#12802,#2829,.T.);
#15922=EDGE_CURVE('',#12803,#12802,#2830,.T.);
#15923=EDGE_CURVE('',#12694,#12803,#2831,.T.);
#15924=EDGE_CURVE('',#12520,#12803,#2832,.T.);
#15925=EDGE_CURVE('',#12802,#12804,#2833,.T.);
#15926=EDGE_CURVE('',#12804,#12518,#2834,.T.);
#15927=EDGE_CURVE('',#12803,#12805,#2835,.T.);
#15928=EDGE_CURVE('',#12805,#12804,#2836,.T.);
#15929=EDGE_CURVE('',#12519,#12805,#2837,.T.);
#15930=EDGE_CURVE('',#12806,#12807,#2838,.T.);
#15931=EDGE_CURVE('',#12807,#12808,#2839,.F.);
#15932=EDGE_CURVE('',#12808,#12809,#2840,.T.);
#15933=EDGE_CURVE('',#12809,#12806,#2841,.T.);
#15934=EDGE_CURVE('',#12809,#12421,#2842,.T.);
#15935=EDGE_CURVE('',#12420,#12806,#2843,.T.);
#15936=EDGE_CURVE('',#12807,#12425,#2844,.T.);
#15937=EDGE_CURVE('',#12810,#12419,#2845,.T.);
#15938=EDGE_CURVE('',#12811,#12810,#2846,.T.);
#15939=EDGE_CURVE('',#12414,#12811,#2847,.T.);
#15940=EDGE_CURVE('',#12812,#12413,#2848,.T.);
#15941=EDGE_CURVE('',#12813,#12812,#2849,.T.);
#15942=EDGE_CURVE('',#12408,#12813,#2850,.T.);
#15943=EDGE_CURVE('',#12814,#12407,#2851,.T.);
#15944=EDGE_CURVE('',#12815,#12814,#2852,.T.);
#15945=EDGE_CURVE('',#12402,#12815,#2853,.T.);
#15946=EDGE_CURVE('',#12816,#12401,#2854,.T.);
#15947=EDGE_CURVE('',#12817,#12816,#2855,.T.);
#15948=EDGE_CURVE('',#12396,#12817,#2856,.T.);
#15949=EDGE_CURVE('',#12818,#12395,#2857,.T.);
#15950=EDGE_CURVE('',#12819,#12818,#2858,.T.);
#15951=EDGE_CURVE('',#12390,#12819,#2859,.T.);
#15952=EDGE_CURVE('',#12820,#12389,#2860,.T.);
#15953=EDGE_CURVE('',#12821,#12820,#2861,.T.);
#15954=EDGE_CURVE('',#12384,#12821,#2862,.T.);
#15955=EDGE_CURVE('',#12822,#12383,#2863,.T.);
#15956=EDGE_CURVE('',#12823,#12822,#2864,.T.);
#15957=EDGE_CURVE('',#12378,#12823,#2865,.T.);
#15958=EDGE_CURVE('',#12824,#12377,#2866,.T.);
#15959=EDGE_CURVE('',#12825,#12824,#2867,.T.);
#15960=EDGE_CURVE('',#12372,#12825,#2868,.T.);
#15961=EDGE_CURVE('',#12826,#12371,#2869,.T.);
#15962=EDGE_CURVE('',#12827,#12826,#2870,.T.);
#15963=EDGE_CURVE('',#12366,#12827,#2871,.T.);
#15964=EDGE_CURVE('',#12828,#12365,#2872,.T.);
#15965=EDGE_CURVE('',#12829,#12828,#2873,.T.);
#15966=EDGE_CURVE('',#12360,#12829,#2874,.T.);
#15967=EDGE_CURVE('',#12830,#12359,#2875,.T.);
#15968=EDGE_CURVE('',#12831,#12830,#2876,.T.);
#15969=EDGE_CURVE('',#12354,#12831,#2877,.T.);
#15970=EDGE_CURVE('',#12832,#12353,#2878,.T.);
#15971=EDGE_CURVE('',#12833,#12832,#2879,.T.);
#15972=EDGE_CURVE('',#12348,#12833,#2880,.T.);
#15973=EDGE_CURVE('',#12834,#12347,#2881,.T.);
#15974=EDGE_CURVE('',#12835,#12834,#2882,.T.);
#15975=EDGE_CURVE('',#12342,#12835,#2883,.T.);
#15976=EDGE_CURVE('',#12836,#12341,#2884,.T.);
#15977=EDGE_CURVE('',#12837,#12836,#2885,.T.);
#15978=EDGE_CURVE('',#12336,#12837,#2886,.T.);
#15979=EDGE_CURVE('',#12838,#12335,#2887,.T.);
#15980=EDGE_CURVE('',#12839,#12838,#2888,.T.);
#15981=EDGE_CURVE('',#12330,#12839,#2889,.T.);
#15982=EDGE_CURVE('',#12840,#12329,#2890,.T.);
#15983=EDGE_CURVE('',#12841,#12840,#2891,.T.);
#15984=EDGE_CURVE('',#12324,#12841,#2892,.T.);
#15985=EDGE_CURVE('',#12842,#12323,#2893,.T.);
#15986=EDGE_CURVE('',#12843,#12842,#2894,.T.);
#15987=EDGE_CURVE('',#12318,#12843,#2895,.T.);
#15988=EDGE_CURVE('',#12844,#12317,#2896,.T.);
#15989=EDGE_CURVE('',#12845,#12844,#2897,.T.);
#15990=EDGE_CURVE('',#12312,#12845,#2898,.T.);
#15991=EDGE_CURVE('',#12846,#12311,#2899,.T.);
#15992=EDGE_CURVE('',#12847,#12846,#2900,.T.);
#15993=EDGE_CURVE('',#12306,#12847,#2901,.T.);
#15994=EDGE_CURVE('',#12848,#12305,#2902,.T.);
#15995=EDGE_CURVE('',#12849,#12848,#2903,.T.);
#15996=EDGE_CURVE('',#12300,#12849,#2904,.T.);
#15997=EDGE_CURVE('',#12850,#12299,#2905,.T.);
#15998=EDGE_CURVE('',#12851,#12850,#2906,.T.);
#15999=EDGE_CURVE('',#12294,#12851,#2907,.T.);
#16000=EDGE_CURVE('',#12852,#12293,#2908,.T.);
#16001=EDGE_CURVE('',#12853,#12852,#2909,.T.);
#16002=EDGE_CURVE('',#12288,#12853,#2910,.T.);
#16003=EDGE_CURVE('',#12854,#12467,#2911,.T.);
#16004=EDGE_CURVE('',#12855,#12854,#2912,.T.);
#16005=EDGE_CURVE('',#12462,#12855,#2913,.T.);
#16006=EDGE_CURVE('',#12856,#12461,#2914,.T.);
#16007=EDGE_CURVE('',#12857,#12856,#2915,.T.);
#16008=EDGE_CURVE('',#12456,#12857,#2916,.T.);
#16009=EDGE_CURVE('',#12858,#12455,#2917,.T.);
#16010=EDGE_CURVE('',#12859,#12858,#2918,.T.);
#16011=EDGE_CURVE('',#12450,#12859,#2919,.T.);
#16012=EDGE_CURVE('',#12860,#12449,#2920,.T.);
#16013=EDGE_CURVE('',#12861,#12860,#2921,.T.);
#16014=EDGE_CURVE('',#12444,#12861,#2922,.T.);
#16015=EDGE_CURVE('',#12862,#12443,#2923,.T.);
#16016=EDGE_CURVE('',#12863,#12862,#2924,.T.);
#16017=EDGE_CURVE('',#12438,#12863,#2925,.T.);
#16018=EDGE_CURVE('',#12864,#12437,#2926,.T.);
#16019=EDGE_CURVE('',#12865,#12864,#2927,.T.);
#16020=EDGE_CURVE('',#12432,#12865,#2928,.T.);
#16021=EDGE_CURVE('',#12866,#12431,#2929,.T.);
#16022=EDGE_CURVE('',#12867,#12866,#2930,.T.);
#16023=EDGE_CURVE('',#12426,#12867,#2931,.T.);
#16024=EDGE_CURVE('',#12868,#12869,#2932,.T.);
#16025=EDGE_CURVE('',#12870,#12868,#2933,.T.);
#16026=EDGE_CURVE('',#12871,#12870,#2934,.T.);
#16027=EDGE_CURVE('',#12871,#12872,#10720,.T.);
#16028=EDGE_CURVE('',#12873,#12872,#2935,.T.);
#16029=EDGE_CURVE('',#12874,#12873,#2936,.T.);
#16030=EDGE_CURVE('',#12875,#12874,#2937,.T.);
#16031=EDGE_CURVE('',#12875,#12869,#10721,.T.);
#16032=EDGE_CURVE('',#12424,#12808,#2938,.T.);
#16033=EDGE_CURVE('',#12866,#12876,#2939,.T.);
#16034=EDGE_CURVE('',#12876,#12877,#2940,.T.);
#16035=EDGE_CURVE('',#12877,#12867,#2941,.T.);
#16036=EDGE_CURVE('',#12430,#12876,#2942,.T.);
#16037=EDGE_CURVE('',#12877,#12427,#2943,.T.);
#16038=EDGE_CURVE('',#12864,#12878,#2944,.T.);
#16039=EDGE_CURVE('',#12878,#12879,#2945,.T.);
#16040=EDGE_CURVE('',#12879,#12865,#2946,.T.);
#16041=EDGE_CURVE('',#12436,#12878,#2947,.T.);
#16042=EDGE_CURVE('',#12879,#12433,#2948,.T.);
#16043=EDGE_CURVE('',#12879,#12880,#2949,.T.);
#16044=EDGE_CURVE('',#12880,#12434,#2950,.T.);
#16045=EDGE_CURVE('',#12878,#12881,#2951,.T.);
#16046=EDGE_CURVE('',#12881,#12880,#2952,.T.);
#16047=EDGE_CURVE('',#12862,#12882,#2953,.T.);
#16048=EDGE_CURVE('',#12882,#12883,#2954,.T.);
#16049=EDGE_CURVE('',#12883,#12863,#2955,.T.);
#16050=EDGE_CURVE('',#12442,#12882,#2956,.T.);
#16051=EDGE_CURVE('',#12883,#12439,#2957,.T.);
#16052=EDGE_CURVE('',#12860,#12884,#2958,.T.);
#16053=EDGE_CURVE('',#12884,#12885,#2959,.T.);
#16054=EDGE_CURVE('',#12885,#12861,#2960,.T.);
#16055=EDGE_CURVE('',#12448,#12884,#2961,.T.);
#16056=EDGE_CURVE('',#12885,#12445,#2962,.T.);
#16057=EDGE_CURVE('',#12885,#12886,#2963,.T.);
#16058=EDGE_CURVE('',#12886,#12446,#2964,.T.);
#16059=EDGE_CURVE('',#12884,#12887,#2965,.T.);
#16060=EDGE_CURVE('',#12887,#12886,#2966,.T.);
#16061=EDGE_CURVE('',#12858,#12888,#2967,.T.);
#16062=EDGE_CURVE('',#12888,#12889,#2968,.T.);
#16063=EDGE_CURVE('',#12889,#12859,#2969,.T.);
#16064=EDGE_CURVE('',#12454,#12888,#2970,.T.);
#16065=EDGE_CURVE('',#12889,#12451,#2971,.T.);
#16066=EDGE_CURVE('',#12856,#12890,#2972,.T.);
#16067=EDGE_CURVE('',#12890,#12891,#2973,.T.);
#16068=EDGE_CURVE('',#12891,#12857,#2974,.T.);
#16069=EDGE_CURVE('',#12460,#12890,#2975,.T.);
#16070=EDGE_CURVE('',#12891,#12457,#2976,.T.);
#16071=EDGE_CURVE('',#12891,#12892,#2977,.T.);
#16072=EDGE_CURVE('',#12892,#12458,#2978,.T.);
#16073=EDGE_CURVE('',#12890,#12893,#2979,.T.);
#16074=EDGE_CURVE('',#12893,#12892,#2980,.T.);
#16075=EDGE_CURVE('',#12855,#12894,#2981,.F.);
#16076=EDGE_CURVE('',#12894,#12463,#2982,.T.);
#16077=EDGE_CURVE('',#12895,#12894,#2983,.T.);
#16078=EDGE_CURVE('',#12854,#12895,#2984,.T.);
#16079=EDGE_CURVE('',#12466,#12895,#2985,.T.);
#16080=EDGE_CURVE('',#12852,#12896,#2986,.T.);
#16081=EDGE_CURVE('',#12896,#12897,#2987,.T.);
#16082=EDGE_CURVE('',#12897,#12853,#2988,.T.);
#16083=EDGE_CURVE('',#12292,#12896,#2989,.T.);
#16084=EDGE_CURVE('',#12897,#12289,#2990,.T.);
#16085=EDGE_CURVE('',#12850,#12898,#2991,.T.);
#16086=EDGE_CURVE('',#12898,#12899,#2992,.T.);
#16087=EDGE_CURVE('',#12899,#12851,#2993,.T.);
#16088=EDGE_CURVE('',#12298,#12898,#2994,.T.);
#16089=EDGE_CURVE('',#12899,#12295,#2995,.T.);
#16090=EDGE_CURVE('',#12899,#12900,#2996,.T.);
#16091=EDGE_CURVE('',#12900,#12296,#2997,.T.);
#16092=EDGE_CURVE('',#12898,#12901,#2998,.T.);
#16093=EDGE_CURVE('',#12901,#12900,#2999,.T.);
#16094=EDGE_CURVE('',#12848,#12902,#3000,.T.);
#16095=EDGE_CURVE('',#12902,#12903,#3001,.T.);
#16096=EDGE_CURVE('',#12903,#12849,#3002,.T.);
#16097=EDGE_CURVE('',#12304,#12902,#3003,.T.);
#16098=EDGE_CURVE('',#12903,#12301,#3004,.T.);
#16099=EDGE_CURVE('',#12846,#12904,#3005,.T.);
#16100=EDGE_CURVE('',#12904,#12905,#3006,.T.);
#16101=EDGE_CURVE('',#12905,#12847,#3007,.T.);
#16102=EDGE_CURVE('',#12310,#12904,#3008,.T.);
#16103=EDGE_CURVE('',#12905,#12307,#3009,.T.);
#16104=EDGE_CURVE('',#12905,#12906,#3010,.T.);
#16105=EDGE_CURVE('',#12906,#12308,#3011,.T.);
#16106=EDGE_CURVE('',#12904,#12907,#3012,.T.);
#16107=EDGE_CURVE('',#12907,#12906,#3013,.T.);
#16108=EDGE_CURVE('',#12844,#12908,#3014,.T.);
#16109=EDGE_CURVE('',#12908,#12909,#3015,.T.);
#16110=EDGE_CURVE('',#12909,#12845,#3016,.T.);
#16111=EDGE_CURVE('',#12316,#12908,#3017,.T.);
#16112=EDGE_CURVE('',#12909,#12313,#3018,.T.);
#16113=EDGE_CURVE('',#12842,#12910,#3019,.T.);
#16114=EDGE_CURVE('',#12910,#12911,#3020,.T.);
#16115=EDGE_CURVE('',#12911,#12843,#3021,.T.);
#16116=EDGE_CURVE('',#12322,#12910,#3022,.T.);
#16117=EDGE_CURVE('',#12911,#12319,#3023,.T.);
#16118=EDGE_CURVE('',#12911,#12912,#3024,.T.);
#16119=EDGE_CURVE('',#12912,#12320,#3025,.T.);
#16120=EDGE_CURVE('',#12910,#12913,#3026,.T.);
#16121=EDGE_CURVE('',#12913,#12912,#3027,.T.);
#16122=EDGE_CURVE('',#12840,#12914,#3028,.T.);
#16123=EDGE_CURVE('',#12914,#12915,#3029,.T.);
#16124=EDGE_CURVE('',#12915,#12841,#3030,.T.);
#16125=EDGE_CURVE('',#12328,#12914,#3031,.T.);
#16126=EDGE_CURVE('',#12915,#12325,#3032,.T.);
#16127=EDGE_CURVE('',#12838,#12916,#3033,.T.);
#16128=EDGE_CURVE('',#12916,#12917,#3034,.T.);
#16129=EDGE_CURVE('',#12917,#12839,#3035,.T.);
#16130=EDGE_CURVE('',#12334,#12916,#3036,.T.);
#16131=EDGE_CURVE('',#12917,#12331,#3037,.T.);
#16132=EDGE_CURVE('',#12917,#12918,#3038,.T.);
#16133=EDGE_CURVE('',#12918,#12332,#3039,.T.);
#16134=EDGE_CURVE('',#12916,#12919,#3040,.T.);
#16135=EDGE_CURVE('',#12919,#12918,#3041,.T.);
#16136=EDGE_CURVE('',#12836,#12920,#3042,.T.);
#16137=EDGE_CURVE('',#12920,#12921,#3043,.T.);
#16138=EDGE_CURVE('',#12921,#12837,#3044,.T.);
#16139=EDGE_CURVE('',#12340,#12920,#3045,.T.);
#16140=EDGE_CURVE('',#12921,#12337,#3046,.T.);
#16141=EDGE_CURVE('',#12834,#12922,#3047,.T.);
#16142=EDGE_CURVE('',#12922,#12923,#3048,.T.);
#16143=EDGE_CURVE('',#12923,#12835,#3049,.T.);
#16144=EDGE_CURVE('',#12346,#12922,#3050,.T.);
#16145=EDGE_CURVE('',#12923,#12343,#3051,.T.);
#16146=EDGE_CURVE('',#12923,#12924,#3052,.T.);
#16147=EDGE_CURVE('',#12924,#12344,#3053,.T.);
#16148=EDGE_CURVE('',#12922,#12925,#3054,.T.);
#16149=EDGE_CURVE('',#12925,#12924,#3055,.T.);
#16150=EDGE_CURVE('',#12832,#12926,#3056,.T.);
#16151=EDGE_CURVE('',#12926,#12927,#3057,.T.);
#16152=EDGE_CURVE('',#12927,#12833,#3058,.T.);
#16153=EDGE_CURVE('',#12352,#12926,#3059,.T.);
#16154=EDGE_CURVE('',#12927,#12349,#3060,.T.);
#16155=EDGE_CURVE('',#12830,#12928,#3061,.T.);
#16156=EDGE_CURVE('',#12928,#12929,#3062,.T.);
#16157=EDGE_CURVE('',#12929,#12831,#3063,.T.);
#16158=EDGE_CURVE('',#12358,#12928,#3064,.T.);
#16159=EDGE_CURVE('',#12929,#12355,#3065,.T.);
#16160=EDGE_CURVE('',#12929,#12930,#3066,.T.);
#16161=EDGE_CURVE('',#12930,#12356,#3067,.T.);
#16162=EDGE_CURVE('',#12928,#12931,#3068,.T.);
#16163=EDGE_CURVE('',#12931,#12930,#3069,.T.);
#16164=EDGE_CURVE('',#12828,#12932,#3070,.F.);
#16165=EDGE_CURVE('',#12932,#12933,#3071,.T.);
#16166=EDGE_CURVE('',#12933,#12829,#3072,.T.);
#16167=EDGE_CURVE('',#12933,#12361,#3073,.T.);
#16168=EDGE_CURVE('',#12364,#12932,#3074,.T.);
#16169=EDGE_CURVE('',#12826,#12934,#3075,.T.);
#16170=EDGE_CURVE('',#12934,#12935,#3076,.T.);
#16171=EDGE_CURVE('',#12935,#12827,#3077,.T.);
#16172=EDGE_CURVE('',#12370,#12934,#3078,.T.);
#16173=EDGE_CURVE('',#12935,#12367,#3079,.T.);
#16174=EDGE_CURVE('',#12824,#12936,#3080,.T.);
#16175=EDGE_CURVE('',#12936,#12937,#3081,.T.);
#16176=EDGE_CURVE('',#12937,#12825,#3082,.T.);
#16177=EDGE_CURVE('',#12376,#12936,#3083,.T.);
#16178=EDGE_CURVE('',#12937,#12373,#3084,.T.);
#16179=EDGE_CURVE('',#12937,#12938,#3085,.T.);
#16180=EDGE_CURVE('',#12938,#12374,#3086,.T.);
#16181=EDGE_CURVE('',#12936,#12939,#3087,.T.);
#16182=EDGE_CURVE('',#12939,#12938,#3088,.T.);
#16183=EDGE_CURVE('',#12822,#12940,#3089,.T.);
#16184=EDGE_CURVE('',#12940,#12941,#3090,.T.);
#16185=EDGE_CURVE('',#12941,#12823,#3091,.T.);
#16186=EDGE_CURVE('',#12382,#12940,#3092,.T.);
#16187=EDGE_CURVE('',#12941,#12379,#3093,.T.);
#16188=EDGE_CURVE('',#12820,#12942,#3094,.T.);
#16189=EDGE_CURVE('',#12942,#12943,#3095,.T.);
#16190=EDGE_CURVE('',#12943,#12821,#3096,.T.);
#16191=EDGE_CURVE('',#12388,#12942,#3097,.T.);
#16192=EDGE_CURVE('',#12943,#12385,#3098,.T.);
#16193=EDGE_CURVE('',#12943,#12944,#3099,.T.);
#16194=EDGE_CURVE('',#12944,#12386,#3100,.T.);
#16195=EDGE_CURVE('',#12942,#12945,#3101,.T.);
#16196=EDGE_CURVE('',#12945,#12944,#3102,.T.);
#16197=EDGE_CURVE('',#12818,#12946,#3103,.T.);
#16198=EDGE_CURVE('',#12946,#12947,#3104,.T.);
#16199=EDGE_CURVE('',#12947,#12819,#3105,.T.);
#16200=EDGE_CURVE('',#12394,#12946,#3106,.T.);
#16201=EDGE_CURVE('',#12947,#12391,#3107,.T.);
#16202=EDGE_CURVE('',#12816,#12948,#3108,.T.);
#16203=EDGE_CURVE('',#12948,#12949,#3109,.T.);
#16204=EDGE_CURVE('',#12949,#12817,#3110,.T.);
#16205=EDGE_CURVE('',#12400,#12948,#3111,.T.);
#16206=EDGE_CURVE('',#12949,#12397,#3112,.T.);
#16207=EDGE_CURVE('',#12949,#12950,#3113,.T.);
#16208=EDGE_CURVE('',#12950,#12398,#3114,.T.);
#16209=EDGE_CURVE('',#12948,#12951,#3115,.T.);
#16210=EDGE_CURVE('',#12951,#12950,#3116,.T.);
#16211=EDGE_CURVE('',#12815,#12952,#3117,.F.);
#16212=EDGE_CURVE('',#12952,#12403,#3118,.T.);
#16213=EDGE_CURVE('',#12953,#12952,#3119,.T.);
#16214=EDGE_CURVE('',#12814,#12953,#3120,.T.);
#16215=EDGE_CURVE('',#12406,#12953,#3121,.T.);
#16216=EDGE_CURVE('',#12812,#12954,#3122,.T.);
#16217=EDGE_CURVE('',#12954,#12955,#3123,.T.);
#16218=EDGE_CURVE('',#12955,#12813,#3124,.T.);
#16219=EDGE_CURVE('',#12412,#12954,#3125,.T.);
#16220=EDGE_CURVE('',#12955,#12409,#3126,.T.);
#16221=EDGE_CURVE('',#12810,#12956,#3127,.T.);
#16222=EDGE_CURVE('',#12956,#12957,#3128,.T.);
#16223=EDGE_CURVE('',#12957,#12811,#3129,.T.);
#16224=EDGE_CURVE('',#12418,#12956,#3130,.T.);
#16225=EDGE_CURVE('',#12957,#12415,#3131,.T.);
#16226=EDGE_CURVE('',#12957,#12958,#3132,.T.);
#16227=EDGE_CURVE('',#12958,#12416,#3133,.T.);
#16228=EDGE_CURVE('',#12956,#12959,#3134,.T.);
#16229=EDGE_CURVE('',#12959,#12958,#3135,.T.);
#16230=EDGE_CURVE('',#12715,#12960,#3136,.T.);
#16231=EDGE_CURVE('',#12960,#12961,#3137,.T.);
#16232=EDGE_CURVE('',#12961,#12709,#3138,.T.);
#16233=EDGE_CURVE('',#12714,#12962,#322,.T.);
#16234=EDGE_CURVE('',#12962,#12960,#3139,.T.);
#16235=EDGE_CURVE('',#12961,#12963,#3140,.T.);
#16236=EDGE_CURVE('',#12963,#12708,#323,.T.);
#16237=EDGE_CURVE('',#12964,#12961,#3141,.T.);
#16238=EDGE_CURVE('',#12965,#12964,#3142,.T.);
#16239=EDGE_CURVE('',#12963,#12965,#3143,.T.);
#16240=EDGE_CURVE('',#12966,#12960,#3144,.T.);
#16241=EDGE_CURVE('',#12964,#12966,#3145,.T.);
#16242=EDGE_CURVE('',#12967,#12962,#3146,.T.);
#16243=EDGE_CURVE('',#12966,#12967,#3147,.T.);
#16244=EDGE_CURVE('',#12968,#12713,#324,.T.);
#16245=EDGE_CURVE('',#12968,#12969,#3148,.T.);
#16246=EDGE_CURVE('',#12872,#12969,#325,.T.);
#16247=EDGE_CURVE('',#12967,#12871,#326,.T.);
#16248=EDGE_CURVE('',#12966,#12870,#3149,.T.);
#16249=EDGE_CURVE('',#12868,#12964,#3150,.T.);
#16250=EDGE_CURVE('',#12869,#12965,#327,.T.);
#16251=EDGE_CURVE('',#12970,#12971,#3151,.T.);
#16252=EDGE_CURVE('',#12971,#12875,#328,.T.);
#16253=EDGE_CURVE('',#12874,#12970,#3152,.T.);
#16254=EDGE_CURVE('',#12873,#12972,#3153,.T.);
#16255=EDGE_CURVE('',#12972,#12970,#3154,.T.);
#16256=EDGE_CURVE('',#12969,#12972,#3155,.T.);
#16257=EDGE_CURVE('',#12970,#12973,#3156,.T.);
#16258=EDGE_CURVE('',#12974,#12973,#3157,.T.);
#16259=EDGE_CURVE('',#12971,#12974,#3158,.T.);
#16260=EDGE_CURVE('',#12972,#12975,#3159,.T.);
#16261=EDGE_CURVE('',#12973,#12975,#3160,.T.);
#16262=EDGE_CURVE('',#12975,#12968,#3161,.T.);
#16263=EDGE_CURVE('',#12710,#12974,#329,.T.);
#16264=EDGE_CURVE('',#12973,#12711,#3162,.T.);
#16265=EDGE_CURVE('',#12975,#12712,#3163,.T.);
#16266=EDGE_CURVE('',#12417,#12959,#3164,.T.);
#16267=EDGE_CURVE('',#12954,#12976,#3165,.T.);
#16268=EDGE_CURVE('',#12976,#12977,#3166,.T.);
#16269=EDGE_CURVE('',#12955,#12977,#3167,.T.);
#16270=EDGE_CURVE('',#12411,#12976,#3168,.T.);
#16271=EDGE_CURVE('',#12977,#12410,#3169,.T.);
#16272=EDGE_CURVE('',#12953,#12978,#3170,.T.);
#16273=EDGE_CURVE('',#12978,#12979,#3171,.T.);
#16274=EDGE_CURVE('',#12952,#12979,#3172,.T.);
#16275=EDGE_CURVE('',#12405,#12978,#3173,.T.);
#16276=EDGE_CURVE('',#12979,#12404,#3174,.T.);
#16277=EDGE_CURVE('',#12399,#12951,#3175,.T.);
#16278=EDGE_CURVE('',#12946,#12980,#3176,.T.);
#16279=EDGE_CURVE('',#12980,#12981,#3177,.T.);
#16280=EDGE_CURVE('',#12947,#12981,#3178,.T.);
#16281=EDGE_CURVE('',#12393,#12980,#3179,.T.);
#16282=EDGE_CURVE('',#12981,#12392,#3180,.T.);
#16283=EDGE_CURVE('',#12387,#12945,#3181,.T.);
#16284=EDGE_CURVE('',#12940,#12982,#3182,.T.);
#16285=EDGE_CURVE('',#12982,#12983,#3183,.T.);
#16286=EDGE_CURVE('',#12941,#12983,#3184,.T.);
#16287=EDGE_CURVE('',#12381,#12982,#3185,.T.);
#16288=EDGE_CURVE('',#12983,#12380,#3186,.T.);
#16289=EDGE_CURVE('',#12375,#12939,#3187,.T.);
#16290=EDGE_CURVE('',#12934,#12984,#3188,.T.);
#16291=EDGE_CURVE('',#12984,#12985,#3189,.T.);
#16292=EDGE_CURVE('',#12935,#12985,#3190,.T.);
#16293=EDGE_CURVE('',#12369,#12984,#3191,.T.);
#16294=EDGE_CURVE('',#12985,#12368,#3192,.T.);
#16295=EDGE_CURVE('',#12932,#12986,#3193,.T.);
#16296=EDGE_CURVE('',#12986,#12987,#3194,.T.);
#16297=EDGE_CURVE('',#12933,#12987,#3195,.T.);
#16298=EDGE_CURVE('',#12363,#12986,#3196,.T.);
#16299=EDGE_CURVE('',#12987,#12362,#3197,.T.);
#16300=EDGE_CURVE('',#12357,#12931,#3198,.T.);
#16301=EDGE_CURVE('',#12926,#12988,#3199,.T.);
#16302=EDGE_CURVE('',#12988,#12989,#3200,.T.);
#16303=EDGE_CURVE('',#12927,#12989,#3201,.T.);
#16304=EDGE_CURVE('',#12351,#12988,#3202,.T.);
#16305=EDGE_CURVE('',#12989,#12350,#3203,.T.);
#16306=EDGE_CURVE('',#12345,#12925,#3204,.T.);
#16307=EDGE_CURVE('',#12920,#12990,#3205,.T.);
#16308=EDGE_CURVE('',#12990,#12991,#3206,.T.);
#16309=EDGE_CURVE('',#12921,#12991,#3207,.T.);
#16310=EDGE_CURVE('',#12339,#12990,#3208,.T.);
#16311=EDGE_CURVE('',#12991,#12338,#3209,.T.);
#16312=EDGE_CURVE('',#12333,#12919,#3210,.T.);
#16313=EDGE_CURVE('',#12914,#12992,#3211,.T.);
#16314=EDGE_CURVE('',#12992,#12993,#3212,.T.);
#16315=EDGE_CURVE('',#12915,#12993,#3213,.T.);
#16316=EDGE_CURVE('',#12327,#12992,#3214,.T.);
#16317=EDGE_CURVE('',#12993,#12326,#3215,.T.);
#16318=EDGE_CURVE('',#12321,#12913,#3216,.T.);
#16319=EDGE_CURVE('',#12908,#12994,#3217,.T.);
#16320=EDGE_CURVE('',#12994,#12995,#3218,.T.);
#16321=EDGE_CURVE('',#12909,#12995,#3219,.T.);
#16322=EDGE_CURVE('',#12315,#12994,#3220,.T.);
#16323=EDGE_CURVE('',#12995,#12314,#3221,.T.);
#16324=EDGE_CURVE('',#12309,#12907,#3222,.T.);
#16325=EDGE_CURVE('',#12729,#12632,#3223,.T.);
#16326=EDGE_CURVE('',#12902,#12996,#3224,.T.);
#16327=EDGE_CURVE('',#12996,#12997,#3225,.T.);
#16328=EDGE_CURVE('',#12903,#12997,#3226,.T.);
#16329=EDGE_CURVE('',#12303,#12996,#3227,.T.);
#16330=EDGE_CURVE('',#12997,#12302,#3228,.T.);
#16331=EDGE_CURVE('',#12297,#12901,#3229,.T.);
#16332=EDGE_CURVE('',#12896,#12998,#3230,.T.);
#16333=EDGE_CURVE('',#12998,#12999,#3231,.T.);
#16334=EDGE_CURVE('',#12897,#12999,#3232,.T.);
#16335=EDGE_CURVE('',#12291,#12998,#3233,.T.);
#16336=EDGE_CURVE('',#12999,#12290,#3234,.T.);
#16337=EDGE_CURVE('',#12895,#13000,#3235,.T.);
#16338=EDGE_CURVE('',#13000,#13001,#3236,.T.);
#16339=EDGE_CURVE('',#12894,#13001,#3237,.T.);
#16340=EDGE_CURVE('',#12465,#13000,#3238,.T.);
#16341=EDGE_CURVE('',#13001,#12464,#3239,.T.);
#16342=EDGE_CURVE('',#12477,#12656,#3240,.T.);
#16343=EDGE_CURVE('',#12459,#12893,#3241,.T.);
#16344=EDGE_CURVE('',#12716,#13002,#3242,.T.);
#16345=EDGE_CURVE('',#13002,#12482,#3243,.T.);
#16346=EDGE_CURVE('',#13003,#13002,#3244,.T.);
#16347=EDGE_CURVE('',#12483,#13003,#3245,.T.);
#16348=EDGE_CURVE('',#12717,#13003,#3246,.T.);
#16349=EDGE_CURVE('',#12888,#13004,#3247,.T.);
#16350=EDGE_CURVE('',#13004,#13005,#3248,.T.);
#16351=EDGE_CURVE('',#12889,#13005,#3249,.T.);
#16352=EDGE_CURVE('',#12453,#13004,#3250,.T.);
#16353=EDGE_CURVE('',#13005,#12452,#3251,.T.);
#16354=EDGE_CURVE('',#12718,#13006,#3252,.T.);
#16355=EDGE_CURVE('',#13006,#12488,#3253,.T.);
#16356=EDGE_CURVE('',#13007,#13006,#3254,.T.);
#16357=EDGE_CURVE('',#12489,#13007,#3255,.T.);
#16358=EDGE_CURVE('',#12719,#13007,#3256,.T.);
#16359=EDGE_CURVE('',#12447,#12887,#3257,.T.);
#16360=EDGE_CURVE('',#12720,#13008,#3258,.T.);
#16361=EDGE_CURVE('',#13008,#12494,#3259,.T.);
#16362=EDGE_CURVE('',#13009,#13008,#3260,.T.);
#16363=EDGE_CURVE('',#12495,#13009,#3261,.T.);
#16364=EDGE_CURVE('',#12721,#13009,#3262,.T.);
#16365=EDGE_CURVE('',#12882,#13010,#3263,.T.);
#16366=EDGE_CURVE('',#13010,#13011,#3264,.T.);
#16367=EDGE_CURVE('',#12883,#13011,#3265,.T.);
#16368=EDGE_CURVE('',#12441,#13010,#3266,.T.);
#16369=EDGE_CURVE('',#13011,#12440,#3267,.T.);
#16370=EDGE_CURVE('',#12722,#13012,#3268,.T.);
#16371=EDGE_CURVE('',#13012,#12500,#3269,.T.);
#16372=EDGE_CURVE('',#13013,#13012,#3270,.T.);
#16373=EDGE_CURVE('',#12501,#13013,#3271,.T.);
#16374=EDGE_CURVE('',#12723,#13013,#3272,.T.);
#16375=EDGE_CURVE('',#12435,#12881,#3273,.T.);
#16376=EDGE_CURVE('',#12724,#13014,#3274,.T.);
#16377=EDGE_CURVE('',#13014,#12506,#3275,.T.);
#16378=EDGE_CURVE('',#13015,#13014,#3276,.T.);
#16379=EDGE_CURVE('',#12507,#13015,#3277,.T.);
#16380=EDGE_CURVE('',#12725,#13015,#3278,.T.);
#16381=EDGE_CURVE('',#12876,#13016,#3279,.T.);
#16382=EDGE_CURVE('',#13016,#13017,#3280,.T.);
#16383=EDGE_CURVE('',#12877,#13017,#3281,.T.);
#16384=EDGE_CURVE('',#12429,#13016,#3282,.T.);
#16385=EDGE_CURVE('',#13017,#12428,#3283,.T.);
#16386=EDGE_CURVE('',#12726,#13018,#3284,.T.);
#16387=EDGE_CURVE('',#13018,#12512,#3285,.T.);
#16388=EDGE_CURVE('',#13019,#13018,#3286,.T.);
#16389=EDGE_CURVE('',#12513,#13019,#3287,.T.);
#16390=EDGE_CURVE('',#12727,#13019,#3288,.T.);
#16391=EDGE_CURVE('',#13020,#12422,#3289,.T.);
#16392=EDGE_CURVE('',#13021,#13020,#3290,.T.);
#16393=EDGE_CURVE('',#12423,#13021,#3291,.T.);
#16394=EDGE_CURVE('',#12808,#13021,#3292,.T.);
#16395=EDGE_CURVE('',#12809,#13020,#3293,.T.);
#16396=EDGE_CURVE('',#13022,#13023,#10722,.T.);
#16397=EDGE_CURVE('',#13022,#13024,#3294,.T.);
#16398=EDGE_CURVE('',#13024,#13025,#3295,.T.);
#16399=EDGE_CURVE('',#13023,#13025,#3296,.T.);
#16400=EDGE_CURVE('',#13023,#13026,#3297,.T.);
#16401=EDGE_CURVE('',#13025,#13027,#3298,.T.);
#16402=EDGE_CURVE('',#13026,#13027,#3299,.T.);
#16403=EDGE_CURVE('',#13028,#13022,#3300,.T.);
#16404=EDGE_CURVE('',#13028,#13029,#3301,.T.);
#16405=EDGE_CURVE('',#13029,#13024,#3302,.T.);
#16406=EDGE_CURVE('',#13026,#13028,#10723,.T.);
#16407=EDGE_CURVE('',#13027,#13029,#3303,.T.);
#16408=EDGE_CURVE('',#13030,#13031,#11189,.T.);
#16409=EDGE_CURVE('',#13032,#13030,#11190,.T.);
#16410=EDGE_CURVE('',#13032,#13033,#3304,.T.);
#16411=EDGE_CURVE('',#13034,#13033,#11191,.T.);
#16412=EDGE_CURVE('',#13033,#13034,#11192,.T.);
#16413=EDGE_CURVE('',#13031,#13032,#11193,.T.);
#16414=EDGE_CURVE('',#13035,#13035,#10724,.T.);
#16415=EDGE_CURVE('',#13036,#13036,#10725,.T.);
#16416=EDGE_CURVE('',#13036,#13035,#3305,.T.);
#16417=EDGE_CURVE('',#13037,#13037,#10726,.T.);
#16418=EDGE_CURVE('',#13037,#13031,#3306,.T.);
#16419=EDGE_CURVE('',#13032,#13036,#3307,.T.);
#16420=EDGE_CURVE('',#13038,#13038,#10727,.T.);
#16421=EDGE_CURVE('',#13038,#13037,#3308,.T.);
#16422=EDGE_CURVE('',#13039,#13039,#10728,.T.);
#16423=EDGE_CURVE('',#13039,#13038,#3309,.T.);
#16424=EDGE_CURVE('',#13040,#13040,#10729,.T.);
#16425=EDGE_CURVE('',#13041,#13041,#10730,.T.);
#16426=EDGE_CURVE('',#13041,#13040,#3310,.T.);
#16427=EDGE_CURVE('',#13042,#13042,#10731,.T.);
#16428=EDGE_CURVE('',#13043,#13043,#10732,.T.);
#16429=EDGE_CURVE('',#13043,#13042,#3311,.T.);
#16430=EDGE_CURVE('',#13044,#13044,#10733,.T.);
#16431=EDGE_CURVE('',#13045,#13045,#10734,.T.);
#16432=EDGE_CURVE('',#13045,#13044,#3312,.T.);
#16433=EDGE_CURVE('',#13046,#13046,#10735,.T.);
#16434=EDGE_CURVE('',#13047,#13047,#10736,.T.);
#16435=EDGE_CURVE('',#13047,#13046,#3313,.T.);
#16436=EDGE_CURVE('',#13048,#13048,#10737,.T.);
#16437=EDGE_CURVE('',#13049,#13049,#10738,.T.);
#16438=EDGE_CURVE('',#13049,#13048,#3314,.T.);
#16439=EDGE_CURVE('',#13050,#13050,#10739,.T.);
#16440=EDGE_CURVE('',#13050,#13049,#3315,.T.);
#16441=EDGE_CURVE('',#13051,#13051,#10740,.T.);
#16442=EDGE_CURVE('',#13051,#13052,#3316,.T.);
#16443=EDGE_CURVE('',#13052,#13052,#10741,.T.);
#16444=EDGE_CURVE('',#13053,#13053,#10742,.T.);
#16445=EDGE_CURVE('',#13053,#13054,#3317,.T.);
#16446=EDGE_CURVE('',#13054,#13054,#10743,.T.);
#16447=EDGE_CURVE('',#13055,#13055,#10744,.T.);
#16448=EDGE_CURVE('',#13056,#13056,#10745,.T.);
#16449=EDGE_CURVE('',#13056,#13055,#3318,.T.);
#16450=EDGE_CURVE('',#13057,#13057,#10746,.T.);
#16451=EDGE_CURVE('',#13057,#13056,#3319,.T.);
#16452=EDGE_CURVE('',#13058,#13058,#10747,.T.);
#16453=EDGE_CURVE('',#13058,#13057,#3320,.T.);
#16454=EDGE_CURVE('',#13059,#13059,#10748,.T.);
#16455=EDGE_CURVE('',#13059,#13060,#3321,.T.);
#16456=EDGE_CURVE('',#13060,#13060,#10749,.T.);
#16457=EDGE_CURVE('',#13061,#13061,#10750,.T.);
#16458=EDGE_CURVE('',#13062,#13062,#10751,.T.);
#16459=EDGE_CURVE('',#13062,#13061,#3322,.T.);
#16460=EDGE_CURVE('',#13063,#13063,#10752,.T.);
#16461=EDGE_CURVE('',#13063,#13064,#3323,.T.);
#16462=EDGE_CURVE('',#13064,#13064,#10753,.T.);
#16463=EDGE_CURVE('',#13064,#13065,#3324,.T.);
#16464=EDGE_CURVE('',#13065,#13065,#10754,.T.);
#16465=EDGE_CURVE('',#13065,#13066,#3325,.T.);
#16466=EDGE_CURVE('',#13066,#13066,#10755,.T.);
#16467=EDGE_CURVE('',#13067,#13067,#10756,.T.);
#16468=EDGE_CURVE('',#13067,#13068,#3326,.T.);
#16469=EDGE_CURVE('',#13068,#13069,#10757,.T.);
#16470=EDGE_CURVE('',#13069,#13068,#10758,.T.);
#16471=EDGE_CURVE('',#13069,#13070,#3327,.T.);
#16472=EDGE_CURVE('',#13070,#13070,#10759,.T.);
#16473=EDGE_CURVE('',#13071,#13071,#10760,.T.);
#16474=EDGE_CURVE('',#13072,#13072,#10761,.T.);
#16475=EDGE_CURVE('',#13072,#13073,#3328,.T.);
#16476=EDGE_CURVE('',#13073,#13073,#10762,.T.);
#16477=EDGE_CURVE('',#13074,#13074,#10763,.T.);
#16478=EDGE_CURVE('',#13070,#13074,#3329,.T.);
#16479=EDGE_CURVE('',#13075,#13075,#10764,.T.);
#16480=EDGE_CURVE('',#13075,#13071,#3330,.T.);
#16481=EDGE_CURVE('',#13076,#13076,#10765,.T.);
#16482=EDGE_CURVE('',#13076,#13077,#3331,.T.);
#16483=EDGE_CURVE('',#13077,#13077,#10766,.T.);
#16484=EDGE_CURVE('',#13078,#13078,#10767,.T.);
#16485=EDGE_CURVE('',#13078,#13079,#3332,.T.);
#16486=EDGE_CURVE('',#13079,#13079,#10768,.T.);
#16487=EDGE_CURVE('',#13080,#13080,#10769,.T.);
#16488=EDGE_CURVE('',#13081,#13081,#10770,.T.);
#16489=EDGE_CURVE('',#13081,#13080,#3333,.T.);
#16490=EDGE_CURVE('',#13082,#13082,#10771,.T.);
#16491=EDGE_CURVE('',#13082,#13081,#3334,.T.);
#16492=EDGE_CURVE('',#13083,#13083,#10772,.T.);
#16493=EDGE_CURVE('',#13084,#13084,#10773,.T.);
#16494=EDGE_CURVE('',#13084,#13083,#3335,.T.);
#16495=EDGE_CURVE('',#13085,#13085,#10774,.T.);
#16496=EDGE_CURVE('',#13085,#13084,#3336,.T.);
#16497=EDGE_CURVE('',#13086,#13086,#10775,.T.);
#16498=EDGE_CURVE('',#13086,#13085,#3337,.T.);
#16499=EDGE_CURVE('',#13087,#13087,#10776,.T.);
#16500=EDGE_CURVE('',#13087,#13088,#3338,.T.);
#16501=EDGE_CURVE('',#13088,#13088,#10777,.T.);
#16502=EDGE_CURVE('',#13089,#13089,#10778,.T.);
#16503=EDGE_CURVE('',#13090,#13090,#10779,.T.);
#16504=EDGE_CURVE('',#13090,#13089,#3339,.T.);
#16505=EDGE_CURVE('',#13091,#13091,#10780,.T.);
#16506=EDGE_CURVE('',#13091,#13091,#10781,.T.);
#16507=EDGE_CURVE('',#13092,#13093,#3340,.T.);
#16508=EDGE_CURVE('',#13093,#13094,#330,.T.);
#16509=EDGE_CURVE('',#13094,#13095,#3341,.T.);
#16510=EDGE_CURVE('',#13095,#13092,#11194,.T.);
#16511=EDGE_CURVE('',#13095,#13096,#10782,.T.);
#16512=EDGE_CURVE('',#13096,#13097,#11195,.T.);
#16513=EDGE_CURVE('',#13097,#13092,#10783,.T.);
#16514=EDGE_CURVE('',#13096,#13098,#3342,.T.);
#16515=EDGE_CURVE('',#13098,#13099,#331,.T.);
#16516=EDGE_CURVE('',#13099,#13097,#3343,.T.);
#16517=EDGE_CURVE('',#13094,#13098,#10784,.T.);
#16518=EDGE_CURVE('',#13100,#13101,#3344,.T.);
#16519=EDGE_CURVE('',#13101,#13102,#332,.T.);
#16520=EDGE_CURVE('',#13102,#13103,#3345,.T.);
#16521=EDGE_CURVE('',#13103,#13100,#11196,.T.);
#16522=EDGE_CURVE('',#13104,#13105,#3346,.T.);
#16523=EDGE_CURVE('',#13105,#13106,#333,.T.);
#16524=EDGE_CURVE('',#13106,#13107,#3347,.T.);
#16525=EDGE_CURVE('',#13107,#13104,#11197,.T.);
#16526=EDGE_CURVE('',#13103,#13104,#10785,.T.);
#16527=EDGE_CURVE('',#13107,#13100,#10786,.T.);
#16528=EDGE_CURVE('',#13106,#13101,#10787,.T.);
#16529=EDGE_CURVE('',#13105,#13099,#3348,.T.);
#16530=EDGE_CURVE('',#13104,#13097,#3349,.T.);
#16531=EDGE_CURVE('',#13103,#13092,#3350,.T.);
#16532=EDGE_CURVE('',#13102,#13093,#3351,.T.);
#16533=EDGE_CURVE('',#13108,#13109,#3352,.T.);
#16534=EDGE_CURVE('',#13110,#13108,#3353,.T.);
#16535=EDGE_CURVE('',#13109,#13110,#163,.F.);
#16536=EDGE_CURVE('',#13111,#13112,#3354,.T.);
#16537=EDGE_CURVE('',#13113,#13111,#3355,.T.);
#16538=EDGE_CURVE('',#13112,#13113,#164,.F.);
#16539=EDGE_CURVE('',#13114,#13115,#334,.T.);
#16540=EDGE_CURVE('',#13115,#13113,#3356,.T.);
#16541=EDGE_CURVE('',#13111,#13114,#3357,.T.);
#16542=EDGE_CURVE('',#13116,#13117,#165,.F.);
#16543=EDGE_CURVE('',#13118,#13116,#3358,.T.);
#16544=EDGE_CURVE('',#13117,#13118,#3359,.T.);
#16545=EDGE_CURVE('',#13119,#13120,#3360,.T.);
#16546=EDGE_CURVE('',#13121,#13119,#166,.F.);
#16547=EDGE_CURVE('',#13120,#13121,#3361,.T.);
#16548=EDGE_CURVE('',#13113,#13121,#10788,.T.);
#16549=EDGE_CURVE('',#13119,#13112,#10789,.T.);
#16550=EDGE_CURVE('',#13122,#13123,#335,.T.);
#16551=EDGE_CURVE('',#13123,#13120,#3362,.T.);
#16552=EDGE_CURVE('',#13121,#13122,#3363,.T.);
#16553=EDGE_CURVE('',#13116,#13119,#3364,.T.);
#16554=EDGE_CURVE('',#13120,#13118,#3365,.T.);
#16555=EDGE_CURVE('',#13124,#13125,#336,.T.);
#16556=EDGE_CURVE('',#13125,#13117,#3366,.T.);
#16557=EDGE_CURVE('',#13118,#13124,#3367,.T.);
#16558=EDGE_CURVE('',#13117,#13109,#10790,.T.);
#16559=EDGE_CURVE('',#13110,#13116,#10791,.T.);
#16560=EDGE_CURVE('',#13108,#13111,#3368,.T.);
#16561=EDGE_CURVE('',#13112,#13110,#3369,.T.);
#16562=EDGE_CURVE('',#13126,#13127,#337,.T.);
#16563=EDGE_CURVE('',#13127,#13108,#3370,.T.);
#16564=EDGE_CURVE('',#13109,#13126,#3371,.T.);
#16565=EDGE_CURVE('',#13122,#13115,#10792,.T.);
#16566=EDGE_CURVE('',#13114,#13127,#3372,.T.);
#16567=EDGE_CURVE('',#13125,#13126,#10793,.T.);
#16568=EDGE_CURVE('',#13123,#13124,#3373,.T.);
#16569=EDGE_CURVE('',#13128,#13128,#10794,.T.);
#16570=EDGE_CURVE('',#13128,#13129,#3374,.T.);
#16571=EDGE_CURVE('',#13129,#13129,#10795,.T.);
#16572=EDGE_CURVE('',#13130,#13131,#11198,.T.);
#16573=EDGE_CURVE('',#13132,#13130,#11199,.T.);
#16574=EDGE_CURVE('',#13133,#13132,#11200,.T.);
#16575=EDGE_CURVE('',#13134,#13133,#11201,.T.);
#16576=EDGE_CURVE('',#13135,#13134,#11202,.T.);
#16577=EDGE_CURVE('',#13135,#13129,#3375,.T.);
#16578=EDGE_CURVE('',#13136,#13135,#11203,.T.);
#16579=EDGE_CURVE('',#13131,#13136,#11204,.T.);
#16580=EDGE_CURVE('',#13137,#13138,#3376,.T.);
#16581=EDGE_CURVE('',#13134,#13137,#11205,.F.);
#16582=EDGE_CURVE('',#13138,#13134,#11206,.F.);
#16583=EDGE_CURVE('',#13133,#13139,#11207,.F.);
#16584=EDGE_CURVE('',#13140,#13133,#11208,.F.);
#16585=EDGE_CURVE('',#13139,#13140,#3377,.T.);
#16586=EDGE_CURVE('',#13141,#13142,#3378,.T.);
#16587=EDGE_CURVE('',#13136,#13141,#11209,.F.);
#16588=EDGE_CURVE('',#13142,#13136,#11210,.F.);
#16589=EDGE_CURVE('',#13132,#13143,#11211,.F.);
#16590=EDGE_CURVE('',#13144,#13132,#11212,.F.);
#16591=EDGE_CURVE('',#13143,#13144,#3379,.T.);
#16592=EDGE_CURVE('',#13145,#13146,#3380,.T.);
#16593=EDGE_CURVE('',#13131,#13145,#11213,.F.);
#16594=EDGE_CURVE('',#13146,#13131,#11214,.F.);
#16595=EDGE_CURVE('',#13130,#13147,#11215,.F.);
#16596=EDGE_CURVE('',#13148,#13130,#11216,.F.);
#16597=EDGE_CURVE('',#13147,#13148,#3381,.T.);
#16598=EDGE_CURVE('',#13145,#13148,#11217,.T.);
#16599=EDGE_CURVE('',#13149,#13150,#3382,.T.);
#16600=EDGE_CURVE('',#13150,#13147,#3383,.T.);
#16601=EDGE_CURVE('',#13148,#13149,#3384,.T.);
#16602=EDGE_CURVE('',#13147,#13144,#11218,.T.);
#16603=EDGE_CURVE('',#13141,#13146,#11219,.T.);
#16604=EDGE_CURVE('',#13151,#13152,#3385,.T.);
#16605=EDGE_CURVE('',#13152,#13145,#3386,.T.);
#16606=EDGE_CURVE('',#13146,#13151,#3387,.T.);
#16607=EDGE_CURVE('',#13153,#13154,#3388,.T.);
#16608=EDGE_CURVE('',#13154,#13143,#3389,.T.);
#16609=EDGE_CURVE('',#13144,#13153,#3390,.T.);
#16610=EDGE_CURVE('',#13143,#13140,#11220,.T.);
#16611=EDGE_CURVE('',#13137,#13142,#11221,.T.);
#16612=EDGE_CURVE('',#13155,#13156,#3391,.T.);
#16613=EDGE_CURVE('',#13156,#13141,#3392,.T.);
#16614=EDGE_CURVE('',#13142,#13155,#3393,.T.);
#16615=EDGE_CURVE('',#13157,#13158,#3394,.T.);
#16616=EDGE_CURVE('',#13158,#13139,#3395,.T.);
#16617=EDGE_CURVE('',#13140,#13157,#3396,.T.);
#16618=EDGE_CURVE('',#13139,#13138,#11222,.T.);
#16619=EDGE_CURVE('',#13159,#13160,#3397,.T.);
#16620=EDGE_CURVE('',#13160,#13137,#3398,.T.);
#16621=EDGE_CURVE('',#13138,#13159,#3399,.T.);
#16622=EDGE_CURVE('',#13161,#13151,#3400,.T.);
#16623=EDGE_CURVE('',#13161,#13162,#10796,.T.);
#16624=EDGE_CURVE('',#13152,#13162,#3401,.T.);
#16625=EDGE_CURVE('',#13156,#13163,#3402,.T.);
#16626=EDGE_CURVE('',#13161,#13163,#3403,.T.);
#16627=EDGE_CURVE('',#13164,#13155,#3404,.T.);
#16628=EDGE_CURVE('',#13164,#13163,#10797,.T.);
#16629=EDGE_CURVE('',#13160,#13165,#3405,.T.);
#16630=EDGE_CURVE('',#13164,#13165,#3406,.T.);
#16631=EDGE_CURVE('',#13166,#13159,#3407,.T.);
#16632=EDGE_CURVE('',#13166,#13165,#10798,.T.);
#16633=EDGE_CURVE('',#13158,#13167,#3408,.T.);
#16634=EDGE_CURVE('',#13166,#13167,#3409,.T.);
#16635=EDGE_CURVE('',#13154,#13168,#3410,.T.);
#16636=EDGE_CURVE('',#13169,#13168,#3411,.T.);
#16637=EDGE_CURVE('',#13169,#13157,#3412,.T.);
#16638=EDGE_CURVE('',#13150,#13170,#3413,.T.);
#16639=EDGE_CURVE('',#13171,#13170,#3414,.T.);
#16640=EDGE_CURVE('',#13171,#13153,#3415,.T.);
#16641=EDGE_CURVE('',#13172,#13149,#3416,.T.);
#16642=EDGE_CURVE('',#13172,#13170,#10799,.T.);
#16643=EDGE_CURVE('',#13171,#13168,#10800,.T.);
#16644=EDGE_CURVE('',#13169,#13167,#10801,.T.);
#16645=EDGE_CURVE('',#13172,#13162,#3417,.T.);
#16646=EDGE_CURVE('',#13167,#13166,#10802,.T.);
#16647=EDGE_CURVE('',#13168,#13169,#10803,.T.);
#16648=EDGE_CURVE('',#13170,#13171,#10804,.T.);
#16649=EDGE_CURVE('',#13162,#13172,#10805,.T.);
#16650=EDGE_CURVE('',#13163,#13161,#10806,.T.);
#16651=EDGE_CURVE('',#13165,#13173,#10807,.T.);
#16652=EDGE_CURVE('',#13173,#13164,#10808,.T.);
#16653=EDGE_CURVE('',#13174,#13174,#10809,.T.);
#16654=EDGE_CURVE('',#13175,#13175,#10810,.T.);
#16655=EDGE_CURVE('',#13175,#13174,#3418,.T.);
#16656=EDGE_CURVE('',#13173,#13175,#3419,.T.);
#16657=EDGE_CURVE('',#13176,#13177,#3420,.T.);
#16658=EDGE_CURVE('',#13177,#13178,#3421,.T.);
#16659=EDGE_CURVE('',#13178,#13179,#3422,.T.);
#16660=EDGE_CURVE('',#13179,#13176,#3423,.T.);
#16661=EDGE_CURVE('',#13180,#13181,#3424,.T.);
#16662=EDGE_CURVE('',#13181,#13177,#10811,.T.);
#16663=EDGE_CURVE('',#13176,#13180,#10812,.T.);
#16664=EDGE_CURVE('',#13182,#13183,#3425,.T.);
#16665=EDGE_CURVE('',#13183,#13181,#3426,.T.);
#16666=EDGE_CURVE('',#13180,#13182,#3427,.T.);
#16667=EDGE_CURVE('',#13184,#13185,#3428,.T.);
#16668=EDGE_CURVE('',#13185,#13183,#10813,.T.);
#16669=EDGE_CURVE('',#13182,#13184,#10814,.T.);
#16670=EDGE_CURVE('',#13186,#13187,#3429,.T.);
#16671=EDGE_CURVE('',#13187,#13185,#3430,.T.);
#16672=EDGE_CURVE('',#13184,#13186,#3431,.T.);
#16673=EDGE_CURVE('',#13188,#13189,#3432,.T.);
#16674=EDGE_CURVE('',#13189,#13187,#10815,.T.);
#16675=EDGE_CURVE('',#13186,#13188,#10816,.T.);
#16676=EDGE_CURVE('',#13190,#13191,#3433,.T.);
#16677=EDGE_CURVE('',#13191,#13189,#3434,.T.);
#16678=EDGE_CURVE('',#13188,#13190,#3435,.T.);
#16679=EDGE_CURVE('',#13178,#13191,#10817,.T.);
#16680=EDGE_CURVE('',#13190,#13179,#10818,.T.);
#16681=EDGE_CURVE('',#13192,#13182,#3436,.T.);
#16682=EDGE_CURVE('',#13193,#13192,#10819,.T.);
#16683=EDGE_CURVE('',#13193,#13184,#3437,.T.);
#16684=EDGE_CURVE('',#13194,#13180,#3438,.T.);
#16685=EDGE_CURVE('',#13192,#13194,#3439,.T.);
#16686=EDGE_CURVE('',#13195,#13176,#3440,.T.);
#16687=EDGE_CURVE('',#13194,#13195,#10820,.T.);
#16688=EDGE_CURVE('',#13196,#13179,#3441,.T.);
#16689=EDGE_CURVE('',#13195,#13196,#3442,.T.);
#16690=EDGE_CURVE('',#13197,#13197,#10821,.T.);
#16691=EDGE_CURVE('',#13198,#13198,#10822,.T.);
#16692=EDGE_CURVE('',#13199,#13199,#10823,.T.);
#16693=EDGE_CURVE('',#13200,#13200,#10824,.T.);
#16694=EDGE_CURVE('',#13201,#13202,#3443,.T.);
#16695=EDGE_CURVE('',#13202,#13203,#10825,.T.);
#16696=EDGE_CURVE('',#13203,#13204,#3444,.T.);
#16697=EDGE_CURVE('',#13204,#13205,#10826,.T.);
#16698=EDGE_CURVE('',#13205,#13206,#3445,.T.);
#16699=EDGE_CURVE('',#13206,#13207,#10827,.T.);
#16700=EDGE_CURVE('',#13207,#13208,#3446,.T.);
#16701=EDGE_CURVE('',#13208,#13201,#10828,.T.);
#16702=EDGE_CURVE('',#13196,#13209,#3447,.T.);
#16703=EDGE_CURVE('',#13209,#13210,#3448,.T.);
#16704=EDGE_CURVE('',#13210,#13195,#3449,.T.);
#16705=EDGE_CURVE('',#13211,#13212,#3450,.T.);
#16706=EDGE_CURVE('',#13212,#13209,#10829,.T.);
#16707=EDGE_CURVE('',#13196,#13211,#10830,.T.);
#16708=EDGE_CURVE('',#13213,#13214,#3451,.T.);
#16709=EDGE_CURVE('',#13214,#13212,#3452,.T.);
#16710=EDGE_CURVE('',#13211,#13213,#3453,.T.);
#16711=EDGE_CURVE('',#13215,#13216,#3454,.T.);
#16712=EDGE_CURVE('',#13216,#13214,#10831,.T.);
#16713=EDGE_CURVE('',#13213,#13215,#10832,.T.);
#16714=EDGE_CURVE('',#13193,#13217,#3455,.T.);
#16715=EDGE_CURVE('',#13217,#13216,#3456,.T.);
#16716=EDGE_CURVE('',#13215,#13193,#3457,.T.);
#16717=EDGE_CURVE('',#13192,#13218,#3458,.T.);
#16718=EDGE_CURVE('',#13218,#13217,#10833,.T.);
#16719=EDGE_CURVE('',#13194,#13219,#3459,.T.);
#16720=EDGE_CURVE('',#13219,#13218,#3460,.T.);
#16721=EDGE_CURVE('',#13210,#13219,#10834,.T.);
#16722=EDGE_CURVE('',#13215,#13186,#3461,.T.);
#16723=EDGE_CURVE('',#13213,#13188,#3462,.T.);
#16724=EDGE_CURVE('',#13211,#13190,#3463,.T.);
#16725=EDGE_CURVE('',#13220,#13220,#10835,.T.);
#16726=EDGE_CURVE('',#13221,#13221,#10836,.T.);
#16727=EDGE_CURVE('',#13222,#13222,#10837,.T.);
#16728=EDGE_CURVE('',#13223,#13223,#10838,.T.);
#16729=EDGE_CURVE('',#13224,#13225,#3464,.T.);
#16730=EDGE_CURVE('',#13225,#13226,#3465,.T.);
#16731=EDGE_CURVE('',#13226,#13227,#3466,.T.);
#16732=EDGE_CURVE('',#13227,#13224,#3467,.T.);
#16733=EDGE_CURVE('',#13228,#13229,#3468,.T.);
#16734=EDGE_CURVE('',#13229,#13225,#10839,.T.);
#16735=EDGE_CURVE('',#13224,#13228,#10840,.T.);
#16736=EDGE_CURVE('',#13230,#13231,#3469,.T.);
#16737=EDGE_CURVE('',#13231,#13229,#3470,.T.);
#16738=EDGE_CURVE('',#13228,#13230,#3471,.T.);
#16739=EDGE_CURVE('',#13232,#13233,#3472,.T.);
#16740=EDGE_CURVE('',#13233,#13231,#10841,.T.);
#16741=EDGE_CURVE('',#13230,#13232,#10842,.T.);
#16742=EDGE_CURVE('',#13234,#13235,#3473,.T.);
#16743=EDGE_CURVE('',#13235,#13233,#3474,.T.);
#16744=EDGE_CURVE('',#13232,#13234,#3475,.T.);
#16745=EDGE_CURVE('',#13236,#13237,#3476,.T.);
#16746=EDGE_CURVE('',#13237,#13235,#10843,.T.);
#16747=EDGE_CURVE('',#13234,#13236,#10844,.T.);
#16748=EDGE_CURVE('',#13238,#13239,#3477,.T.);
#16749=EDGE_CURVE('',#13239,#13237,#3478,.T.);
#16750=EDGE_CURVE('',#13236,#13238,#3479,.T.);
#16751=EDGE_CURVE('',#13226,#13239,#10845,.T.);
#16752=EDGE_CURVE('',#13238,#13227,#10846,.T.);
#16753=EDGE_CURVE('',#13207,#13230,#3480,.T.);
#16754=EDGE_CURVE('',#13206,#13232,#3481,.T.);
#16755=EDGE_CURVE('',#13208,#13228,#3482,.T.);
#16756=EDGE_CURVE('',#13201,#13224,#3483,.T.);
#16757=EDGE_CURVE('',#13202,#13227,#3484,.T.);
#16758=EDGE_CURVE('',#13203,#13238,#3485,.T.);
#16759=EDGE_CURVE('',#13204,#13236,#3486,.T.);
#16760=EDGE_CURVE('',#13205,#13234,#3487,.T.);
#16761=EDGE_CURVE('',#13223,#13200,#3488,.T.);
#16762=EDGE_CURVE('',#13222,#13199,#3489,.T.);
#16763=EDGE_CURVE('',#13221,#13198,#3490,.T.);
#16764=EDGE_CURVE('',#13220,#13197,#3491,.T.);
#16765=EDGE_CURVE('',#13240,#13241,#167,.F.);
#16766=EDGE_CURVE('',#13241,#13242,#10847,.T.);
#16767=EDGE_CURVE('',#13242,#13243,#10848,.T.);
#16768=EDGE_CURVE('',#13243,#13244,#168,.F.);
#16769=EDGE_CURVE('',#13244,#13240,#10849,.T.);
#16770=EDGE_CURVE('',#13243,#13245,#169,.T.);
#16771=EDGE_CURVE('',#13242,#13246,#3492,.T.);
#16772=EDGE_CURVE('',#13247,#13246,#10850,.T.);
#16773=EDGE_CURVE('',#13246,#13247,#10851,.T.);
#16774=EDGE_CURVE('',#13248,#13241,#170,.T.);
#16775=EDGE_CURVE('',#13248,#13249,#171,.T.);
#16776=EDGE_CURVE('',#13249,#13250,#172,.T.);
#16777=EDGE_CURVE('',#13251,#13250,#10852,.T.);
#16778=EDGE_CURVE('',#13252,#13251,#173,.T.);
#16779=EDGE_CURVE('',#13253,#13252,#10853,.T.);
#16780=EDGE_CURVE('',#13254,#13253,#174,.T.);
#16781=EDGE_CURVE('',#13254,#13255,#175,.T.);
#16782=EDGE_CURVE('',#13255,#13256,#176,.T.);
#16783=EDGE_CURVE('',#13257,#13256,#10854,.T.);
#16784=EDGE_CURVE('',#13258,#13257,#177,.F.);
#16785=EDGE_CURVE('',#13258,#13259,#178,.T.);
#16786=EDGE_CURVE('',#13260,#13259,#179,.T.);
#16787=EDGE_CURVE('',#13261,#13260,#10855,.T.);
#16788=EDGE_CURVE('',#13262,#13261,#180,.T.);
#16789=EDGE_CURVE('',#13262,#13263,#181,.T.);
#16790=EDGE_CURVE('',#13263,#13264,#182,.T.);
#16791=EDGE_CURVE('',#13265,#13264,#10856,.T.);
#16792=EDGE_CURVE('',#13266,#13265,#183,.F.);
#16793=EDGE_CURVE('',#13266,#13245,#184,.T.);
#16794=EDGE_CURVE('',#13267,#13268,#10857,.T.);
#16795=EDGE_CURVE('',#13268,#13267,#10858,.T.);
#16796=EDGE_CURVE('',#13267,#13269,#3493,.T.);
#16797=EDGE_CURVE('',#13269,#13269,#10859,.T.);
#16798=EDGE_CURVE('',#13270,#13271,#10860,.T.);
#16799=EDGE_CURVE('',#13271,#13270,#10861,.T.);
#16800=EDGE_CURVE('',#13271,#13268,#3494,.T.);
#16801=EDGE_CURVE('',#13272,#13272,#10862,.T.);
#16802=EDGE_CURVE('',#13252,#13273,#185,.F.);
#16803=EDGE_CURVE('',#13273,#13274,#10863,.T.);
#16804=EDGE_CURVE('',#13274,#13253,#186,.F.);
#16805=EDGE_CURVE('',#13275,#13261,#187,.F.);
#16806=EDGE_CURVE('',#13260,#13276,#188,.F.);
#16807=EDGE_CURVE('',#13276,#13275,#10864,.T.);
#16808=EDGE_CURVE('',#13277,#13278,#3495,.T.);
#16809=EDGE_CURVE('',#13279,#13277,#3496,.T.);
#16810=EDGE_CURVE('',#13278,#13279,#3497,.T.);
#16811=EDGE_CURVE('',#13280,#13281,#3498,.F.);
#16812=EDGE_CURVE('',#13281,#13279,#3499,.T.);
#16813=EDGE_CURVE('',#13277,#13280,#3500,.T.);
#16814=EDGE_CURVE('',#13282,#13283,#3501,.T.);
#16815=EDGE_CURVE('',#13284,#13282,#3502,.T.);
#16816=EDGE_CURVE('',#13283,#13284,#3503,.T.);
#16817=EDGE_CURVE('',#13285,#13286,#3504,.T.);
#16818=EDGE_CURVE('',#13287,#13285,#3505,.T.);
#16819=EDGE_CURVE('',#13286,#13287,#3506,.T.);
#16820=EDGE_CURVE('',#13288,#13289,#3507,.F.);
#16821=EDGE_CURVE('',#13289,#13287,#3508,.T.);
#16822=EDGE_CURVE('',#13285,#13288,#3509,.T.);
#16823=EDGE_CURVE('',#13278,#13286,#3510,.T.);
#16824=EDGE_CURVE('',#13287,#13277,#3511,.T.);
#16825=EDGE_CURVE('',#13290,#13291,#3512,.T.);
#16826=EDGE_CURVE('',#13292,#13290,#3513,.T.);
#16827=EDGE_CURVE('',#13291,#13292,#3514,.T.);
#16828=EDGE_CURVE('',#13257,#13292,#3515,.T.);
#16829=EDGE_CURVE('',#13290,#13258,#3516,.T.);
#16830=EDGE_CURVE('',#13293,#13294,#3517,.T.);
#16831=EDGE_CURVE('',#13295,#13293,#3518,.T.);
#16832=EDGE_CURVE('',#13294,#13295,#3519,.T.);
#16833=EDGE_CURVE('',#13296,#13297,#3520,.T.);
#16834=EDGE_CURVE('',#13298,#13296,#3521,.T.);
#16835=EDGE_CURVE('',#13297,#13298,#3522,.T.);
#16836=EDGE_CURVE('',#13296,#13291,#3523,.T.);
#16837=EDGE_CURVE('',#13292,#13298,#3524,.T.);
#16838=EDGE_CURVE('',#13255,#13297,#3525,.T.);
#16839=EDGE_CURVE('',#13298,#13256,#3526,.T.);
#16840=EDGE_CURVE('',#13293,#13296,#3527,.T.);
#16841=EDGE_CURVE('',#13297,#13295,#3528,.T.);
#16842=EDGE_CURVE('',#13286,#13294,#3529,.T.);
#16843=EDGE_CURVE('',#13295,#13285,#3530,.T.);
#16844=EDGE_CURVE('',#13294,#13283,#3531,.T.);
#16845=EDGE_CURVE('',#13284,#13293,#3532,.T.);
#16846=EDGE_CURVE('',#13282,#13290,#3533,.T.);
#16847=EDGE_CURVE('',#13291,#13284,#3534,.T.);
#16848=EDGE_CURVE('',#13283,#13278,#3535,.T.);
#16849=EDGE_CURVE('',#13279,#13282,#3536,.T.);
#16850=EDGE_CURVE('',#13276,#13281,#3537,.T.);
#16851=EDGE_CURVE('',#13280,#13289,#3538,.T.);
#16852=EDGE_CURVE('',#13299,#13300,#10865,.T.);
#16853=EDGE_CURVE('',#13300,#13299,#10866,.T.);
#16854=EDGE_CURVE('',#13299,#13270,#3539,.T.);
#16855=EDGE_CURVE('',#13301,#13302,#10867,.T.);
#16856=EDGE_CURVE('',#13302,#13301,#10868,.T.);
#16857=EDGE_CURVE('',#13302,#13300,#3540,.T.);
#16858=EDGE_CURVE('',#13303,#13303,#11223,.T.);
#16859=EDGE_CURVE('',#13247,#13301,#3541,.T.);
#16860=EDGE_CURVE('',#13304,#13305,#3542,.T.);
#16861=EDGE_CURVE('',#13306,#13304,#3543,.T.);
#16862=EDGE_CURVE('',#13305,#13306,#3544,.T.);
#16863=EDGE_CURVE('',#13307,#13308,#3545,.F.);
#16864=EDGE_CURVE('',#13308,#13306,#3546,.T.);
#16865=EDGE_CURVE('',#13304,#13307,#3547,.T.);
#16866=EDGE_CURVE('',#13309,#13310,#3548,.T.);
#16867=EDGE_CURVE('',#13310,#13305,#3549,.T.);
#16868=EDGE_CURVE('',#13306,#13311,#3550,.T.);
#16869=EDGE_CURVE('',#13311,#13309,#3551,.T.);
#16870=EDGE_CURVE('',#13312,#13313,#3552,.T.);
#16871=EDGE_CURVE('',#13313,#13304,#3553,.T.);
#16872=EDGE_CURVE('',#13305,#13314,#3554,.T.);
#16873=EDGE_CURVE('',#13314,#13312,#3555,.T.);
#16874=EDGE_CURVE('',#13273,#13308,#3556,.T.);
#16875=EDGE_CURVE('',#13251,#13315,#3557,.T.);
#16876=EDGE_CURVE('',#13316,#13315,#3558,.T.);
#16877=EDGE_CURVE('',#13311,#13316,#3559,.T.);
#16878=EDGE_CURVE('',#13317,#13313,#3560,.T.);
#16879=EDGE_CURVE('',#13307,#13317,#3561,.T.);
#16880=EDGE_CURVE('',#13312,#13318,#3562,.T.);
#16881=EDGE_CURVE('',#13318,#13319,#3563,.T.);
#16882=EDGE_CURVE('',#13319,#13317,#3564,.F.);
#16883=EDGE_CURVE('',#13320,#13321,#3565,.T.);
#16884=EDGE_CURVE('',#13322,#13320,#3566,.T.);
#16885=EDGE_CURVE('',#13321,#13322,#3567,.T.);
#16886=EDGE_CURVE('',#13323,#13324,#3568,.T.);
#16887=EDGE_CURVE('',#13325,#13323,#3569,.T.);
#16888=EDGE_CURVE('',#13324,#13325,#3570,.T.);
#16889=EDGE_CURVE('',#13315,#13325,#3571,.T.);
#16890=EDGE_CURVE('',#13323,#13326,#3572,.T.);
#16891=EDGE_CURVE('',#13326,#13316,#3573,.T.);
#16892=EDGE_CURVE('',#13249,#13324,#3574,.T.);
#16893=EDGE_CURVE('',#13325,#13250,#3575,.T.);
#16894=EDGE_CURVE('',#13320,#13323,#3576,.T.);
#16895=EDGE_CURVE('',#13324,#13322,#3577,.T.);
#16896=EDGE_CURVE('',#13314,#13321,#3578,.T.);
#16897=EDGE_CURVE('',#13322,#13318,#3579,.T.);
#16898=EDGE_CURVE('',#13327,#13309,#3580,.T.);
#16899=EDGE_CURVE('',#13327,#13320,#3581,.T.);
#16900=EDGE_CURVE('',#13321,#13310,#3582,.T.);
#16901=EDGE_CURVE('',#13326,#13327,#3583,.T.);
#16902=EDGE_CURVE('',#13319,#13240,#3584,.T.);
#16903=EDGE_CURVE('',#13328,#13329,#3585,.T.);
#16904=EDGE_CURVE('',#13330,#13328,#3586,.T.);
#16905=EDGE_CURVE('',#13329,#13330,#3587,.T.);
#16906=EDGE_CURVE('',#13331,#13332,#3588,.F.);
#16907=EDGE_CURVE('',#13332,#13330,#3589,.T.);
#16908=EDGE_CURVE('',#13328,#13331,#3590,.T.);
#16909=EDGE_CURVE('',#13333,#13334,#3591,.T.);
#16910=EDGE_CURVE('',#13335,#13333,#3592,.T.);
#16911=EDGE_CURVE('',#13334,#13335,#3593,.T.);
#16912=EDGE_CURVE('',#13336,#13337,#3594,.T.);
#16913=EDGE_CURVE('',#13338,#13336,#3595,.T.);
#16914=EDGE_CURVE('',#13337,#13338,#3596,.T.);
#16915=EDGE_CURVE('',#13339,#13340,#3597,.F.);
#16916=EDGE_CURVE('',#13340,#13338,#3598,.T.);
#16917=EDGE_CURVE('',#13336,#13339,#3599,.T.);
#16918=EDGE_CURVE('',#13329,#13337,#3600,.T.);
#16919=EDGE_CURVE('',#13338,#13328,#3601,.T.);
#16920=EDGE_CURVE('',#13341,#13342,#3602,.T.);
#16921=EDGE_CURVE('',#13343,#13341,#3603,.T.);
#16922=EDGE_CURVE('',#13342,#13343,#3604,.T.);
#16923=EDGE_CURVE('',#13265,#13343,#3605,.T.);
#16924=EDGE_CURVE('',#13341,#13266,#3606,.T.);
#16925=EDGE_CURVE('',#13344,#13345,#3607,.T.);
#16926=EDGE_CURVE('',#13346,#13344,#3608,.T.);
#16927=EDGE_CURVE('',#13345,#13346,#3609,.T.);
#16928=EDGE_CURVE('',#13347,#13348,#3610,.T.);
#16929=EDGE_CURVE('',#13349,#13347,#3611,.T.);
#16930=EDGE_CURVE('',#13348,#13349,#3612,.T.);
#16931=EDGE_CURVE('',#13347,#13342,#3613,.T.);
#16932=EDGE_CURVE('',#13343,#13349,#3614,.T.);
#16933=EDGE_CURVE('',#13263,#13348,#3615,.T.);
#16934=EDGE_CURVE('',#13349,#13264,#3616,.T.);
#16935=EDGE_CURVE('',#13344,#13347,#3617,.T.);
#16936=EDGE_CURVE('',#13348,#13346,#3618,.T.);
#16937=EDGE_CURVE('',#13337,#13345,#3619,.T.);
#16938=EDGE_CURVE('',#13346,#13336,#3620,.T.);
#16939=EDGE_CURVE('',#13345,#13334,#3621,.T.);
#16940=EDGE_CURVE('',#13335,#13344,#3622,.T.);
#16941=EDGE_CURVE('',#13333,#13341,#3623,.T.);
#16942=EDGE_CURVE('',#13342,#13335,#3624,.T.);
#16943=EDGE_CURVE('',#13334,#13329,#3625,.T.);
#16944=EDGE_CURVE('',#13330,#13333,#3626,.T.);
#16945=EDGE_CURVE('',#13244,#13332,#3627,.T.);
#16946=EDGE_CURVE('',#13331,#13340,#3628,.T.);
#16947=EDGE_CURVE('',#13303,#13350,#3629,.T.);
#16948=EDGE_CURVE('',#13350,#13350,#11224,.T.);
#16949=EDGE_CURVE('',#13350,#13351,#3630,.T.);
#16950=EDGE_CURVE('',#13351,#13352,#10869,.T.);
#16951=EDGE_CURVE('',#13352,#13351,#10870,.T.);
#16952=EDGE_CURVE('',#13352,#13351,#3631,.T.);
#16953=EDGE_CURVE('',#13352,#13351,#3632,.T.);
#16954=EDGE_CURVE('',#13339,#13275,#3633,.T.);
#16955=EDGE_CURVE('',#13288,#13274,#3634,.T.);
#16956=EDGE_CURVE('',#13353,#13353,#10871,.T.);
#16957=EDGE_CURVE('',#13353,#13352,#3635,.T.);
#16958=EDGE_CURVE('',#13351,#13272,#3636,.T.);
#16959=EDGE_CURVE('',#13354,#13355,#3637,.T.);
#16960=EDGE_CURVE('',#13354,#13356,#11225,.T.);
#16961=EDGE_CURVE('',#13356,#13357,#10872,.T.);
#16962=EDGE_CURVE('',#13357,#13355,#11226,.T.);
#16963=EDGE_CURVE('',#13358,#13359,#3638,.T.);
#16964=EDGE_CURVE('',#13358,#13354,#11227,.T.);
#16965=EDGE_CURVE('',#13355,#13359,#11228,.T.);
#16966=EDGE_CURVE('',#13360,#13361,#3639,.T.);
#16967=EDGE_CURVE('',#13360,#13358,#11229,.T.);
#16968=EDGE_CURVE('',#13359,#13361,#11230,.T.);
#16969=EDGE_CURVE('',#13362,#13363,#3640,.T.);
#16970=EDGE_CURVE('',#13362,#13360,#11231,.T.);
#16971=EDGE_CURVE('',#13361,#13363,#11232,.T.);
#16972=EDGE_CURVE('',#13364,#13365,#3641,.T.);
#16973=EDGE_CURVE('',#13364,#13362,#11233,.T.);
#16974=EDGE_CURVE('',#13363,#13365,#11234,.T.);
#16975=EDGE_CURVE('',#13366,#13367,#3642,.T.);
#16976=EDGE_CURVE('',#13366,#13364,#11235,.T.);
#16977=EDGE_CURVE('',#13365,#13367,#11236,.T.);
#16978=EDGE_CURVE('',#13368,#13369,#3643,.T.);
#16979=EDGE_CURVE('',#13368,#13366,#11237,.T.);
#16980=EDGE_CURVE('',#13367,#13369,#11238,.T.);
#16981=EDGE_CURVE('',#13370,#13371,#3644,.T.);
#16982=EDGE_CURVE('',#13370,#13368,#11239,.T.);
#16983=EDGE_CURVE('',#13369,#13371,#11240,.T.);
#16984=EDGE_CURVE('',#13372,#13373,#3645,.T.);
#16985=EDGE_CURVE('',#13372,#13370,#11241,.T.);
#16986=EDGE_CURVE('',#13371,#13373,#11242,.T.);
#16987=EDGE_CURVE('',#13374,#13375,#3646,.T.);
#16988=EDGE_CURVE('',#13374,#13372,#11243,.T.);
#16989=EDGE_CURVE('',#13373,#13375,#11244,.T.);
#16990=EDGE_CURVE('',#13376,#13377,#3647,.T.);
#16991=EDGE_CURVE('',#13376,#13374,#11245,.T.);
#16992=EDGE_CURVE('',#13375,#13377,#11246,.T.);
#16993=EDGE_CURVE('',#13378,#13379,#3648,.T.);
#16994=EDGE_CURVE('',#13378,#13376,#11247,.T.);
#16995=EDGE_CURVE('',#13377,#13379,#11248,.T.);
#16996=EDGE_CURVE('',#13380,#13381,#3649,.T.);
#16997=EDGE_CURVE('',#13380,#13378,#11249,.T.);
#16998=EDGE_CURVE('',#13379,#13381,#11250,.T.);
#16999=EDGE_CURVE('',#13382,#13383,#3650,.T.);
#17000=EDGE_CURVE('',#13382,#13380,#11251,.T.);
#17001=EDGE_CURVE('',#13381,#13383,#11252,.T.);
#17002=EDGE_CURVE('',#13384,#13385,#3651,.T.);
#17003=EDGE_CURVE('',#13384,#13382,#11253,.T.);
#17004=EDGE_CURVE('',#13383,#13385,#11254,.T.);
#17005=EDGE_CURVE('',#13386,#13387,#3652,.T.);
#17006=EDGE_CURVE('',#13386,#13384,#11255,.T.);
#17007=EDGE_CURVE('',#13385,#13387,#11256,.T.);
#17008=EDGE_CURVE('',#13388,#13389,#3653,.T.);
#17009=EDGE_CURVE('',#13388,#13386,#11257,.T.);
#17010=EDGE_CURVE('',#13387,#13389,#11258,.T.);
#17011=EDGE_CURVE('',#13390,#13391,#3654,.T.);
#17012=EDGE_CURVE('',#13390,#13388,#11259,.T.);
#17013=EDGE_CURVE('',#13389,#13391,#11260,.T.);
#17014=EDGE_CURVE('',#13392,#13393,#3655,.T.);
#17015=EDGE_CURVE('',#13392,#13390,#11261,.T.);
#17016=EDGE_CURVE('',#13391,#13393,#11262,.T.);
#17017=EDGE_CURVE('',#13394,#13395,#3656,.T.);
#17018=EDGE_CURVE('',#13394,#13392,#11263,.T.);
#17019=EDGE_CURVE('',#13393,#13395,#11264,.T.);
#17020=EDGE_CURVE('',#13396,#13397,#3657,.T.);
#17021=EDGE_CURVE('',#13396,#13398,#11265,.T.);
#17022=EDGE_CURVE('',#13397,#13398,#10873,.T.);
#17023=EDGE_CURVE('',#13399,#13400,#3658,.T.);
#17024=EDGE_CURVE('',#13399,#13396,#11266,.T.);
#17025=EDGE_CURVE('',#13401,#13397,#10874,.T.);
#17026=EDGE_CURVE('',#13400,#13401,#11267,.T.);
#17027=EDGE_CURVE('',#13402,#13403,#3659,.T.);
#17028=EDGE_CURVE('',#13402,#13399,#11268,.T.);
#17029=EDGE_CURVE('',#13403,#13400,#11269,.T.);
#17030=EDGE_CURVE('',#13404,#13405,#3660,.T.);
#17031=EDGE_CURVE('',#13404,#13402,#11270,.T.);
#17032=EDGE_CURVE('',#13405,#13403,#11271,.T.);
#17033=EDGE_CURVE('',#13406,#13407,#3661,.T.);
#17034=EDGE_CURVE('',#13406,#13404,#11272,.T.);
#17035=EDGE_CURVE('',#13407,#13405,#11273,.T.);
#17036=EDGE_CURVE('',#13408,#13409,#3662,.T.);
#17037=EDGE_CURVE('',#13408,#13406,#11274,.T.);
#17038=EDGE_CURVE('',#13409,#13407,#11275,.T.);
#17039=EDGE_CURVE('',#13410,#13411,#3663,.T.);
#17040=EDGE_CURVE('',#13410,#13408,#11276,.T.);
#17041=EDGE_CURVE('',#13411,#13409,#11277,.T.);
#17042=EDGE_CURVE('',#13412,#13413,#3664,.T.);
#17043=EDGE_CURVE('',#13412,#13410,#11278,.T.);
#17044=EDGE_CURVE('',#13413,#13411,#11279,.T.);
#17045=EDGE_CURVE('',#13414,#13415,#3665,.T.);
#17046=EDGE_CURVE('',#13414,#13412,#11280,.T.);
#17047=EDGE_CURVE('',#13415,#13413,#11281,.T.);
#17048=EDGE_CURVE('',#13416,#13417,#3666,.T.);
#17049=EDGE_CURVE('',#13416,#13414,#11282,.T.);
#17050=EDGE_CURVE('',#13417,#13415,#11283,.T.);
#17051=EDGE_CURVE('',#13418,#13419,#3667,.T.);
#17052=EDGE_CURVE('',#13418,#13416,#11284,.T.);
#17053=EDGE_CURVE('',#13419,#13417,#11285,.T.);
#17054=EDGE_CURVE('',#13420,#13421,#3668,.T.);
#17055=EDGE_CURVE('',#13420,#13418,#11286,.T.);
#17056=EDGE_CURVE('',#13421,#13419,#11287,.T.);
#17057=EDGE_CURVE('',#13422,#13423,#3669,.T.);
#17058=EDGE_CURVE('',#13422,#13420,#11288,.T.);
#17059=EDGE_CURVE('',#13423,#13421,#11289,.T.);
#17060=EDGE_CURVE('',#13424,#13425,#3670,.T.);
#17061=EDGE_CURVE('',#13424,#13422,#11290,.T.);
#17062=EDGE_CURVE('',#13425,#13423,#11291,.T.);
#17063=EDGE_CURVE('',#13426,#13427,#3671,.T.);
#17064=EDGE_CURVE('',#13426,#13424,#11292,.T.);
#17065=EDGE_CURVE('',#13427,#13425,#11293,.T.);
#17066=EDGE_CURVE('',#13428,#13429,#3672,.T.);
#17067=EDGE_CURVE('',#13428,#13426,#11294,.T.);
#17068=EDGE_CURVE('',#13429,#13427,#11295,.T.);
#17069=EDGE_CURVE('',#13430,#13431,#3673,.T.);
#17070=EDGE_CURVE('',#13430,#13428,#11296,.T.);
#17071=EDGE_CURVE('',#13431,#13429,#11297,.T.);
#17072=EDGE_CURVE('',#13432,#13433,#3674,.T.);
#17073=EDGE_CURVE('',#13432,#13430,#11298,.T.);
#17074=EDGE_CURVE('',#13433,#13431,#11299,.T.);
#17075=EDGE_CURVE('',#13434,#13435,#3675,.T.);
#17076=EDGE_CURVE('',#13434,#13432,#11300,.T.);
#17077=EDGE_CURVE('',#13435,#13433,#11301,.T.);
#17078=EDGE_CURVE('',#13436,#13437,#3676,.T.);
#17079=EDGE_CURVE('',#13436,#13434,#11302,.T.);
#17080=EDGE_CURVE('',#13437,#13435,#11303,.T.);
#17081=EDGE_CURVE('',#13438,#13401,#11304,.T.);
#17082=EDGE_CURVE('',#13395,#13438,#11305,.T.);
#17083=EDGE_CURVE('',#13439,#13357,#11306,.T.);
#17084=EDGE_CURVE('',#13439,#13437,#11307,.T.);
#17085=EDGE_CURVE('',#13357,#13440,#10875,.T.);
#17086=EDGE_CURVE('',#13440,#13356,#10876,.T.);
#17087=EDGE_CURVE('',#13356,#13441,#11308,.T.);
#17088=EDGE_CURVE('',#13441,#13439,#10877,.T.);
#17089=EDGE_CURVE('',#13441,#13436,#11309,.T.);
#17090=EDGE_CURVE('',#13398,#13442,#11310,.T.);
#17091=EDGE_CURVE('',#13442,#13394,#11311,.T.);
#17092=EDGE_CURVE('',#13443,#13444,#189,.T.);
#17093=EDGE_CURVE('',#13445,#13443,#190,.T.);
#17094=EDGE_CURVE('',#13446,#13445,#191,.T.);
#17095=EDGE_CURVE('',#13447,#13446,#192,.T.);
#17096=EDGE_CURVE('',#13448,#13447,#193,.T.);
#17097=EDGE_CURVE('',#13448,#13449,#3677,.T.);
#17098=EDGE_CURVE('',#13449,#13449,#10878,.T.);
#17099=EDGE_CURVE('',#13450,#13448,#194,.T.);
#17100=EDGE_CURVE('',#13444,#13450,#195,.T.);
#17101=EDGE_CURVE('',#13451,#13446,#3678,.T.);
#17102=EDGE_CURVE('',#13451,#13452,#3679,.T.);
#17103=EDGE_CURVE('',#13452,#13447,#3680,.T.);
#17104=EDGE_CURVE('',#13453,#13445,#3681,.T.);
#17105=EDGE_CURVE('',#13453,#13451,#3682,.T.);
#17106=EDGE_CURVE('',#13454,#13443,#3683,.T.);
#17107=EDGE_CURVE('',#13454,#13453,#3684,.T.);
#17108=EDGE_CURVE('',#13455,#13454,#3685,.T.);
#17109=EDGE_CURVE('',#13456,#13455,#3686,.T.);
#17110=EDGE_CURVE('',#13452,#13456,#3687,.T.);
#17111=EDGE_CURVE('',#13442,#13438,#10879,.F.);
#17112=EDGE_CURVE('',#13455,#13444,#3688,.T.);
#17113=EDGE_CURVE('',#13456,#13450,#3689,.T.);
#17114=EDGE_CURVE('',#13457,#13457,#10880,.T.);
#17115=EDGE_CURVE('',#13440,#13457,#3690,.T.);
#17116=EDGE_CURVE('',#13458,#13459,#3691,.T.);
#17117=EDGE_CURVE('',#13458,#13460,#11312,.T.);
#17118=EDGE_CURVE('',#13460,#13461,#10881,.T.);
#17119=EDGE_CURVE('',#13461,#13459,#11313,.T.);
#17120=EDGE_CURVE('',#13462,#13463,#3692,.T.);
#17121=EDGE_CURVE('',#13462,#13458,#11314,.T.);
#17122=EDGE_CURVE('',#13459,#13463,#11315,.T.);
#17123=EDGE_CURVE('',#13464,#13465,#3693,.T.);
#17124=EDGE_CURVE('',#13464,#13462,#11316,.T.);
#17125=EDGE_CURVE('',#13463,#13465,#11317,.T.);
#17126=EDGE_CURVE('',#13466,#13467,#3694,.T.);
#17127=EDGE_CURVE('',#13466,#13464,#11318,.T.);
#17128=EDGE_CURVE('',#13465,#13467,#11319,.T.);
#17129=EDGE_CURVE('',#13468,#13469,#3695,.T.);
#17130=EDGE_CURVE('',#13468,#13466,#11320,.T.);
#17131=EDGE_CURVE('',#13467,#13469,#11321,.T.);
#17132=EDGE_CURVE('',#13470,#13471,#3696,.T.);
#17133=EDGE_CURVE('',#13470,#13468,#11322,.T.);
#17134=EDGE_CURVE('',#13469,#13471,#11323,.T.);
#17135=EDGE_CURVE('',#13472,#13473,#3697,.T.);
#17136=EDGE_CURVE('',#13472,#13470,#11324,.T.);
#17137=EDGE_CURVE('',#13471,#13473,#11325,.T.);
#17138=EDGE_CURVE('',#13474,#13475,#3698,.T.);
#17139=EDGE_CURVE('',#13474,#13472,#11326,.T.);
#17140=EDGE_CURVE('',#13473,#13475,#11327,.T.);
#17141=EDGE_CURVE('',#13476,#13477,#3699,.T.);
#17142=EDGE_CURVE('',#13476,#13474,#11328,.T.);
#17143=EDGE_CURVE('',#13475,#13477,#11329,.T.);
#17144=EDGE_CURVE('',#13478,#13479,#3700,.T.);
#17145=EDGE_CURVE('',#13478,#13476,#11330,.T.);
#17146=EDGE_CURVE('',#13477,#13479,#11331,.T.);
#17147=EDGE_CURVE('',#13480,#13481,#3701,.T.);
#17148=EDGE_CURVE('',#13480,#13478,#11332,.T.);
#17149=EDGE_CURVE('',#13479,#13481,#11333,.T.);
#17150=EDGE_CURVE('',#13482,#13483,#3702,.T.);
#17151=EDGE_CURVE('',#13482,#13480,#11334,.T.);
#17152=EDGE_CURVE('',#13481,#13483,#11335,.T.);
#17153=EDGE_CURVE('',#13484,#13485,#3703,.T.);
#17154=EDGE_CURVE('',#13484,#13482,#11336,.T.);
#17155=EDGE_CURVE('',#13483,#13485,#11337,.T.);
#17156=EDGE_CURVE('',#13486,#13487,#3704,.T.);
#17157=EDGE_CURVE('',#13486,#13484,#11338,.T.);
#17158=EDGE_CURVE('',#13485,#13487,#11339,.T.);
#17159=EDGE_CURVE('',#13488,#13489,#3705,.T.);
#17160=EDGE_CURVE('',#13488,#13486,#11340,.T.);
#17161=EDGE_CURVE('',#13487,#13489,#11341,.T.);
#17162=EDGE_CURVE('',#13490,#13491,#3706,.T.);
#17163=EDGE_CURVE('',#13490,#13488,#11342,.T.);
#17164=EDGE_CURVE('',#13489,#13491,#11343,.T.);
#17165=EDGE_CURVE('',#13492,#13493,#3707,.T.);
#17166=EDGE_CURVE('',#13492,#13490,#11344,.T.);
#17167=EDGE_CURVE('',#13491,#13493,#11345,.T.);
#17168=EDGE_CURVE('',#13494,#13495,#3708,.T.);
#17169=EDGE_CURVE('',#13494,#13492,#11346,.T.);
#17170=EDGE_CURVE('',#13493,#13495,#11347,.T.);
#17171=EDGE_CURVE('',#13496,#13497,#3709,.T.);
#17172=EDGE_CURVE('',#13496,#13494,#11348,.T.);
#17173=EDGE_CURVE('',#13495,#13497,#11349,.T.);
#17174=EDGE_CURVE('',#13498,#13499,#3710,.T.);
#17175=EDGE_CURVE('',#13498,#13496,#11350,.T.);
#17176=EDGE_CURVE('',#13497,#13499,#11351,.T.);
#17177=EDGE_CURVE('',#13500,#13501,#3711,.T.);
#17178=EDGE_CURVE('',#13500,#13502,#11352,.T.);
#17179=EDGE_CURVE('',#13501,#13502,#10882,.T.);
#17180=EDGE_CURVE('',#13503,#13504,#3712,.T.);
#17181=EDGE_CURVE('',#13503,#13500,#11353,.T.);
#17182=EDGE_CURVE('',#13505,#13501,#10883,.T.);
#17183=EDGE_CURVE('',#13504,#13505,#11354,.T.);
#17184=EDGE_CURVE('',#13506,#13507,#3713,.T.);
#17185=EDGE_CURVE('',#13506,#13503,#11355,.T.);
#17186=EDGE_CURVE('',#13507,#13504,#11356,.T.);
#17187=EDGE_CURVE('',#13508,#13509,#3714,.T.);
#17188=EDGE_CURVE('',#13508,#13506,#11357,.T.);
#17189=EDGE_CURVE('',#13509,#13507,#11358,.T.);
#17190=EDGE_CURVE('',#13510,#13511,#3715,.T.);
#17191=EDGE_CURVE('',#13510,#13508,#11359,.T.);
#17192=EDGE_CURVE('',#13511,#13509,#11360,.T.);
#17193=EDGE_CURVE('',#13512,#13513,#3716,.T.);
#17194=EDGE_CURVE('',#13512,#13510,#11361,.T.);
#17195=EDGE_CURVE('',#13513,#13511,#11362,.T.);
#17196=EDGE_CURVE('',#13514,#13515,#3717,.T.);
#17197=EDGE_CURVE('',#13514,#13512,#11363,.T.);
#17198=EDGE_CURVE('',#13515,#13513,#11364,.T.);
#17199=EDGE_CURVE('',#13516,#13517,#3718,.T.);
#17200=EDGE_CURVE('',#13516,#13514,#11365,.T.);
#17201=EDGE_CURVE('',#13517,#13515,#11366,.T.);
#17202=EDGE_CURVE('',#13518,#13519,#3719,.T.);
#17203=EDGE_CURVE('',#13518,#13516,#11367,.T.);
#17204=EDGE_CURVE('',#13519,#13517,#11368,.T.);
#17205=EDGE_CURVE('',#13520,#13521,#3720,.T.);
#17206=EDGE_CURVE('',#13520,#13518,#11369,.T.);
#17207=EDGE_CURVE('',#13521,#13519,#11370,.T.);
#17208=EDGE_CURVE('',#13522,#13523,#3721,.T.);
#17209=EDGE_CURVE('',#13522,#13520,#11371,.T.);
#17210=EDGE_CURVE('',#13523,#13521,#11372,.T.);
#17211=EDGE_CURVE('',#13524,#13525,#3722,.T.);
#17212=EDGE_CURVE('',#13524,#13522,#11373,.T.);
#17213=EDGE_CURVE('',#13525,#13523,#11374,.T.);
#17214=EDGE_CURVE('',#13526,#13527,#3723,.T.);
#17215=EDGE_CURVE('',#13526,#13524,#11375,.T.);
#17216=EDGE_CURVE('',#13527,#13525,#11376,.T.);
#17217=EDGE_CURVE('',#13528,#13529,#3724,.T.);
#17218=EDGE_CURVE('',#13528,#13526,#11377,.T.);
#17219=EDGE_CURVE('',#13529,#13527,#11378,.T.);
#17220=EDGE_CURVE('',#13530,#13531,#3725,.T.);
#17221=EDGE_CURVE('',#13530,#13528,#11379,.T.);
#17222=EDGE_CURVE('',#13531,#13529,#11380,.T.);
#17223=EDGE_CURVE('',#13532,#13533,#3726,.T.);
#17224=EDGE_CURVE('',#13532,#13530,#11381,.T.);
#17225=EDGE_CURVE('',#13533,#13531,#11382,.T.);
#17226=EDGE_CURVE('',#13534,#13535,#3727,.T.);
#17227=EDGE_CURVE('',#13534,#13532,#11383,.T.);
#17228=EDGE_CURVE('',#13535,#13533,#11384,.T.);
#17229=EDGE_CURVE('',#13536,#13537,#3728,.T.);
#17230=EDGE_CURVE('',#13536,#13534,#11385,.T.);
#17231=EDGE_CURVE('',#13537,#13535,#11386,.T.);
#17232=EDGE_CURVE('',#13538,#13539,#3729,.T.);
#17233=EDGE_CURVE('',#13538,#13536,#11387,.T.);
#17234=EDGE_CURVE('',#13539,#13537,#11388,.T.);
#17235=EDGE_CURVE('',#13540,#13541,#3730,.T.);
#17236=EDGE_CURVE('',#13540,#13538,#11389,.T.);
#17237=EDGE_CURVE('',#13541,#13539,#11390,.T.);
#17238=EDGE_CURVE('',#13542,#13505,#11391,.T.);
#17239=EDGE_CURVE('',#13499,#13542,#11392,.T.);
#17240=EDGE_CURVE('',#13543,#13461,#11393,.T.);
#17241=EDGE_CURVE('',#13543,#13541,#11394,.T.);
#17242=EDGE_CURVE('',#13461,#13544,#10884,.T.);
#17243=EDGE_CURVE('',#13544,#13460,#10885,.T.);
#17244=EDGE_CURVE('',#13460,#13545,#11395,.T.);
#17245=EDGE_CURVE('',#13545,#13543,#10886,.T.);
#17246=EDGE_CURVE('',#13545,#13540,#11396,.T.);
#17247=EDGE_CURVE('',#13502,#13546,#11397,.T.);
#17248=EDGE_CURVE('',#13546,#13498,#11398,.T.);
#17249=EDGE_CURVE('',#13547,#13548,#3731,.T.);
#17250=EDGE_CURVE('',#13547,#13549,#3732,.T.);
#17251=EDGE_CURVE('',#13550,#13549,#3733,.T.);
#17252=EDGE_CURVE('',#13548,#13550,#3734,.T.);
#17253=EDGE_CURVE('',#13548,#13551,#10887,.T.);
#17254=EDGE_CURVE('',#13550,#13551,#3735,.T.);
#17255=EDGE_CURVE('',#13551,#13552,#3736,.T.);
#17256=EDGE_CURVE('',#13549,#13552,#3737,.T.);
#17257=EDGE_CURVE('',#13552,#13547,#10888,.T.);
#17258=EDGE_CURVE('',#13553,#13554,#3738,.T.);
#17259=EDGE_CURVE('',#13553,#13555,#3739,.T.);
#17260=EDGE_CURVE('',#13556,#13555,#3740,.T.);
#17261=EDGE_CURVE('',#13554,#13556,#3741,.T.);
#17262=EDGE_CURVE('',#13554,#13557,#10889,.T.);
#17263=EDGE_CURVE('',#13556,#13557,#3742,.T.);
#17264=EDGE_CURVE('',#13557,#13558,#3743,.T.);
#17265=EDGE_CURVE('',#13555,#13558,#3744,.T.);
#17266=EDGE_CURVE('',#13558,#13553,#10890,.T.);
#17267=EDGE_CURVE('',#13559,#13560,#3745,.T.);
#17268=EDGE_CURVE('',#13559,#13561,#3746,.T.);
#17269=EDGE_CURVE('',#13562,#13561,#3747,.T.);
#17270=EDGE_CURVE('',#13560,#13562,#3748,.T.);
#17271=EDGE_CURVE('',#13560,#13563,#10891,.T.);
#17272=EDGE_CURVE('',#13562,#13563,#3749,.T.);
#17273=EDGE_CURVE('',#13563,#13564,#3750,.T.);
#17274=EDGE_CURVE('',#13561,#13564,#3751,.T.);
#17275=EDGE_CURVE('',#13564,#13559,#10892,.T.);
#17276=EDGE_CURVE('',#13565,#13566,#3752,.T.);
#17277=EDGE_CURVE('',#13565,#13567,#3753,.T.);
#17278=EDGE_CURVE('',#13568,#13567,#3754,.T.);
#17279=EDGE_CURVE('',#13566,#13568,#3755,.T.);
#17280=EDGE_CURVE('',#13566,#13569,#10893,.T.);
#17281=EDGE_CURVE('',#13568,#13569,#3756,.T.);
#17282=EDGE_CURVE('',#13569,#13570,#3757,.T.);
#17283=EDGE_CURVE('',#13567,#13570,#3758,.T.);
#17284=EDGE_CURVE('',#13570,#13565,#10894,.T.);
#17285=EDGE_CURVE('',#13571,#13572,#3759,.T.);
#17286=EDGE_CURVE('',#13571,#13573,#3760,.T.);
#17287=EDGE_CURVE('',#13574,#13573,#3761,.T.);
#17288=EDGE_CURVE('',#13572,#13574,#3762,.T.);
#17289=EDGE_CURVE('',#13572,#13575,#10895,.T.);
#17290=EDGE_CURVE('',#13574,#13575,#3763,.T.);
#17291=EDGE_CURVE('',#13575,#13576,#3764,.T.);
#17292=EDGE_CURVE('',#13573,#13576,#3765,.T.);
#17293=EDGE_CURVE('',#13576,#13571,#10896,.T.);
#17294=EDGE_CURVE('',#13577,#13578,#3766,.T.);
#17295=EDGE_CURVE('',#13577,#13579,#3767,.T.);
#17296=EDGE_CURVE('',#13580,#13579,#3768,.T.);
#17297=EDGE_CURVE('',#13578,#13580,#3769,.T.);
#17298=EDGE_CURVE('',#13578,#13581,#10897,.T.);
#17299=EDGE_CURVE('',#13580,#13581,#3770,.T.);
#17300=EDGE_CURVE('',#13581,#13582,#3771,.T.);
#17301=EDGE_CURVE('',#13579,#13582,#3772,.T.);
#17302=EDGE_CURVE('',#13582,#13577,#10898,.T.);
#17303=EDGE_CURVE('',#13583,#13584,#3773,.T.);
#17304=EDGE_CURVE('',#13583,#13585,#3774,.T.);
#17305=EDGE_CURVE('',#13586,#13585,#3775,.T.);
#17306=EDGE_CURVE('',#13584,#13586,#3776,.T.);
#17307=EDGE_CURVE('',#13584,#13587,#10899,.T.);
#17308=EDGE_CURVE('',#13586,#13587,#3777,.T.);
#17309=EDGE_CURVE('',#13587,#13588,#3778,.T.);
#17310=EDGE_CURVE('',#13585,#13588,#3779,.T.);
#17311=EDGE_CURVE('',#13588,#13583,#10900,.T.);
#17312=EDGE_CURVE('',#13589,#13590,#3780,.T.);
#17313=EDGE_CURVE('',#13589,#13591,#3781,.T.);
#17314=EDGE_CURVE('',#13592,#13591,#3782,.T.);
#17315=EDGE_CURVE('',#13590,#13592,#3783,.T.);
#17316=EDGE_CURVE('',#13590,#13593,#10901,.T.);
#17317=EDGE_CURVE('',#13592,#13593,#3784,.T.);
#17318=EDGE_CURVE('',#13593,#13594,#3785,.T.);
#17319=EDGE_CURVE('',#13591,#13594,#3786,.T.);
#17320=EDGE_CURVE('',#13594,#13589,#10902,.T.);
#17321=EDGE_CURVE('',#13595,#13596,#3787,.T.);
#17322=EDGE_CURVE('',#13595,#13597,#3788,.T.);
#17323=EDGE_CURVE('',#13598,#13597,#3789,.T.);
#17324=EDGE_CURVE('',#13596,#13598,#3790,.T.);
#17325=EDGE_CURVE('',#13596,#13599,#10903,.T.);
#17326=EDGE_CURVE('',#13598,#13599,#3791,.T.);
#17327=EDGE_CURVE('',#13599,#13600,#3792,.T.);
#17328=EDGE_CURVE('',#13597,#13600,#3793,.T.);
#17329=EDGE_CURVE('',#13600,#13595,#10904,.T.);
#17330=EDGE_CURVE('',#13601,#13602,#3794,.T.);
#17331=EDGE_CURVE('',#13601,#13603,#3795,.T.);
#17332=EDGE_CURVE('',#13604,#13603,#3796,.T.);
#17333=EDGE_CURVE('',#13602,#13604,#3797,.T.);
#17334=EDGE_CURVE('',#13602,#13605,#10905,.T.);
#17335=EDGE_CURVE('',#13604,#13605,#3798,.T.);
#17336=EDGE_CURVE('',#13605,#13606,#3799,.T.);
#17337=EDGE_CURVE('',#13603,#13606,#3800,.T.);
#17338=EDGE_CURVE('',#13606,#13601,#10906,.T.);
#17339=EDGE_CURVE('',#13607,#13608,#3801,.T.);
#17340=EDGE_CURVE('',#13607,#13609,#3802,.T.);
#17341=EDGE_CURVE('',#13610,#13609,#3803,.T.);
#17342=EDGE_CURVE('',#13608,#13610,#3804,.T.);
#17343=EDGE_CURVE('',#13608,#13611,#10907,.T.);
#17344=EDGE_CURVE('',#13610,#13611,#3805,.T.);
#17345=EDGE_CURVE('',#13611,#13612,#3806,.T.);
#17346=EDGE_CURVE('',#13609,#13612,#3807,.T.);
#17347=EDGE_CURVE('',#13612,#13607,#10908,.T.);
#17348=EDGE_CURVE('',#13613,#13614,#3808,.T.);
#17349=EDGE_CURVE('',#13613,#13615,#3809,.T.);
#17350=EDGE_CURVE('',#13616,#13615,#3810,.T.);
#17351=EDGE_CURVE('',#13614,#13616,#3811,.T.);
#17352=EDGE_CURVE('',#13614,#13617,#10909,.T.);
#17353=EDGE_CURVE('',#13616,#13617,#3812,.T.);
#17354=EDGE_CURVE('',#13617,#13618,#3813,.T.);
#17355=EDGE_CURVE('',#13615,#13618,#3814,.T.);
#17356=EDGE_CURVE('',#13618,#13613,#10910,.T.);
#17357=EDGE_CURVE('',#13619,#13620,#3815,.T.);
#17358=EDGE_CURVE('',#13619,#13621,#3816,.T.);
#17359=EDGE_CURVE('',#13622,#13621,#3817,.T.);
#17360=EDGE_CURVE('',#13620,#13622,#3818,.T.);
#17361=EDGE_CURVE('',#13620,#13623,#10911,.T.);
#17362=EDGE_CURVE('',#13622,#13623,#3819,.T.);
#17363=EDGE_CURVE('',#13623,#13624,#3820,.T.);
#17364=EDGE_CURVE('',#13621,#13624,#3821,.T.);
#17365=EDGE_CURVE('',#13624,#13619,#10912,.T.);
#17366=EDGE_CURVE('',#13625,#13626,#3822,.T.);
#17367=EDGE_CURVE('',#13625,#13627,#3823,.T.);
#17368=EDGE_CURVE('',#13628,#13627,#3824,.T.);
#17369=EDGE_CURVE('',#13626,#13628,#3825,.T.);
#17370=EDGE_CURVE('',#13626,#13629,#10913,.T.);
#17371=EDGE_CURVE('',#13628,#13629,#3826,.T.);
#17372=EDGE_CURVE('',#13629,#13630,#3827,.T.);
#17373=EDGE_CURVE('',#13627,#13630,#3828,.T.);
#17374=EDGE_CURVE('',#13630,#13625,#10914,.T.);
#17375=EDGE_CURVE('',#13631,#13632,#3829,.T.);
#17376=EDGE_CURVE('',#13631,#13633,#3830,.T.);
#17377=EDGE_CURVE('',#13634,#13633,#3831,.T.);
#17378=EDGE_CURVE('',#13632,#13634,#3832,.T.);
#17379=EDGE_CURVE('',#13632,#13635,#10915,.T.);
#17380=EDGE_CURVE('',#13634,#13635,#3833,.T.);
#17381=EDGE_CURVE('',#13635,#13636,#3834,.T.);
#17382=EDGE_CURVE('',#13633,#13636,#3835,.T.);
#17383=EDGE_CURVE('',#13636,#13631,#10916,.T.);
#17384=EDGE_CURVE('',#13637,#13638,#3836,.T.);
#17385=EDGE_CURVE('',#13637,#13639,#3837,.T.);
#17386=EDGE_CURVE('',#13640,#13639,#3838,.T.);
#17387=EDGE_CURVE('',#13638,#13640,#3839,.T.);
#17388=EDGE_CURVE('',#13638,#13641,#10917,.T.);
#17389=EDGE_CURVE('',#13640,#13641,#3840,.T.);
#17390=EDGE_CURVE('',#13641,#13642,#3841,.T.);
#17391=EDGE_CURVE('',#13639,#13642,#3842,.T.);
#17392=EDGE_CURVE('',#13642,#13637,#10918,.T.);
#17393=EDGE_CURVE('',#13643,#13644,#3843,.T.);
#17394=EDGE_CURVE('',#13643,#13645,#3844,.T.);
#17395=EDGE_CURVE('',#13646,#13645,#3845,.T.);
#17396=EDGE_CURVE('',#13644,#13646,#3846,.T.);
#17397=EDGE_CURVE('',#13644,#13647,#10919,.T.);
#17398=EDGE_CURVE('',#13646,#13647,#3847,.T.);
#17399=EDGE_CURVE('',#13647,#13648,#3848,.T.);
#17400=EDGE_CURVE('',#13645,#13648,#3849,.T.);
#17401=EDGE_CURVE('',#13648,#13643,#10920,.T.);
#17402=EDGE_CURVE('',#13649,#13650,#3850,.T.);
#17403=EDGE_CURVE('',#13649,#13651,#3851,.T.);
#17404=EDGE_CURVE('',#13652,#13651,#3852,.T.);
#17405=EDGE_CURVE('',#13650,#13652,#3853,.T.);
#17406=EDGE_CURVE('',#13650,#13653,#10921,.T.);
#17407=EDGE_CURVE('',#13652,#13654,#3854,.T.);
#17408=EDGE_CURVE('',#13653,#13654,#10922,.T.);
#17409=EDGE_CURVE('',#13654,#13655,#3855,.T.);
#17410=EDGE_CURVE('',#13651,#13655,#3856,.T.);
#17411=EDGE_CURVE('',#13655,#13656,#10923,.T.);
#17412=EDGE_CURVE('',#13656,#13649,#10924,.T.);
#17413=EDGE_CURVE('',#13657,#13658,#3857,.T.);
#17414=EDGE_CURVE('',#13657,#13659,#3858,.T.);
#17415=EDGE_CURVE('',#13660,#13659,#3859,.T.);
#17416=EDGE_CURVE('',#13658,#13660,#3860,.T.);
#17417=EDGE_CURVE('',#13658,#13661,#10925,.T.);
#17418=EDGE_CURVE('',#13660,#13661,#3861,.T.);
#17419=EDGE_CURVE('',#13661,#13662,#3862,.T.);
#17420=EDGE_CURVE('',#13659,#13662,#3863,.T.);
#17421=EDGE_CURVE('',#13662,#13657,#10926,.T.);
#17422=EDGE_CURVE('',#13663,#13664,#3864,.T.);
#17423=EDGE_CURVE('',#13663,#13665,#3865,.T.);
#17424=EDGE_CURVE('',#13666,#13665,#3866,.T.);
#17425=EDGE_CURVE('',#13664,#13666,#3867,.T.);
#17426=EDGE_CURVE('',#13664,#13667,#10927,.T.);
#17427=EDGE_CURVE('',#13666,#13667,#3868,.T.);
#17428=EDGE_CURVE('',#13667,#13668,#3869,.T.);
#17429=EDGE_CURVE('',#13665,#13668,#3870,.T.);
#17430=EDGE_CURVE('',#13668,#13663,#10928,.T.);
#17431=EDGE_CURVE('',#13669,#13670,#3871,.T.);
#17432=EDGE_CURVE('',#13669,#13671,#3872,.T.);
#17433=EDGE_CURVE('',#13672,#13671,#3873,.T.);
#17434=EDGE_CURVE('',#13670,#13672,#3874,.T.);
#17435=EDGE_CURVE('',#13670,#13673,#10929,.T.);
#17436=EDGE_CURVE('',#13672,#13673,#3875,.T.);
#17437=EDGE_CURVE('',#13673,#13674,#3876,.T.);
#17438=EDGE_CURVE('',#13671,#13674,#3877,.T.);
#17439=EDGE_CURVE('',#13674,#13669,#10930,.T.);
#17440=EDGE_CURVE('',#13675,#13676,#3878,.T.);
#17441=EDGE_CURVE('',#13675,#13677,#3879,.T.);
#17442=EDGE_CURVE('',#13678,#13677,#3880,.T.);
#17443=EDGE_CURVE('',#13676,#13678,#3881,.T.);
#17444=EDGE_CURVE('',#13676,#13679,#10931,.T.);
#17445=EDGE_CURVE('',#13678,#13679,#3882,.T.);
#17446=EDGE_CURVE('',#13679,#13680,#3883,.T.);
#17447=EDGE_CURVE('',#13677,#13680,#3884,.T.);
#17448=EDGE_CURVE('',#13680,#13675,#10932,.T.);
#17449=EDGE_CURVE('',#13681,#13682,#3885,.T.);
#17450=EDGE_CURVE('',#13681,#13683,#3886,.T.);
#17451=EDGE_CURVE('',#13684,#13683,#3887,.T.);
#17452=EDGE_CURVE('',#13682,#13684,#3888,.T.);
#17453=EDGE_CURVE('',#13682,#13685,#10933,.T.);
#17454=EDGE_CURVE('',#13684,#13685,#3889,.T.);
#17455=EDGE_CURVE('',#13685,#13686,#3890,.T.);
#17456=EDGE_CURVE('',#13683,#13686,#3891,.T.);
#17457=EDGE_CURVE('',#13686,#13681,#10934,.T.);
#17458=EDGE_CURVE('',#13687,#13688,#3892,.T.);
#17459=EDGE_CURVE('',#13687,#13689,#3893,.T.);
#17460=EDGE_CURVE('',#13690,#13689,#3894,.T.);
#17461=EDGE_CURVE('',#13688,#13690,#3895,.T.);
#17462=EDGE_CURVE('',#13688,#13691,#10935,.T.);
#17463=EDGE_CURVE('',#13690,#13691,#3896,.T.);
#17464=EDGE_CURVE('',#13691,#13692,#3897,.T.);
#17465=EDGE_CURVE('',#13689,#13692,#3898,.T.);
#17466=EDGE_CURVE('',#13692,#13687,#10936,.T.);
#17467=EDGE_CURVE('',#13693,#13694,#3899,.T.);
#17468=EDGE_CURVE('',#13693,#13695,#3900,.T.);
#17469=EDGE_CURVE('',#13696,#13695,#3901,.T.);
#17470=EDGE_CURVE('',#13694,#13696,#3902,.T.);
#17471=EDGE_CURVE('',#13694,#13697,#10937,.T.);
#17472=EDGE_CURVE('',#13696,#13697,#3903,.T.);
#17473=EDGE_CURVE('',#13697,#13698,#3904,.T.);
#17474=EDGE_CURVE('',#13695,#13698,#3905,.T.);
#17475=EDGE_CURVE('',#13698,#13693,#10938,.T.);
#17476=EDGE_CURVE('',#13699,#13700,#3906,.T.);
#17477=EDGE_CURVE('',#13699,#13701,#3907,.T.);
#17478=EDGE_CURVE('',#13702,#13701,#3908,.T.);
#17479=EDGE_CURVE('',#13700,#13702,#3909,.T.);
#17480=EDGE_CURVE('',#13700,#13703,#10939,.T.);
#17481=EDGE_CURVE('',#13702,#13703,#3910,.T.);
#17482=EDGE_CURVE('',#13703,#13704,#3911,.T.);
#17483=EDGE_CURVE('',#13701,#13704,#3912,.T.);
#17484=EDGE_CURVE('',#13704,#13699,#10940,.T.);
#17485=EDGE_CURVE('',#13705,#13706,#3913,.T.);
#17486=EDGE_CURVE('',#13705,#13707,#3914,.T.);
#17487=EDGE_CURVE('',#13708,#13707,#3915,.T.);
#17488=EDGE_CURVE('',#13706,#13708,#3916,.T.);
#17489=EDGE_CURVE('',#13706,#13709,#10941,.T.);
#17490=EDGE_CURVE('',#13708,#13709,#3917,.T.);
#17491=EDGE_CURVE('',#13709,#13710,#3918,.T.);
#17492=EDGE_CURVE('',#13707,#13710,#3919,.T.);
#17493=EDGE_CURVE('',#13710,#13705,#10942,.T.);
#17494=EDGE_CURVE('',#13711,#13712,#3920,.T.);
#17495=EDGE_CURVE('',#13711,#13713,#3921,.T.);
#17496=EDGE_CURVE('',#13714,#13713,#3922,.T.);
#17497=EDGE_CURVE('',#13712,#13714,#3923,.T.);
#17498=EDGE_CURVE('',#13712,#13715,#10943,.T.);
#17499=EDGE_CURVE('',#13714,#13715,#3924,.T.);
#17500=EDGE_CURVE('',#13715,#13716,#3925,.T.);
#17501=EDGE_CURVE('',#13713,#13716,#3926,.T.);
#17502=EDGE_CURVE('',#13716,#13711,#10944,.T.);
#17503=EDGE_CURVE('',#13717,#13718,#3927,.T.);
#17504=EDGE_CURVE('',#13717,#13719,#3928,.T.);
#17505=EDGE_CURVE('',#13720,#13719,#3929,.T.);
#17506=EDGE_CURVE('',#13718,#13720,#3930,.T.);
#17507=EDGE_CURVE('',#13718,#13721,#10945,.T.);
#17508=EDGE_CURVE('',#13720,#13721,#3931,.T.);
#17509=EDGE_CURVE('',#13721,#13722,#3932,.T.);
#17510=EDGE_CURVE('',#13719,#13722,#3933,.T.);
#17511=EDGE_CURVE('',#13722,#13717,#10946,.T.);
#17512=EDGE_CURVE('',#13723,#13724,#3934,.T.);
#17513=EDGE_CURVE('',#13723,#13725,#3935,.T.);
#17514=EDGE_CURVE('',#13726,#13725,#3936,.T.);
#17515=EDGE_CURVE('',#13724,#13726,#3937,.T.);
#17516=EDGE_CURVE('',#13724,#13727,#10947,.T.);
#17517=EDGE_CURVE('',#13726,#13727,#3938,.T.);
#17518=EDGE_CURVE('',#13727,#13728,#3939,.T.);
#17519=EDGE_CURVE('',#13725,#13728,#3940,.T.);
#17520=EDGE_CURVE('',#13728,#13723,#10948,.T.);
#17521=EDGE_CURVE('',#13729,#13730,#3941,.T.);
#17522=EDGE_CURVE('',#13729,#13731,#3942,.T.);
#17523=EDGE_CURVE('',#13732,#13731,#3943,.T.);
#17524=EDGE_CURVE('',#13730,#13732,#3944,.T.);
#17525=EDGE_CURVE('',#13730,#13733,#10949,.T.);
#17526=EDGE_CURVE('',#13732,#13733,#3945,.T.);
#17527=EDGE_CURVE('',#13733,#13734,#3946,.T.);
#17528=EDGE_CURVE('',#13731,#13734,#3947,.T.);
#17529=EDGE_CURVE('',#13734,#13729,#10950,.T.);
#17530=EDGE_CURVE('',#13735,#13736,#3948,.T.);
#17531=EDGE_CURVE('',#13735,#13737,#3949,.T.);
#17532=EDGE_CURVE('',#13738,#13737,#3950,.T.);
#17533=EDGE_CURVE('',#13736,#13738,#3951,.T.);
#17534=EDGE_CURVE('',#13736,#13739,#10951,.T.);
#17535=EDGE_CURVE('',#13738,#13739,#3952,.T.);
#17536=EDGE_CURVE('',#13739,#13740,#3953,.T.);
#17537=EDGE_CURVE('',#13737,#13740,#3954,.T.);
#17538=EDGE_CURVE('',#13740,#13735,#10952,.T.);
#17539=EDGE_CURVE('',#13741,#13742,#3955,.T.);
#17540=EDGE_CURVE('',#13741,#13743,#3956,.T.);
#17541=EDGE_CURVE('',#13744,#13743,#3957,.T.);
#17542=EDGE_CURVE('',#13742,#13744,#3958,.T.);
#17543=EDGE_CURVE('',#13742,#13745,#10953,.T.);
#17544=EDGE_CURVE('',#13744,#13745,#3959,.T.);
#17545=EDGE_CURVE('',#13745,#13746,#3960,.T.);
#17546=EDGE_CURVE('',#13743,#13746,#3961,.T.);
#17547=EDGE_CURVE('',#13746,#13741,#10954,.T.);
#17548=EDGE_CURVE('',#13747,#13748,#3962,.T.);
#17549=EDGE_CURVE('',#13747,#13749,#3963,.T.);
#17550=EDGE_CURVE('',#13750,#13749,#3964,.T.);
#17551=EDGE_CURVE('',#13748,#13750,#3965,.T.);
#17552=EDGE_CURVE('',#13748,#13751,#10955,.T.);
#17553=EDGE_CURVE('',#13750,#13751,#3966,.T.);
#17554=EDGE_CURVE('',#13751,#13752,#3967,.T.);
#17555=EDGE_CURVE('',#13749,#13752,#3968,.T.);
#17556=EDGE_CURVE('',#13752,#13747,#10956,.T.);
#17557=EDGE_CURVE('',#13753,#13754,#3969,.T.);
#17558=EDGE_CURVE('',#13753,#13755,#3970,.T.);
#17559=EDGE_CURVE('',#13756,#13755,#3971,.T.);
#17560=EDGE_CURVE('',#13754,#13756,#3972,.T.);
#17561=EDGE_CURVE('',#13754,#13757,#10957,.T.);
#17562=EDGE_CURVE('',#13756,#13757,#3973,.T.);
#17563=EDGE_CURVE('',#13757,#13758,#3974,.T.);
#17564=EDGE_CURVE('',#13755,#13758,#3975,.T.);
#17565=EDGE_CURVE('',#13758,#13753,#10958,.T.);
#17566=EDGE_CURVE('',#13759,#13760,#3976,.T.);
#17567=EDGE_CURVE('',#13759,#13761,#3977,.T.);
#17568=EDGE_CURVE('',#13762,#13761,#3978,.T.);
#17569=EDGE_CURVE('',#13760,#13762,#3979,.T.);
#17570=EDGE_CURVE('',#13760,#13763,#10959,.T.);
#17571=EDGE_CURVE('',#13762,#13763,#3980,.T.);
#17572=EDGE_CURVE('',#13763,#13764,#3981,.T.);
#17573=EDGE_CURVE('',#13761,#13764,#3982,.T.);
#17574=EDGE_CURVE('',#13764,#13759,#10960,.T.);
#17575=EDGE_CURVE('',#13765,#13766,#3983,.T.);
#17576=EDGE_CURVE('',#13765,#13767,#3984,.T.);
#17577=EDGE_CURVE('',#13767,#13768,#3985,.T.);
#17578=EDGE_CURVE('',#13766,#13768,#3986,.T.);
#17579=EDGE_CURVE('',#13769,#13765,#3987,.T.);
#17580=EDGE_CURVE('',#13769,#13770,#3988,.T.);
#17581=EDGE_CURVE('',#13770,#13767,#3989,.T.);
#17582=EDGE_CURVE('',#13771,#13769,#3990,.T.);
#17583=EDGE_CURVE('',#13771,#13772,#3991,.T.);
#17584=EDGE_CURVE('',#13772,#13770,#3992,.T.);
#17585=EDGE_CURVE('',#13773,#13771,#3993,.T.);
#17586=EDGE_CURVE('',#13773,#13774,#3994,.T.);
#17587=EDGE_CURVE('',#13774,#13772,#3995,.T.);
#17588=EDGE_CURVE('',#13775,#13773,#3996,.T.);
#17589=EDGE_CURVE('',#13775,#13776,#3997,.T.);
#17590=EDGE_CURVE('',#13776,#13774,#3998,.T.);
#17591=EDGE_CURVE('',#13766,#13775,#3999,.T.);
#17592=EDGE_CURVE('',#13768,#13776,#4000,.T.);
#17593=EDGE_CURVE('',#13777,#13777,#10961,.T.);
#17594=EDGE_CURVE('',#13544,#13777,#4001,.T.);
#17595=EDGE_CURVE('',#13546,#13542,#10962,.T.);
#17596=EDGE_CURVE('',#13778,#13778,#10963,.T.);
#17597=EDGE_CURVE('',#13779,#13779,#10964,.T.);
#17598=EDGE_CURVE('',#13779,#13656,#4002,.T.);
#17599=EDGE_CURVE('',#13653,#13778,#4003,.T.);
#17600=EDGE_CURVE('',#13780,#13780,#10965,.T.);
#17601=EDGE_CURVE('',#13780,#13779,#4004,.T.);
#17602=EDGE_CURVE('',#13781,#13782,#4005,.T.);
#17603=EDGE_CURVE('',#13783,#13781,#4006,.T.);
#17604=EDGE_CURVE('',#13782,#13783,#4007,.T.);
#17605=EDGE_CURVE('',#13784,#13785,#4008,.T.);
#17606=EDGE_CURVE('',#13785,#13783,#4009,.T.);
#17607=EDGE_CURVE('',#13781,#13784,#4010,.T.);
#17608=EDGE_CURVE('',#13786,#13787,#4011,.T.);
#17609=EDGE_CURVE('',#13788,#13786,#4012,.T.);
#17610=EDGE_CURVE('',#13787,#13788,#4013,.T.);
#17611=EDGE_CURVE('',#13789,#13790,#4014,.T.);
#17612=EDGE_CURVE('',#13790,#13788,#4015,.T.);
#17613=EDGE_CURVE('',#13786,#13789,#4016,.T.);
#17614=EDGE_CURVE('',#13782,#13787,#4017,.T.);
#17615=EDGE_CURVE('',#13788,#13781,#4018,.T.);
#17616=EDGE_CURVE('',#13791,#13792,#4019,.T.);
#17617=EDGE_CURVE('',#13793,#13791,#4020,.T.);
#17618=EDGE_CURVE('',#13792,#13793,#4021,.T.);
#17619=EDGE_CURVE('',#13794,#13795,#4022,.T.);
#17620=EDGE_CURVE('',#13795,#13793,#4023,.T.);
#17621=EDGE_CURVE('',#13791,#13794,#4024,.T.);
#17622=EDGE_CURVE('',#13796,#13797,#4025,.T.);
#17623=EDGE_CURVE('',#13798,#13796,#4026,.T.);
#17624=EDGE_CURVE('',#13797,#13798,#4027,.T.);
#17625=EDGE_CURVE('',#13799,#13800,#4028,.T.);
#17626=EDGE_CURVE('',#13800,#13798,#4029,.T.);
#17627=EDGE_CURVE('',#13796,#13799,#4030,.T.);
#17628=EDGE_CURVE('',#13787,#13797,#4031,.T.);
#17629=EDGE_CURVE('',#13798,#13786,#4032,.T.);
#17630=EDGE_CURVE('',#13801,#13802,#4033,.T.);
#17631=EDGE_CURVE('',#13803,#13801,#4034,.T.);
#17632=EDGE_CURVE('',#13802,#13803,#4035,.T.);
#17633=EDGE_CURVE('',#13804,#13805,#4036,.T.);
#17634=EDGE_CURVE('',#13805,#13803,#4037,.T.);
#17635=EDGE_CURVE('',#13801,#13804,#4038,.T.);
#17636=EDGE_CURVE('',#13806,#13807,#4039,.T.);
#17637=EDGE_CURVE('',#13808,#13806,#4040,.T.);
#17638=EDGE_CURVE('',#13807,#13808,#4041,.T.);
#17639=EDGE_CURVE('',#13809,#13810,#4042,.T.);
#17640=EDGE_CURVE('',#13810,#13808,#4043,.T.);
#17641=EDGE_CURVE('',#13806,#13809,#4044,.T.);
#17642=EDGE_CURVE('',#13797,#13807,#4045,.T.);
#17643=EDGE_CURVE('',#13808,#13796,#4046,.T.);
#17644=EDGE_CURVE('',#13807,#13802,#4047,.T.);
#17645=EDGE_CURVE('',#13803,#13806,#4048,.T.);
#17646=EDGE_CURVE('',#13802,#13792,#4049,.T.);
#17647=EDGE_CURVE('',#13793,#13801,#4050,.T.);
#17648=EDGE_CURVE('',#13792,#13782,#4051,.T.);
#17649=EDGE_CURVE('',#13783,#13791,#4052,.T.);
#17650=EDGE_CURVE('',#13790,#13784,#4053,.T.);
#17651=EDGE_CURVE('',#13800,#13789,#4054,.T.);
#17652=EDGE_CURVE('',#13810,#13799,#4055,.T.);
#17653=EDGE_CURVE('',#13811,#13812,#4056,.T.);
#17654=EDGE_CURVE('',#13813,#13811,#4057,.T.);
#17655=EDGE_CURVE('',#13814,#13813,#4058,.T.);
#17656=EDGE_CURVE('',#13815,#13814,#4059,.T.);
#17657=EDGE_CURVE('',#13816,#13815,#4060,.T.);
#17658=EDGE_CURVE('',#13812,#13816,#4061,.T.);
#17659=EDGE_CURVE('',#13814,#13817,#4062,.T.);
#17660=EDGE_CURVE('',#13817,#13818,#4063,.T.);
#17661=EDGE_CURVE('',#13815,#13818,#4064,.T.);
#17662=EDGE_CURVE('',#13813,#13819,#4065,.T.);
#17663=EDGE_CURVE('',#13819,#13817,#4066,.T.);
#17664=EDGE_CURVE('',#13812,#13820,#4067,.T.);
#17665=EDGE_CURVE('',#13820,#13821,#4068,.T.);
#17666=EDGE_CURVE('',#13821,#13811,#4069,.T.);
#17667=EDGE_CURVE('',#13822,#13820,#4070,.T.);
#17668=EDGE_CURVE('',#13816,#13822,#4071,.T.);
#17669=EDGE_CURVE('',#13821,#13819,#4072,.T.);
#17670=EDGE_CURVE('',#13818,#13822,#4073,.T.);
#17671=EDGE_CURVE('',#13819,#13823,#4074,.T.);
#17672=EDGE_CURVE('',#13823,#13824,#4075,.T.);
#17673=EDGE_CURVE('',#13817,#13824,#4076,.T.);
#17674=EDGE_CURVE('',#13821,#13825,#4077,.T.);
#17675=EDGE_CURVE('',#13825,#13823,#4078,.T.);
#17676=EDGE_CURVE('',#13820,#13826,#4079,.T.);
#17677=EDGE_CURVE('',#13826,#13825,#4080,.T.);
#17678=EDGE_CURVE('',#13822,#13827,#4081,.T.);
#17679=EDGE_CURVE('',#13827,#13826,#4082,.T.);
#17680=EDGE_CURVE('',#13818,#13828,#4083,.T.);
#17681=EDGE_CURVE('',#13828,#13827,#4084,.T.);
#17682=EDGE_CURVE('',#13824,#13828,#4085,.T.);
#17683=EDGE_CURVE('',#13805,#13809,#4086,.T.);
#17684=EDGE_CURVE('',#13795,#13804,#4087,.T.);
#17685=EDGE_CURVE('',#13785,#13794,#4088,.T.);
#17686=EDGE_CURVE('',#13829,#13829,#10966,.T.);
#17687=EDGE_CURVE('',#13830,#13830,#10967,.T.);
#17688=EDGE_CURVE('',#13831,#13831,#10968,.T.);
#17689=EDGE_CURVE('',#13831,#13830,#4089,.T.);
#17690=EDGE_CURVE('',#13829,#13831,#4090,.T.);
#17691=EDGE_CURVE('',#13832,#13833,#4091,.T.);
#17692=EDGE_CURVE('',#13832,#13834,#11399,.T.);
#17693=EDGE_CURVE('',#13834,#13835,#10969,.T.);
#17694=EDGE_CURVE('',#13835,#13833,#11400,.T.);
#17695=EDGE_CURVE('',#13836,#13837,#4092,.T.);
#17696=EDGE_CURVE('',#13836,#13832,#11401,.T.);
#17697=EDGE_CURVE('',#13833,#13837,#11402,.T.);
#17698=EDGE_CURVE('',#13838,#13839,#4093,.T.);
#17699=EDGE_CURVE('',#13838,#13836,#11403,.T.);
#17700=EDGE_CURVE('',#13837,#13839,#11404,.T.);
#17701=EDGE_CURVE('',#13840,#13841,#4094,.T.);
#17702=EDGE_CURVE('',#13840,#13838,#11405,.T.);
#17703=EDGE_CURVE('',#13839,#13841,#11406,.T.);
#17704=EDGE_CURVE('',#13842,#13843,#4095,.T.);
#17705=EDGE_CURVE('',#13842,#13840,#11407,.T.);
#17706=EDGE_CURVE('',#13841,#13843,#11408,.T.);
#17707=EDGE_CURVE('',#13844,#13845,#4096,.T.);
#17708=EDGE_CURVE('',#13844,#13842,#11409,.T.);
#17709=EDGE_CURVE('',#13843,#13845,#11410,.T.);
#17710=EDGE_CURVE('',#13846,#13847,#4097,.T.);
#17711=EDGE_CURVE('',#13846,#13844,#11411,.T.);
#17712=EDGE_CURVE('',#13845,#13847,#11412,.T.);
#17713=EDGE_CURVE('',#13848,#13849,#4098,.T.);
#17714=EDGE_CURVE('',#13848,#13846,#11413,.T.);
#17715=EDGE_CURVE('',#13847,#13849,#11414,.T.);
#17716=EDGE_CURVE('',#13850,#13851,#4099,.T.);
#17717=EDGE_CURVE('',#13850,#13848,#11415,.T.);
#17718=EDGE_CURVE('',#13849,#13851,#11416,.T.);
#17719=EDGE_CURVE('',#13852,#13853,#4100,.T.);
#17720=EDGE_CURVE('',#13852,#13850,#11417,.T.);
#17721=EDGE_CURVE('',#13851,#13853,#11418,.T.);
#17722=EDGE_CURVE('',#13854,#13855,#4101,.T.);
#17723=EDGE_CURVE('',#13854,#13852,#11419,.T.);
#17724=EDGE_CURVE('',#13853,#13855,#11420,.T.);
#17725=EDGE_CURVE('',#13856,#13857,#4102,.T.);
#17726=EDGE_CURVE('',#13856,#13854,#11421,.T.);
#17727=EDGE_CURVE('',#13855,#13857,#11422,.T.);
#17728=EDGE_CURVE('',#13858,#13859,#4103,.T.);
#17729=EDGE_CURVE('',#13860,#13858,#10970,.T.);
#17730=EDGE_CURVE('',#13860,#13856,#11423,.T.);
#17731=EDGE_CURVE('',#13857,#13859,#11424,.T.);
#17732=EDGE_CURVE('',#13861,#13862,#4104,.T.);
#17733=EDGE_CURVE('',#13861,#13863,#11425,.T.);
#17734=EDGE_CURVE('',#13864,#13863,#10971,.T.);
#17735=EDGE_CURVE('',#13862,#13864,#11426,.T.);
#17736=EDGE_CURVE('',#13865,#13866,#4105,.T.);
#17737=EDGE_CURVE('',#13865,#13861,#11427,.T.);
#17738=EDGE_CURVE('',#13866,#13862,#11428,.T.);
#17739=EDGE_CURVE('',#13867,#13868,#4106,.T.);
#17740=EDGE_CURVE('',#13867,#13865,#11429,.T.);
#17741=EDGE_CURVE('',#13868,#13866,#11430,.T.);
#17742=EDGE_CURVE('',#13869,#13870,#4107,.T.);
#17743=EDGE_CURVE('',#13869,#13867,#11431,.T.);
#17744=EDGE_CURVE('',#13870,#13868,#11432,.T.);
#17745=EDGE_CURVE('',#13871,#13872,#4108,.T.);
#17746=EDGE_CURVE('',#13871,#13869,#11433,.T.);
#17747=EDGE_CURVE('',#13872,#13870,#11434,.T.);
#17748=EDGE_CURVE('',#13873,#13874,#4109,.T.);
#17749=EDGE_CURVE('',#13873,#13871,#11435,.T.);
#17750=EDGE_CURVE('',#13874,#13872,#11436,.T.);
#17751=EDGE_CURVE('',#13875,#13876,#4110,.T.);
#17752=EDGE_CURVE('',#13875,#13873,#11437,.T.);
#17753=EDGE_CURVE('',#13876,#13874,#11438,.T.);
#17754=EDGE_CURVE('',#13877,#13878,#4111,.T.);
#17755=EDGE_CURVE('',#13877,#13875,#11439,.T.);
#17756=EDGE_CURVE('',#13878,#13876,#11440,.T.);
#17757=EDGE_CURVE('',#13879,#13880,#4112,.T.);
#17758=EDGE_CURVE('',#13879,#13877,#11441,.T.);
#17759=EDGE_CURVE('',#13880,#13878,#11442,.T.);
#17760=EDGE_CURVE('',#13881,#13882,#4113,.T.);
#17761=EDGE_CURVE('',#13881,#13879,#11443,.T.);
#17762=EDGE_CURVE('',#13882,#13880,#11444,.T.);
#17763=EDGE_CURVE('',#13883,#13884,#4114,.T.);
#17764=EDGE_CURVE('',#13883,#13881,#11445,.T.);
#17765=EDGE_CURVE('',#13884,#13882,#11446,.T.);
#17766=EDGE_CURVE('',#13885,#13886,#4115,.T.);
#17767=EDGE_CURVE('',#13885,#13883,#11447,.T.);
#17768=EDGE_CURVE('',#13886,#13884,#11448,.T.);
#17769=EDGE_CURVE('',#13887,#13864,#11449,.T.);
#17770=EDGE_CURVE('',#13859,#13887,#11450,.T.);
#17771=EDGE_CURVE('',#13888,#13835,#11451,.T.);
#17772=EDGE_CURVE('',#13888,#13886,#11452,.T.);
#17773=EDGE_CURVE('',#13835,#13889,#10972,.T.);
#17774=EDGE_CURVE('',#13889,#13834,#10973,.T.);
#17775=EDGE_CURVE('',#13834,#13890,#11453,.T.);
#17776=EDGE_CURVE('',#13890,#13888,#10974,.T.);
#17777=EDGE_CURVE('',#13890,#13885,#11454,.T.);
#17778=EDGE_CURVE('',#13863,#13860,#11455,.T.);
#17779=EDGE_CURVE('',#13891,#13892,#11456,.T.);
#17780=EDGE_CURVE('',#13891,#13893,#4116,.T.);
#17781=EDGE_CURVE('',#13893,#13894,#4117,.T.);
#17782=EDGE_CURVE('',#13892,#13894,#4118,.T.);
#17783=EDGE_CURVE('',#13892,#13895,#11457,.T.);
#17784=EDGE_CURVE('',#13894,#13896,#4119,.T.);
#17785=EDGE_CURVE('',#13895,#13896,#4120,.T.);
#17786=EDGE_CURVE('',#13895,#13897,#11458,.T.);
#17787=EDGE_CURVE('',#13896,#13898,#4121,.T.);
#17788=EDGE_CURVE('',#13897,#13898,#4122,.T.);
#17789=EDGE_CURVE('',#13897,#13899,#11459,.T.);
#17790=EDGE_CURVE('',#13898,#13900,#4123,.T.);
#17791=EDGE_CURVE('',#13899,#13900,#4124,.T.);
#17792=EDGE_CURVE('',#13901,#13891,#11460,.T.);
#17793=EDGE_CURVE('',#13901,#13902,#4125,.T.);
#17794=EDGE_CURVE('',#13902,#13893,#4126,.T.);
#17795=EDGE_CURVE('',#13899,#13901,#11461,.T.);
#17796=EDGE_CURVE('',#13900,#13902,#4127,.T.);
#17797=EDGE_CURVE('',#13903,#13903,#10975,.T.);
#17798=EDGE_CURVE('',#13889,#13903,#4128,.T.);
#17799=EDGE_CURVE('',#13858,#13887,#10976,.T.);
#17800=EDGE_CURVE('',#13904,#13904,#10977,.T.);
#17801=EDGE_CURVE('',#13897,#13904,#196,.T.);
#17802=ORIENTED_EDGE('',*,*,#13905,.T.);
#17803=ORIENTED_EDGE('',*,*,#13906,.T.);
#17804=ORIENTED_EDGE('',*,*,#13907,.T.);
#17805=ORIENTED_EDGE('',*,*,#13908,.T.);
#17806=ORIENTED_EDGE('',*,*,#13907,.F.);
#17807=ORIENTED_EDGE('',*,*,#13909,.T.);
#17808=ORIENTED_EDGE('',*,*,#13910,.T.);
#17809=ORIENTED_EDGE('',*,*,#13911,.F.);
#17810=ORIENTED_EDGE('',*,*,#13906,.F.);
#17811=ORIENTED_EDGE('',*,*,#13912,.T.);
#17812=ORIENTED_EDGE('',*,*,#13913,.F.);
#17813=ORIENTED_EDGE('',*,*,#13914,.F.);
#17814=ORIENTED_EDGE('',*,*,#13915,.T.);
#17815=ORIENTED_EDGE('',*,*,#13916,.T.);
#17816=ORIENTED_EDGE('',*,*,#13917,.T.);
#17817=ORIENTED_EDGE('',*,*,#13918,.T.);
#17818=ORIENTED_EDGE('',*,*,#13919,.T.);
#17819=ORIENTED_EDGE('',*,*,#13920,.T.);
#17820=ORIENTED_EDGE('',*,*,#13921,.T.);
#17821=ORIENTED_EDGE('',*,*,#13922,.F.);
#17822=ORIENTED_EDGE('',*,*,#13923,.F.);
#17823=ORIENTED_EDGE('',*,*,#13924,.T.);
#17824=ORIENTED_EDGE('',*,*,#13925,.F.);
#17825=ORIENTED_EDGE('',*,*,#13909,.F.);
#17826=ORIENTED_EDGE('',*,*,#13908,.F.);
#17827=ORIENTED_EDGE('',*,*,#13926,.T.);
#17828=ORIENTED_EDGE('',*,*,#13927,.T.);
#17829=ORIENTED_EDGE('',*,*,#13928,.T.);
#17830=ORIENTED_EDGE('',*,*,#13929,.T.);
#17831=ORIENTED_EDGE('',*,*,#13930,.T.);
#17832=ORIENTED_EDGE('',*,*,#13914,.T.);
#17833=ORIENTED_EDGE('',*,*,#13931,.T.);
#17834=ORIENTED_EDGE('',*,*,#13932,.T.);
#17835=ORIENTED_EDGE('',*,*,#13931,.F.);
#17836=ORIENTED_EDGE('',*,*,#13913,.T.);
#17837=ORIENTED_EDGE('',*,*,#13933,.T.);
#17838=ORIENTED_EDGE('',*,*,#13922,.T.);
#17839=ORIENTED_EDGE('',*,*,#13934,.T.);
#17840=ORIENTED_EDGE('',*,*,#13932,.F.);
#17841=ORIENTED_EDGE('',*,*,#13935,.T.);
#17842=ORIENTED_EDGE('',*,*,#13936,.T.);
#17843=ORIENTED_EDGE('',*,*,#13937,.T.);
#17844=ORIENTED_EDGE('',*,*,#13938,.T.);
#17845=ORIENTED_EDGE('',*,*,#13939,.T.);
#17846=ORIENTED_EDGE('',*,*,#13940,.T.);
#17847=ORIENTED_EDGE('',*,*,#13941,.T.);
#17848=ORIENTED_EDGE('',*,*,#13942,.T.);
#17849=ORIENTED_EDGE('',*,*,#13943,.F.);
#17850=ORIENTED_EDGE('',*,*,#13944,.T.);
#17851=ORIENTED_EDGE('',*,*,#13945,.T.);
#17852=ORIENTED_EDGE('',*,*,#13946,.T.);
#17853=ORIENTED_EDGE('',*,*,#13947,.T.);
#17854=ORIENTED_EDGE('',*,*,#13948,.T.);
#17855=ORIENTED_EDGE('',*,*,#13949,.T.);
#17856=ORIENTED_EDGE('',*,*,#13946,.F.);
#17857=ORIENTED_EDGE('',*,*,#13950,.T.);
#17858=ORIENTED_EDGE('',*,*,#13951,.T.);
#17859=ORIENTED_EDGE('',*,*,#13952,.T.);
#17860=ORIENTED_EDGE('',*,*,#13948,.F.);
#17861=ORIENTED_EDGE('',*,*,#13953,.T.);
#17862=ORIENTED_EDGE('',*,*,#13954,.T.);
#17863=ORIENTED_EDGE('',*,*,#13955,.T.);
#17864=ORIENTED_EDGE('',*,*,#13951,.F.);
#17865=ORIENTED_EDGE('',*,*,#13956,.T.);
#17866=ORIENTED_EDGE('',*,*,#13957,.T.);
#17867=ORIENTED_EDGE('',*,*,#13958,.T.);
#17868=ORIENTED_EDGE('',*,*,#13954,.F.);
#17869=ORIENTED_EDGE('',*,*,#13959,.T.);
#17870=ORIENTED_EDGE('',*,*,#13960,.T.);
#17871=ORIENTED_EDGE('',*,*,#13961,.T.);
#17872=ORIENTED_EDGE('',*,*,#13957,.F.);
#17873=ORIENTED_EDGE('',*,*,#13962,.T.);
#17874=ORIENTED_EDGE('',*,*,#13963,.T.);
#17875=ORIENTED_EDGE('',*,*,#13964,.T.);
#17876=ORIENTED_EDGE('',*,*,#13960,.F.);
#17877=ORIENTED_EDGE('',*,*,#13965,.T.);
#17878=ORIENTED_EDGE('',*,*,#13944,.F.);
#17879=ORIENTED_EDGE('',*,*,#13966,.T.);
#17880=ORIENTED_EDGE('',*,*,#13963,.F.);
#17881=ORIENTED_EDGE('',*,*,#13967,.T.);
#17882=ORIENTED_EDGE('',*,*,#13961,.F.);
#17883=ORIENTED_EDGE('',*,*,#13968,.T.);
#17884=ORIENTED_EDGE('',*,*,#13969,.F.);
#17885=ORIENTED_EDGE('',*,*,#13970,.F.);
#17886=ORIENTED_EDGE('',*,*,#13964,.F.);
#17887=ORIENTED_EDGE('',*,*,#13971,.T.);
#17888=ORIENTED_EDGE('',*,*,#13972,.F.);
#17889=ORIENTED_EDGE('',*,*,#13968,.F.);
#17890=ORIENTED_EDGE('',*,*,#13966,.F.);
#17891=ORIENTED_EDGE('',*,*,#13973,.T.);
#17892=ORIENTED_EDGE('',*,*,#13974,.F.);
#17893=ORIENTED_EDGE('',*,*,#13971,.F.);
#17894=ORIENTED_EDGE('',*,*,#13947,.F.);
#17895=ORIENTED_EDGE('',*,*,#13975,.T.);
#17896=ORIENTED_EDGE('',*,*,#13976,.F.);
#17897=ORIENTED_EDGE('',*,*,#13973,.F.);
#17898=ORIENTED_EDGE('',*,*,#13945,.F.);
#17899=ORIENTED_EDGE('',*,*,#13967,.F.);
#17900=ORIENTED_EDGE('',*,*,#13965,.F.);
#17901=ORIENTED_EDGE('',*,*,#13962,.F.);
#17902=ORIENTED_EDGE('',*,*,#13959,.F.);
#17903=ORIENTED_EDGE('',*,*,#13956,.F.);
#17904=ORIENTED_EDGE('',*,*,#13953,.F.);
#17905=ORIENTED_EDGE('',*,*,#13950,.F.);
#17906=ORIENTED_EDGE('',*,*,#13977,.T.);
#17907=ORIENTED_EDGE('',*,*,#13978,.T.);
#17908=ORIENTED_EDGE('',*,*,#13979,.T.);
#17909=ORIENTED_EDGE('',*,*,#13980,.T.);
#17910=ORIENTED_EDGE('',*,*,#13981,.T.);
#17911=ORIENTED_EDGE('',*,*,#13982,.T.);
#17912=ORIENTED_EDGE('',*,*,#13983,.T.);
#17913=ORIENTED_EDGE('',*,*,#13984,.T.);
#17914=ORIENTED_EDGE('',*,*,#13981,.F.);
#17915=ORIENTED_EDGE('',*,*,#13985,.T.);
#17916=ORIENTED_EDGE('',*,*,#13986,.T.);
#17917=ORIENTED_EDGE('',*,*,#13987,.T.);
#17918=ORIENTED_EDGE('',*,*,#13983,.F.);
#17919=ORIENTED_EDGE('',*,*,#13988,.T.);
#17920=ORIENTED_EDGE('',*,*,#13989,.T.);
#17921=ORIENTED_EDGE('',*,*,#13990,.T.);
#17922=ORIENTED_EDGE('',*,*,#13986,.F.);
#17923=ORIENTED_EDGE('',*,*,#13969,.T.);
#17924=ORIENTED_EDGE('',*,*,#13991,.T.);
#17925=ORIENTED_EDGE('',*,*,#13992,.T.);
#17926=ORIENTED_EDGE('',*,*,#13989,.F.);
#17927=ORIENTED_EDGE('',*,*,#13972,.T.);
#17928=ORIENTED_EDGE('',*,*,#13993,.T.);
#17929=ORIENTED_EDGE('',*,*,#13994,.T.);
#17930=ORIENTED_EDGE('',*,*,#13991,.F.);
#17931=ORIENTED_EDGE('',*,*,#13974,.T.);
#17932=ORIENTED_EDGE('',*,*,#13995,.T.);
#17933=ORIENTED_EDGE('',*,*,#13996,.T.);
#17934=ORIENTED_EDGE('',*,*,#13993,.F.);
#17935=ORIENTED_EDGE('',*,*,#13976,.T.);
#17936=ORIENTED_EDGE('',*,*,#13979,.F.);
#17937=ORIENTED_EDGE('',*,*,#13997,.T.);
#17938=ORIENTED_EDGE('',*,*,#13995,.F.);
#17939=ORIENTED_EDGE('',*,*,#13998,.T.);
#17940=ORIENTED_EDGE('',*,*,#13958,.F.);
#17941=ORIENTED_EDGE('',*,*,#13970,.T.);
#17942=ORIENTED_EDGE('',*,*,#13988,.F.);
#17943=ORIENTED_EDGE('',*,*,#13999,.F.);
#17944=ORIENTED_EDGE('',*,*,#13955,.F.);
#17945=ORIENTED_EDGE('',*,*,#13999,.T.);
#17946=ORIENTED_EDGE('',*,*,#13985,.F.);
#17947=ORIENTED_EDGE('',*,*,#14000,.F.);
#17948=ORIENTED_EDGE('',*,*,#13952,.F.);
#17949=ORIENTED_EDGE('',*,*,#14000,.T.);
#17950=ORIENTED_EDGE('',*,*,#13980,.F.);
#17951=ORIENTED_EDGE('',*,*,#14001,.F.);
#17952=ORIENTED_EDGE('',*,*,#13982,.F.);
#17953=ORIENTED_EDGE('',*,*,#13984,.F.);
#17954=ORIENTED_EDGE('',*,*,#13987,.F.);
#17955=ORIENTED_EDGE('',*,*,#13990,.F.);
#17956=ORIENTED_EDGE('',*,*,#13992,.F.);
#17957=ORIENTED_EDGE('',*,*,#13994,.F.);
#17958=ORIENTED_EDGE('',*,*,#13996,.F.);
#17959=ORIENTED_EDGE('',*,*,#13997,.F.);
#17960=ORIENTED_EDGE('',*,*,#14002,.F.);
#17961=ORIENTED_EDGE('',*,*,#14003,.F.);
#17962=ORIENTED_EDGE('',*,*,#14004,.F.);
#17963=ORIENTED_EDGE('',*,*,#14005,.F.);
#17964=ORIENTED_EDGE('',*,*,#14006,.F.);
#17965=ORIENTED_EDGE('',*,*,#14007,.F.);
#17966=ORIENTED_EDGE('',*,*,#14008,.F.);
#17967=ORIENTED_EDGE('',*,*,#14009,.F.);
#17968=ORIENTED_EDGE('',*,*,#14010,.T.);
#17969=ORIENTED_EDGE('',*,*,#14011,.T.);
#17970=ORIENTED_EDGE('',*,*,#14012,.T.);
#17971=ORIENTED_EDGE('',*,*,#14013,.T.);
#17972=ORIENTED_EDGE('',*,*,#14014,.T.);
#17973=ORIENTED_EDGE('',*,*,#14015,.T.);
#17974=ORIENTED_EDGE('',*,*,#14016,.T.);
#17975=ORIENTED_EDGE('',*,*,#14017,.T.);
#17976=ORIENTED_EDGE('',*,*,#14014,.F.);
#17977=ORIENTED_EDGE('',*,*,#14018,.T.);
#17978=ORIENTED_EDGE('',*,*,#14019,.T.);
#17979=ORIENTED_EDGE('',*,*,#14020,.T.);
#17980=ORIENTED_EDGE('',*,*,#14016,.F.);
#17981=ORIENTED_EDGE('',*,*,#14021,.T.);
#17982=ORIENTED_EDGE('',*,*,#14022,.T.);
#17983=ORIENTED_EDGE('',*,*,#14023,.T.);
#17984=ORIENTED_EDGE('',*,*,#14019,.F.);
#17985=ORIENTED_EDGE('',*,*,#14024,.T.);
#17986=ORIENTED_EDGE('',*,*,#14025,.T.);
#17987=ORIENTED_EDGE('',*,*,#14026,.T.);
#17988=ORIENTED_EDGE('',*,*,#14022,.F.);
#17989=ORIENTED_EDGE('',*,*,#14027,.T.);
#17990=ORIENTED_EDGE('',*,*,#14028,.T.);
#17991=ORIENTED_EDGE('',*,*,#14029,.T.);
#17992=ORIENTED_EDGE('',*,*,#14025,.F.);
#17993=ORIENTED_EDGE('',*,*,#14030,.T.);
#17994=ORIENTED_EDGE('',*,*,#14031,.T.);
#17995=ORIENTED_EDGE('',*,*,#14032,.T.);
#17996=ORIENTED_EDGE('',*,*,#14028,.F.);
#17997=ORIENTED_EDGE('',*,*,#14033,.T.);
#17998=ORIENTED_EDGE('',*,*,#14012,.F.);
#17999=ORIENTED_EDGE('',*,*,#14034,.T.);
#18000=ORIENTED_EDGE('',*,*,#14031,.F.);
#18001=ORIENTED_EDGE('',*,*,#14035,.T.);
#18002=ORIENTED_EDGE('',*,*,#14024,.F.);
#18003=ORIENTED_EDGE('',*,*,#14036,.F.);
#18004=ORIENTED_EDGE('',*,*,#14037,.F.);
#18005=ORIENTED_EDGE('',*,*,#14038,.T.);
#18006=ORIENTED_EDGE('',*,*,#14021,.F.);
#18007=ORIENTED_EDGE('',*,*,#14039,.F.);
#18008=ORIENTED_EDGE('',*,*,#14040,.F.);
#18009=ORIENTED_EDGE('',*,*,#14036,.T.);
#18010=ORIENTED_EDGE('',*,*,#14018,.F.);
#18011=ORIENTED_EDGE('',*,*,#14041,.F.);
#18012=ORIENTED_EDGE('',*,*,#14042,.F.);
#18013=ORIENTED_EDGE('',*,*,#14039,.T.);
#18014=ORIENTED_EDGE('',*,*,#14013,.F.);
#18015=ORIENTED_EDGE('',*,*,#14043,.F.);
#18016=ORIENTED_EDGE('',*,*,#14044,.F.);
#18017=ORIENTED_EDGE('',*,*,#14041,.T.);
#18018=ORIENTED_EDGE('',*,*,#14015,.F.);
#18019=ORIENTED_EDGE('',*,*,#14017,.F.);
#18020=ORIENTED_EDGE('',*,*,#14020,.F.);
#18021=ORIENTED_EDGE('',*,*,#14023,.F.);
#18022=ORIENTED_EDGE('',*,*,#14026,.F.);
#18023=ORIENTED_EDGE('',*,*,#14029,.F.);
#18024=ORIENTED_EDGE('',*,*,#14032,.F.);
#18025=ORIENTED_EDGE('',*,*,#14034,.F.);
#18026=ORIENTED_EDGE('',*,*,#14045,.T.);
#18027=ORIENTED_EDGE('',*,*,#14046,.T.);
#18028=ORIENTED_EDGE('',*,*,#14047,.T.);
#18029=ORIENTED_EDGE('',*,*,#14048,.T.);
#18030=ORIENTED_EDGE('',*,*,#14049,.T.);
#18031=ORIENTED_EDGE('',*,*,#14050,.T.);
#18032=ORIENTED_EDGE('',*,*,#14051,.T.);
#18033=ORIENTED_EDGE('',*,*,#14048,.F.);
#18034=ORIENTED_EDGE('',*,*,#14052,.T.);
#18035=ORIENTED_EDGE('',*,*,#14053,.T.);
#18036=ORIENTED_EDGE('',*,*,#14054,.T.);
#18037=ORIENTED_EDGE('',*,*,#14050,.F.);
#18038=ORIENTED_EDGE('',*,*,#14055,.T.);
#18039=ORIENTED_EDGE('',*,*,#14056,.T.);
#18040=ORIENTED_EDGE('',*,*,#14057,.T.);
#18041=ORIENTED_EDGE('',*,*,#14053,.F.);
#18042=ORIENTED_EDGE('',*,*,#14058,.T.);
#18043=ORIENTED_EDGE('',*,*,#14059,.T.);
#18044=ORIENTED_EDGE('',*,*,#14060,.T.);
#18045=ORIENTED_EDGE('',*,*,#14056,.F.);
#18046=ORIENTED_EDGE('',*,*,#14061,.T.);
#18047=ORIENTED_EDGE('',*,*,#14062,.T.);
#18048=ORIENTED_EDGE('',*,*,#14063,.T.);
#18049=ORIENTED_EDGE('',*,*,#14059,.F.);
#18050=ORIENTED_EDGE('',*,*,#14064,.T.);
#18051=ORIENTED_EDGE('',*,*,#14065,.T.);
#18052=ORIENTED_EDGE('',*,*,#14066,.T.);
#18053=ORIENTED_EDGE('',*,*,#14062,.F.);
#18054=ORIENTED_EDGE('',*,*,#14067,.T.);
#18055=ORIENTED_EDGE('',*,*,#14046,.F.);
#18056=ORIENTED_EDGE('',*,*,#14068,.T.);
#18057=ORIENTED_EDGE('',*,*,#14065,.F.);
#18058=ORIENTED_EDGE('',*,*,#14069,.T.);
#18059=ORIENTED_EDGE('',*,*,#14058,.F.);
#18060=ORIENTED_EDGE('',*,*,#14070,.F.);
#18061=ORIENTED_EDGE('',*,*,#14071,.F.);
#18062=ORIENTED_EDGE('',*,*,#14072,.T.);
#18063=ORIENTED_EDGE('',*,*,#14055,.F.);
#18064=ORIENTED_EDGE('',*,*,#14073,.F.);
#18065=ORIENTED_EDGE('',*,*,#14074,.F.);
#18066=ORIENTED_EDGE('',*,*,#14070,.T.);
#18067=ORIENTED_EDGE('',*,*,#14052,.F.);
#18068=ORIENTED_EDGE('',*,*,#14075,.F.);
#18069=ORIENTED_EDGE('',*,*,#14076,.F.);
#18070=ORIENTED_EDGE('',*,*,#14073,.T.);
#18071=ORIENTED_EDGE('',*,*,#14047,.F.);
#18072=ORIENTED_EDGE('',*,*,#14077,.F.);
#18073=ORIENTED_EDGE('',*,*,#14078,.F.);
#18074=ORIENTED_EDGE('',*,*,#14075,.T.);
#18075=ORIENTED_EDGE('',*,*,#14049,.F.);
#18076=ORIENTED_EDGE('',*,*,#14051,.F.);
#18077=ORIENTED_EDGE('',*,*,#14054,.F.);
#18078=ORIENTED_EDGE('',*,*,#14057,.F.);
#18079=ORIENTED_EDGE('',*,*,#14060,.F.);
#18080=ORIENTED_EDGE('',*,*,#14063,.F.);
#18081=ORIENTED_EDGE('',*,*,#14066,.F.);
#18082=ORIENTED_EDGE('',*,*,#14068,.F.);
#18083=ORIENTED_EDGE('',*,*,#14079,.T.);
#18084=ORIENTED_EDGE('',*,*,#13943,.T.);
#18085=ORIENTED_EDGE('',*,*,#14080,.T.);
#18086=ORIENTED_EDGE('',*,*,#14081,.T.);
#18087=ORIENTED_EDGE('',*,*,#14080,.F.);
#18088=ORIENTED_EDGE('',*,*,#14081,.F.);
#18089=ORIENTED_EDGE('',*,*,#14082,.T.);
#18090=ORIENTED_EDGE('',*,*,#14083,.T.);
#18091=ORIENTED_EDGE('',*,*,#14084,.F.);
#18092=ORIENTED_EDGE('',*,*,#14085,.F.);
#18093=ORIENTED_EDGE('',*,*,#14086,.T.);
#18094=ORIENTED_EDGE('',*,*,#14087,.F.);
#18095=ORIENTED_EDGE('',*,*,#14088,.T.);
#18096=ORIENTED_EDGE('',*,*,#14089,.T.);
#18097=ORIENTED_EDGE('',*,*,#14082,.F.);
#18098=ORIENTED_EDGE('',*,*,#14090,.T.);
#18099=ORIENTED_EDGE('',*,*,#14091,.T.);
#18100=ORIENTED_EDGE('',*,*,#14092,.T.);
#18101=ORIENTED_EDGE('',*,*,#14091,.F.);
#18102=ORIENTED_EDGE('',*,*,#14093,.F.);
#18103=ORIENTED_EDGE('',*,*,#14086,.F.);
#18104=ORIENTED_EDGE('',*,*,#14094,.F.);
#18105=ORIENTED_EDGE('',*,*,#14095,.F.);
#18106=ORIENTED_EDGE('',*,*,#14090,.F.);
#18107=ORIENTED_EDGE('',*,*,#14092,.F.);
#18108=ORIENTED_EDGE('',*,*,#14096,.T.);
#18109=ORIENTED_EDGE('',*,*,#14097,.T.);
#18110=ORIENTED_EDGE('',*,*,#14096,.F.);
#18111=ORIENTED_EDGE('',*,*,#14098,.T.);
#18112=ORIENTED_EDGE('',*,*,#14087,.T.);
#18113=ORIENTED_EDGE('',*,*,#14093,.T.);
#18114=ORIENTED_EDGE('',*,*,#14099,.T.);
#18115=ORIENTED_EDGE('',*,*,#14100,.T.);
#18116=ORIENTED_EDGE('',*,*,#14099,.F.);
#18117=ORIENTED_EDGE('',*,*,#14095,.T.);
#18118=ORIENTED_EDGE('',*,*,#14101,.T.);
#18119=ORIENTED_EDGE('',*,*,#14094,.T.);
#18120=ORIENTED_EDGE('',*,*,#14085,.T.);
#18121=ORIENTED_EDGE('',*,*,#14102,.T.);
#18122=ORIENTED_EDGE('',*,*,#14101,.F.);
#18123=ORIENTED_EDGE('',*,*,#14098,.F.);
#18124=ORIENTED_EDGE('',*,*,#14103,.T.);
#18125=ORIENTED_EDGE('',*,*,#14104,.T.);
#18126=ORIENTED_EDGE('',*,*,#14088,.F.);
#18127=ORIENTED_EDGE('',*,*,#14100,.F.);
#18128=ORIENTED_EDGE('',*,*,#14105,.T.);
#18129=ORIENTED_EDGE('',*,*,#14106,.T.);
#18130=ORIENTED_EDGE('',*,*,#14103,.F.);
#18131=ORIENTED_EDGE('',*,*,#14102,.F.);
#18132=ORIENTED_EDGE('',*,*,#14084,.T.);
#18133=ORIENTED_EDGE('',*,*,#14107,.T.);
#18134=ORIENTED_EDGE('',*,*,#14105,.F.);
#18135=ORIENTED_EDGE('',*,*,#14108,.T.);
#18136=ORIENTED_EDGE('',*,*,#14109,.T.);
#18137=ORIENTED_EDGE('',*,*,#14110,.T.);
#18138=ORIENTED_EDGE('',*,*,#14111,.T.);
#18139=ORIENTED_EDGE('',*,*,#14112,.T.);
#18140=ORIENTED_EDGE('',*,*,#14113,.T.);
#18141=ORIENTED_EDGE('',*,*,#14114,.T.);
#18142=ORIENTED_EDGE('',*,*,#14111,.F.);
#18143=ORIENTED_EDGE('',*,*,#14115,.T.);
#18144=ORIENTED_EDGE('',*,*,#14116,.T.);
#18145=ORIENTED_EDGE('',*,*,#14117,.T.);
#18146=ORIENTED_EDGE('',*,*,#14113,.F.);
#18147=ORIENTED_EDGE('',*,*,#14118,.T.);
#18148=ORIENTED_EDGE('',*,*,#14108,.F.);
#18149=ORIENTED_EDGE('',*,*,#14119,.T.);
#18150=ORIENTED_EDGE('',*,*,#14116,.F.);
#18151=ORIENTED_EDGE('',*,*,#14120,.T.);
#18152=ORIENTED_EDGE('',*,*,#14119,.F.);
#18153=ORIENTED_EDGE('',*,*,#14121,.T.);
#18154=ORIENTED_EDGE('',*,*,#14122,.F.);
#18155=ORIENTED_EDGE('',*,*,#14123,.F.);
#18156=ORIENTED_EDGE('',*,*,#14124,.T.);
#18157=ORIENTED_EDGE('',*,*,#14125,.T.);
#18158=ORIENTED_EDGE('',*,*,#14112,.F.);
#18159=ORIENTED_EDGE('',*,*,#14126,.T.);
#18160=ORIENTED_EDGE('',*,*,#14127,.F.);
#18161=ORIENTED_EDGE('',*,*,#14121,.F.);
#18162=ORIENTED_EDGE('',*,*,#14109,.F.);
#18163=ORIENTED_EDGE('',*,*,#14120,.F.);
#18164=ORIENTED_EDGE('',*,*,#14118,.F.);
#18165=ORIENTED_EDGE('',*,*,#14115,.F.);
#18166=ORIENTED_EDGE('',*,*,#14110,.F.);
#18167=ORIENTED_EDGE('',*,*,#14128,.T.);
#18168=ORIENTED_EDGE('',*,*,#14129,.T.);
#18169=ORIENTED_EDGE('',*,*,#14128,.F.);
#18170=ORIENTED_EDGE('',*,*,#13925,.T.);
#18171=ORIENTED_EDGE('',*,*,#14130,.T.);
#18172=ORIENTED_EDGE('',*,*,#14131,.T.);
#18173=ORIENTED_EDGE('',*,*,#14132,.T.);
#18174=ORIENTED_EDGE('',*,*,#13910,.F.);
#18175=ORIENTED_EDGE('',*,*,#14133,.T.);
#18176=ORIENTED_EDGE('',*,*,#14134,.T.);
#18177=ORIENTED_EDGE('',*,*,#14135,.T.);
#18178=ORIENTED_EDGE('',*,*,#14136,.T.);
#18179=ORIENTED_EDGE('',*,*,#14137,.T.);
#18180=ORIENTED_EDGE('',*,*,#14138,.T.);
#18181=ORIENTED_EDGE('',*,*,#14135,.F.);
#18182=ORIENTED_EDGE('',*,*,#14139,.T.);
#18183=ORIENTED_EDGE('',*,*,#13923,.T.);
#18184=ORIENTED_EDGE('',*,*,#14140,.T.);
#18185=ORIENTED_EDGE('',*,*,#14137,.F.);
#18186=ORIENTED_EDGE('',*,*,#14141,.T.);
#18187=ORIENTED_EDGE('',*,*,#14133,.F.);
#18188=ORIENTED_EDGE('',*,*,#14142,.T.);
#18189=ORIENTED_EDGE('',*,*,#14131,.F.);
#18190=ORIENTED_EDGE('',*,*,#14143,.T.);
#18191=ORIENTED_EDGE('',*,*,#14138,.F.);
#18192=ORIENTED_EDGE('',*,*,#14144,.T.);
#18193=ORIENTED_EDGE('',*,*,#14145,.F.);
#18194=ORIENTED_EDGE('',*,*,#14146,.F.);
#18195=ORIENTED_EDGE('',*,*,#14147,.F.);
#18196=ORIENTED_EDGE('',*,*,#14148,.F.);
#18197=ORIENTED_EDGE('',*,*,#14140,.F.);
#18198=ORIENTED_EDGE('',*,*,#13933,.F.);
#18199=ORIENTED_EDGE('',*,*,#14149,.T.);
#18200=ORIENTED_EDGE('',*,*,#14123,.T.);
#18201=ORIENTED_EDGE('',*,*,#14150,.F.);
#18202=ORIENTED_EDGE('',*,*,#14144,.F.);
#18203=ORIENTED_EDGE('',*,*,#14141,.F.);
#18204=ORIENTED_EDGE('',*,*,#14139,.F.);
#18205=ORIENTED_EDGE('',*,*,#14134,.F.);
#18206=ORIENTED_EDGE('',*,*,#14143,.F.);
#18207=ORIENTED_EDGE('',*,*,#14130,.F.);
#18208=ORIENTED_EDGE('',*,*,#13924,.F.);
#18209=ORIENTED_EDGE('',*,*,#14151,.T.);
#18210=ORIENTED_EDGE('',*,*,#14152,.T.);
#18211=ORIENTED_EDGE('',*,*,#14153,.T.);
#18212=ORIENTED_EDGE('',*,*,#14154,.T.);
#18213=ORIENTED_EDGE('',*,*,#14155,.T.);
#18214=ORIENTED_EDGE('',*,*,#14156,.T.);
#18215=ORIENTED_EDGE('',*,*,#14153,.F.);
#18216=ORIENTED_EDGE('',*,*,#14145,.T.);
#18217=ORIENTED_EDGE('',*,*,#14157,.T.);
#18218=ORIENTED_EDGE('',*,*,#14158,.T.);
#18219=ORIENTED_EDGE('',*,*,#14155,.F.);
#18220=ORIENTED_EDGE('',*,*,#14150,.T.);
#18221=ORIENTED_EDGE('',*,*,#14159,.T.);
#18222=ORIENTED_EDGE('',*,*,#14160,.T.);
#18223=ORIENTED_EDGE('',*,*,#14157,.F.);
#18224=ORIENTED_EDGE('',*,*,#14122,.T.);
#18225=ORIENTED_EDGE('',*,*,#14161,.T.);
#18226=ORIENTED_EDGE('',*,*,#14162,.T.);
#18227=ORIENTED_EDGE('',*,*,#14159,.F.);
#18228=ORIENTED_EDGE('',*,*,#14127,.T.);
#18229=ORIENTED_EDGE('',*,*,#14163,.T.);
#18230=ORIENTED_EDGE('',*,*,#14164,.T.);
#18231=ORIENTED_EDGE('',*,*,#14161,.F.);
#18232=ORIENTED_EDGE('',*,*,#14165,.T.);
#18233=ORIENTED_EDGE('',*,*,#14166,.T.);
#18234=ORIENTED_EDGE('',*,*,#14167,.T.);
#18235=ORIENTED_EDGE('',*,*,#14163,.F.);
#18236=ORIENTED_EDGE('',*,*,#14168,.T.);
#18237=ORIENTED_EDGE('',*,*,#14151,.F.);
#18238=ORIENTED_EDGE('',*,*,#14169,.T.);
#18239=ORIENTED_EDGE('',*,*,#14166,.F.);
#18240=ORIENTED_EDGE('',*,*,#14170,.T.);
#18241=ORIENTED_EDGE('',*,*,#14152,.F.);
#18242=ORIENTED_EDGE('',*,*,#14171,.F.);
#18243=ORIENTED_EDGE('',*,*,#14172,.F.);
#18244=ORIENTED_EDGE('',*,*,#14146,.T.);
#18245=ORIENTED_EDGE('',*,*,#14154,.F.);
#18246=ORIENTED_EDGE('',*,*,#14156,.F.);
#18247=ORIENTED_EDGE('',*,*,#14158,.F.);
#18248=ORIENTED_EDGE('',*,*,#14160,.F.);
#18249=ORIENTED_EDGE('',*,*,#14162,.F.);
#18250=ORIENTED_EDGE('',*,*,#14164,.F.);
#18251=ORIENTED_EDGE('',*,*,#14167,.F.);
#18252=ORIENTED_EDGE('',*,*,#14169,.F.);
#18253=ORIENTED_EDGE('',*,*,#14044,.T.);
#18254=ORIENTED_EDGE('',*,*,#14173,.T.);
#18255=ORIENTED_EDGE('',*,*,#14174,.T.);
#18256=ORIENTED_EDGE('',*,*,#14175,.T.);
#18257=ORIENTED_EDGE('',*,*,#14176,.T.);
#18258=ORIENTED_EDGE('',*,*,#14037,.T.);
#18259=ORIENTED_EDGE('',*,*,#14040,.T.);
#18260=ORIENTED_EDGE('',*,*,#14042,.T.);
#18261=ORIENTED_EDGE('',*,*,#14078,.T.);
#18262=ORIENTED_EDGE('',*,*,#14177,.T.);
#18263=ORIENTED_EDGE('',*,*,#14178,.T.);
#18264=ORIENTED_EDGE('',*,*,#14179,.T.);
#18265=ORIENTED_EDGE('',*,*,#14180,.T.);
#18266=ORIENTED_EDGE('',*,*,#14071,.T.);
#18267=ORIENTED_EDGE('',*,*,#14074,.T.);
#18268=ORIENTED_EDGE('',*,*,#14076,.T.);
#18269=ORIENTED_EDGE('',*,*,#14181,.T.);
#18270=ORIENTED_EDGE('',*,*,#14182,.T.);
#18271=ORIENTED_EDGE('',*,*,#14183,.T.);
#18272=ORIENTED_EDGE('',*,*,#14184,.T.);
#18273=ORIENTED_EDGE('',*,*,#14185,.T.);
#18274=ORIENTED_EDGE('',*,*,#14172,.T.);
#18275=ORIENTED_EDGE('',*,*,#14186,.T.);
#18276=ORIENTED_EDGE('',*,*,#14147,.T.);
#18277=ORIENTED_EDGE('',*,*,#14185,.F.);
#18278=ORIENTED_EDGE('',*,*,#14187,.T.);
#18279=ORIENTED_EDGE('',*,*,#14188,.T.);
#18280=ORIENTED_EDGE('',*,*,#14189,.T.);
#18281=ORIENTED_EDGE('',*,*,#14186,.F.);
#18282=ORIENTED_EDGE('',*,*,#14190,.T.);
#18283=ORIENTED_EDGE('',*,*,#14182,.F.);
#18284=ORIENTED_EDGE('',*,*,#14191,.T.);
#18285=ORIENTED_EDGE('',*,*,#14188,.F.);
#18286=ORIENTED_EDGE('',*,*,#14192,.T.);
#18287=ORIENTED_EDGE('',*,*,#14142,.F.);
#18288=ORIENTED_EDGE('',*,*,#14193,.T.);
#18289=ORIENTED_EDGE('',*,*,#14191,.F.);
#18290=ORIENTED_EDGE('',*,*,#14171,.T.);
#18291=ORIENTED_EDGE('',*,*,#14170,.F.);
#18292=ORIENTED_EDGE('',*,*,#14194,.F.);
#18293=ORIENTED_EDGE('',*,*,#14183,.F.);
#18294=ORIENTED_EDGE('',*,*,#14192,.F.);
#18295=ORIENTED_EDGE('',*,*,#14190,.F.);
#18296=ORIENTED_EDGE('',*,*,#14187,.F.);
#18297=ORIENTED_EDGE('',*,*,#14184,.F.);
#18298=ORIENTED_EDGE('',*,*,#14195,.T.);
#18299=ORIENTED_EDGE('',*,*,#14196,.T.);
#18300=ORIENTED_EDGE('',*,*,#14195,.F.);
#18301=ORIENTED_EDGE('',*,*,#14011,.F.);
#18302=ORIENTED_EDGE('',*,*,#14197,.T.);
#18303=ORIENTED_EDGE('',*,*,#13978,.F.);
#18304=ORIENTED_EDGE('',*,*,#14197,.F.);
#18305=ORIENTED_EDGE('',*,*,#14010,.F.);
#18306=ORIENTED_EDGE('',*,*,#14198,.T.);
#18307=ORIENTED_EDGE('',*,*,#13977,.F.);
#18308=ORIENTED_EDGE('',*,*,#14198,.F.);
#18309=ORIENTED_EDGE('',*,*,#14045,.F.);
#18310=ORIENTED_EDGE('',*,*,#14199,.T.);
#18311=ORIENTED_EDGE('',*,*,#14200,.T.);
#18312=ORIENTED_EDGE('',*,*,#14199,.F.);
#18313=ORIENTED_EDGE('',*,*,#14200,.F.);
#18314=ORIENTED_EDGE('',*,*,#14079,.F.);
#18315=ORIENTED_EDGE('',*,*,#14201,.T.);
#18316=ORIENTED_EDGE('',*,*,#14202,.T.);
#18317=ORIENTED_EDGE('',*,*,#14201,.F.);
#18318=ORIENTED_EDGE('',*,*,#14202,.F.);
#18319=ORIENTED_EDGE('',*,*,#14181,.F.);
#18320=ORIENTED_EDGE('',*,*,#14203,.T.);
#18321=ORIENTED_EDGE('',*,*,#14204,.T.);
#18322=ORIENTED_EDGE('',*,*,#14203,.F.);
#18323=ORIENTED_EDGE('',*,*,#14204,.F.);
#18324=ORIENTED_EDGE('',*,*,#14196,.F.);
#18325=ORIENTED_EDGE('',*,*,#14136,.F.);
#18326=ORIENTED_EDGE('',*,*,#14148,.T.);
#18327=ORIENTED_EDGE('',*,*,#14189,.F.);
#18328=ORIENTED_EDGE('',*,*,#14193,.F.);
#18329=ORIENTED_EDGE('',*,*,#14129,.F.);
#18330=ORIENTED_EDGE('',*,*,#14117,.F.);
#18331=ORIENTED_EDGE('',*,*,#14125,.F.);
#18332=ORIENTED_EDGE('',*,*,#14205,.T.);
#18333=ORIENTED_EDGE('',*,*,#14206,.T.);
#18334=ORIENTED_EDGE('',*,*,#13926,.F.);
#18335=ORIENTED_EDGE('',*,*,#14207,.T.);
#18336=ORIENTED_EDGE('',*,*,#14208,.T.);
#18337=ORIENTED_EDGE('',*,*,#14207,.F.);
#18338=ORIENTED_EDGE('',*,*,#14208,.F.);
#18339=ORIENTED_EDGE('',*,*,#13927,.F.);
#18340=ORIENTED_EDGE('',*,*,#14209,.T.);
#18341=ORIENTED_EDGE('',*,*,#14210,.T.);
#18342=ORIENTED_EDGE('',*,*,#14209,.F.);
#18343=ORIENTED_EDGE('',*,*,#14210,.F.);
#18344=ORIENTED_EDGE('',*,*,#13928,.F.);
#18345=ORIENTED_EDGE('',*,*,#14211,.T.);
#18346=ORIENTED_EDGE('',*,*,#14212,.T.);
#18347=ORIENTED_EDGE('',*,*,#14211,.F.);
#18348=ORIENTED_EDGE('',*,*,#14212,.F.);
#18349=ORIENTED_EDGE('',*,*,#13929,.F.);
#18350=ORIENTED_EDGE('',*,*,#14213,.T.);
#18351=ORIENTED_EDGE('',*,*,#14214,.T.);
#18352=ORIENTED_EDGE('',*,*,#14213,.F.);
#18353=ORIENTED_EDGE('',*,*,#14214,.F.);
#18354=ORIENTED_EDGE('',*,*,#13935,.F.);
#18355=ORIENTED_EDGE('',*,*,#14215,.T.);
#18356=ORIENTED_EDGE('',*,*,#14216,.T.);
#18357=ORIENTED_EDGE('',*,*,#14215,.F.);
#18358=ORIENTED_EDGE('',*,*,#14216,.F.);
#18359=ORIENTED_EDGE('',*,*,#13936,.F.);
#18360=ORIENTED_EDGE('',*,*,#14217,.T.);
#18361=ORIENTED_EDGE('',*,*,#14218,.T.);
#18362=ORIENTED_EDGE('',*,*,#14217,.F.);
#18363=ORIENTED_EDGE('',*,*,#14218,.F.);
#18364=ORIENTED_EDGE('',*,*,#13937,.F.);
#18365=ORIENTED_EDGE('',*,*,#14219,.T.);
#18366=ORIENTED_EDGE('',*,*,#14220,.T.);
#18367=ORIENTED_EDGE('',*,*,#14219,.F.);
#18368=ORIENTED_EDGE('',*,*,#14220,.F.);
#18369=ORIENTED_EDGE('',*,*,#13938,.F.);
#18370=ORIENTED_EDGE('',*,*,#14221,.T.);
#18371=ORIENTED_EDGE('',*,*,#14222,.T.);
#18372=ORIENTED_EDGE('',*,*,#14221,.F.);
#18373=ORIENTED_EDGE('',*,*,#14222,.F.);
#18374=ORIENTED_EDGE('',*,*,#13939,.F.);
#18375=ORIENTED_EDGE('',*,*,#14223,.T.);
#18376=ORIENTED_EDGE('',*,*,#14224,.T.);
#18377=ORIENTED_EDGE('',*,*,#14223,.F.);
#18378=ORIENTED_EDGE('',*,*,#14224,.F.);
#18379=ORIENTED_EDGE('',*,*,#13940,.F.);
#18380=ORIENTED_EDGE('',*,*,#14225,.T.);
#18381=ORIENTED_EDGE('',*,*,#14226,.T.);
#18382=ORIENTED_EDGE('',*,*,#14225,.F.);
#18383=ORIENTED_EDGE('',*,*,#14226,.F.);
#18384=ORIENTED_EDGE('',*,*,#13941,.F.);
#18385=ORIENTED_EDGE('',*,*,#14227,.T.);
#18386=ORIENTED_EDGE('',*,*,#14228,.T.);
#18387=ORIENTED_EDGE('',*,*,#14227,.F.);
#18388=ORIENTED_EDGE('',*,*,#14228,.F.);
#18389=ORIENTED_EDGE('',*,*,#13942,.F.);
#18390=ORIENTED_EDGE('',*,*,#14229,.T.);
#18391=ORIENTED_EDGE('',*,*,#14230,.T.);
#18392=ORIENTED_EDGE('',*,*,#14229,.F.);
#18393=ORIENTED_EDGE('',*,*,#14230,.F.);
#18394=ORIENTED_EDGE('',*,*,#14107,.F.);
#18395=ORIENTED_EDGE('',*,*,#14083,.F.);
#18396=ORIENTED_EDGE('',*,*,#14089,.F.);
#18397=ORIENTED_EDGE('',*,*,#14104,.F.);
#18398=ORIENTED_EDGE('',*,*,#14106,.F.);
#18399=ORIENTED_EDGE('',*,*,#14097,.F.);
#18400=ORIENTED_EDGE('',*,*,#14231,.T.);
#18401=ORIENTED_EDGE('',*,*,#14231,.F.);
#18402=ORIENTED_EDGE('',*,*,#14232,.T.);
#18403=ORIENTED_EDGE('',*,*,#13930,.F.);
#18404=ORIENTED_EDGE('',*,*,#14232,.F.);
#18405=ORIENTED_EDGE('',*,*,#14069,.F.);
#18406=ORIENTED_EDGE('',*,*,#14233,.F.);
#18407=ORIENTED_EDGE('',*,*,#14177,.F.);
#18408=ORIENTED_EDGE('',*,*,#14077,.T.);
#18409=ORIENTED_EDGE('',*,*,#14067,.F.);
#18410=ORIENTED_EDGE('',*,*,#14234,.F.);
#18411=ORIENTED_EDGE('',*,*,#14178,.F.);
#18412=ORIENTED_EDGE('',*,*,#14233,.T.);
#18413=ORIENTED_EDGE('',*,*,#14064,.F.);
#18414=ORIENTED_EDGE('',*,*,#14235,.F.);
#18415=ORIENTED_EDGE('',*,*,#14179,.F.);
#18416=ORIENTED_EDGE('',*,*,#14234,.T.);
#18417=ORIENTED_EDGE('',*,*,#14061,.F.);
#18418=ORIENTED_EDGE('',*,*,#14072,.F.);
#18419=ORIENTED_EDGE('',*,*,#14180,.F.);
#18420=ORIENTED_EDGE('',*,*,#14235,.T.);
#18421=ORIENTED_EDGE('',*,*,#14035,.F.);
#18422=ORIENTED_EDGE('',*,*,#14236,.F.);
#18423=ORIENTED_EDGE('',*,*,#14173,.F.);
#18424=ORIENTED_EDGE('',*,*,#14043,.T.);
#18425=ORIENTED_EDGE('',*,*,#14033,.F.);
#18426=ORIENTED_EDGE('',*,*,#14237,.F.);
#18427=ORIENTED_EDGE('',*,*,#14174,.F.);
#18428=ORIENTED_EDGE('',*,*,#14236,.T.);
#18429=ORIENTED_EDGE('',*,*,#14030,.F.);
#18430=ORIENTED_EDGE('',*,*,#14238,.F.);
#18431=ORIENTED_EDGE('',*,*,#14175,.F.);
#18432=ORIENTED_EDGE('',*,*,#14237,.T.);
#18433=ORIENTED_EDGE('',*,*,#14027,.F.);
#18434=ORIENTED_EDGE('',*,*,#14038,.F.);
#18435=ORIENTED_EDGE('',*,*,#14176,.F.);
#18436=ORIENTED_EDGE('',*,*,#14238,.T.);
#18437=ORIENTED_EDGE('',*,*,#13949,.F.);
#18438=ORIENTED_EDGE('',*,*,#14001,.T.);
#18439=ORIENTED_EDGE('',*,*,#13998,.F.);
#18440=ORIENTED_EDGE('',*,*,#13975,.F.);
#18441=ORIENTED_EDGE('',*,*,#13915,.F.);
#18442=ORIENTED_EDGE('',*,*,#14239,.F.);
#18443=ORIENTED_EDGE('',*,*,#14002,.T.);
#18444=ORIENTED_EDGE('',*,*,#14240,.T.);
#18445=ORIENTED_EDGE('',*,*,#13934,.F.);
#18446=ORIENTED_EDGE('',*,*,#14241,.F.);
#18447=ORIENTED_EDGE('',*,*,#14003,.T.);
#18448=ORIENTED_EDGE('',*,*,#14239,.T.);
#18449=ORIENTED_EDGE('',*,*,#13921,.F.);
#18450=ORIENTED_EDGE('',*,*,#14242,.F.);
#18451=ORIENTED_EDGE('',*,*,#14004,.T.);
#18452=ORIENTED_EDGE('',*,*,#14241,.T.);
#18453=ORIENTED_EDGE('',*,*,#13920,.F.);
#18454=ORIENTED_EDGE('',*,*,#14243,.F.);
#18455=ORIENTED_EDGE('',*,*,#14005,.T.);
#18456=ORIENTED_EDGE('',*,*,#14242,.T.);
#18457=ORIENTED_EDGE('',*,*,#13919,.F.);
#18458=ORIENTED_EDGE('',*,*,#14244,.F.);
#18459=ORIENTED_EDGE('',*,*,#14006,.T.);
#18460=ORIENTED_EDGE('',*,*,#14243,.T.);
#18461=ORIENTED_EDGE('',*,*,#13918,.F.);
#18462=ORIENTED_EDGE('',*,*,#14245,.F.);
#18463=ORIENTED_EDGE('',*,*,#14007,.T.);
#18464=ORIENTED_EDGE('',*,*,#14244,.T.);
#18465=ORIENTED_EDGE('',*,*,#13917,.F.);
#18466=ORIENTED_EDGE('',*,*,#14246,.F.);
#18467=ORIENTED_EDGE('',*,*,#14008,.T.);
#18468=ORIENTED_EDGE('',*,*,#14245,.T.);
#18469=ORIENTED_EDGE('',*,*,#13916,.F.);
#18470=ORIENTED_EDGE('',*,*,#14240,.F.);
#18471=ORIENTED_EDGE('',*,*,#14009,.T.);
#18472=ORIENTED_EDGE('',*,*,#14246,.T.);
#18473=ORIENTED_EDGE('',*,*,#14247,.T.);
#18474=ORIENTED_EDGE('',*,*,#14248,.F.);
#18475=ORIENTED_EDGE('',*,*,#14205,.F.);
#18476=ORIENTED_EDGE('',*,*,#14124,.F.);
#18477=ORIENTED_EDGE('',*,*,#14149,.F.);
#18478=ORIENTED_EDGE('',*,*,#13912,.F.);
#18479=ORIENTED_EDGE('',*,*,#13905,.F.);
#18480=ORIENTED_EDGE('',*,*,#14132,.F.);
#18481=ORIENTED_EDGE('',*,*,#14194,.T.);
#18482=ORIENTED_EDGE('',*,*,#14168,.F.);
#18483=ORIENTED_EDGE('',*,*,#14249,.F.);
#18484=ORIENTED_EDGE('',*,*,#14247,.F.);
#18485=ORIENTED_EDGE('',*,*,#13911,.T.);
#18486=ORIENTED_EDGE('',*,*,#14114,.F.);
#18487=ORIENTED_EDGE('',*,*,#14206,.F.);
#18488=ORIENTED_EDGE('',*,*,#14248,.T.);
#18489=ORIENTED_EDGE('',*,*,#14249,.T.);
#18490=ORIENTED_EDGE('',*,*,#14165,.F.);
#18491=ORIENTED_EDGE('',*,*,#14126,.F.);
#18492=ORIENTED_EDGE('',*,*,#14250,.T.);
#18493=ORIENTED_EDGE('',*,*,#14251,.F.);
#18494=ORIENTED_EDGE('',*,*,#14252,.T.);
#18495=ORIENTED_EDGE('',*,*,#14253,.T.);
#18496=ORIENTED_EDGE('',*,*,#14251,.T.);
#18497=ORIENTED_EDGE('',*,*,#14254,.T.);
#18498=ORIENTED_EDGE('',*,*,#14255,.T.);
#18499=ORIENTED_EDGE('',*,*,#14256,.T.);
#18500=ORIENTED_EDGE('',*,*,#14257,.T.);
#18501=ORIENTED_EDGE('',*,*,#14258,.T.);
#18502=ORIENTED_EDGE('',*,*,#14255,.F.);
#18503=ORIENTED_EDGE('',*,*,#14259,.T.);
#18504=ORIENTED_EDGE('',*,*,#14253,.F.);
#18505=ORIENTED_EDGE('',*,*,#14260,.F.);
#18506=ORIENTED_EDGE('',*,*,#14261,.F.);
#18507=ORIENTED_EDGE('',*,*,#14262,.F.);
#18508=ORIENTED_EDGE('',*,*,#14263,.F.);
#18509=ORIENTED_EDGE('',*,*,#14264,.F.);
#18510=ORIENTED_EDGE('',*,*,#14265,.F.);
#18511=ORIENTED_EDGE('',*,*,#14252,.F.);
#18512=ORIENTED_EDGE('',*,*,#14256,.F.);
#18513=ORIENTED_EDGE('',*,*,#14266,.T.);
#18514=ORIENTED_EDGE('',*,*,#14267,.F.);
#18515=ORIENTED_EDGE('',*,*,#14268,.F.);
#18516=ORIENTED_EDGE('',*,*,#14260,.T.);
#18517=ORIENTED_EDGE('',*,*,#14258,.F.);
#18518=ORIENTED_EDGE('',*,*,#14269,.F.);
#18519=ORIENTED_EDGE('',*,*,#14270,.F.);
#18520=ORIENTED_EDGE('',*,*,#14266,.F.);
#18521=ORIENTED_EDGE('',*,*,#14268,.T.);
#18522=ORIENTED_EDGE('',*,*,#14271,.F.);
#18523=ORIENTED_EDGE('',*,*,#14272,.T.);
#18524=ORIENTED_EDGE('',*,*,#14261,.T.);
#18525=ORIENTED_EDGE('',*,*,#14271,.T.);
#18526=ORIENTED_EDGE('',*,*,#14267,.T.);
#18527=ORIENTED_EDGE('',*,*,#14273,.T.);
#18528=ORIENTED_EDGE('',*,*,#14274,.T.);
#18529=ORIENTED_EDGE('',*,*,#14275,.T.);
#18530=ORIENTED_EDGE('',*,*,#14276,.T.);
#18531=ORIENTED_EDGE('',*,*,#14273,.F.);
#18532=ORIENTED_EDGE('',*,*,#14270,.T.);
#18533=ORIENTED_EDGE('',*,*,#14272,.F.);
#18534=ORIENTED_EDGE('',*,*,#14274,.F.);
#18535=ORIENTED_EDGE('',*,*,#14277,.T.);
#18536=ORIENTED_EDGE('',*,*,#14278,.T.);
#18537=ORIENTED_EDGE('',*,*,#14262,.T.);
#18538=ORIENTED_EDGE('',*,*,#14276,.F.);
#18539=ORIENTED_EDGE('',*,*,#14279,.F.);
#18540=ORIENTED_EDGE('',*,*,#14280,.F.);
#18541=ORIENTED_EDGE('',*,*,#14277,.F.);
#18542=ORIENTED_EDGE('',*,*,#14281,.T.);
#18543=ORIENTED_EDGE('',*,*,#14282,.F.);
#18544=ORIENTED_EDGE('',*,*,#14283,.T.);
#18545=ORIENTED_EDGE('',*,*,#14284,.T.);
#18546=ORIENTED_EDGE('',*,*,#14282,.T.);
#18547=ORIENTED_EDGE('',*,*,#14285,.T.);
#18548=ORIENTED_EDGE('',*,*,#14286,.T.);
#18549=ORIENTED_EDGE('',*,*,#14287,.T.);
#18550=ORIENTED_EDGE('',*,*,#14288,.T.);
#18551=ORIENTED_EDGE('',*,*,#14289,.T.);
#18552=ORIENTED_EDGE('',*,*,#14286,.F.);
#18553=ORIENTED_EDGE('',*,*,#14290,.T.);
#18554=ORIENTED_EDGE('',*,*,#14284,.F.);
#18555=ORIENTED_EDGE('',*,*,#14291,.F.);
#18556=ORIENTED_EDGE('',*,*,#14292,.F.);
#18557=ORIENTED_EDGE('',*,*,#14293,.F.);
#18558=ORIENTED_EDGE('',*,*,#14294,.F.);
#18559=ORIENTED_EDGE('',*,*,#14283,.F.);
#18560=ORIENTED_EDGE('',*,*,#14287,.F.);
#18561=ORIENTED_EDGE('',*,*,#14295,.T.);
#18562=ORIENTED_EDGE('',*,*,#14296,.T.);
#18563=ORIENTED_EDGE('',*,*,#14291,.T.);
#18564=ORIENTED_EDGE('',*,*,#14289,.F.);
#18565=ORIENTED_EDGE('',*,*,#14297,.F.);
#18566=ORIENTED_EDGE('',*,*,#14298,.F.);
#18567=ORIENTED_EDGE('',*,*,#14295,.F.);
#18568=ORIENTED_EDGE('',*,*,#14299,.T.);
#18569=ORIENTED_EDGE('',*,*,#14300,.F.);
#18570=ORIENTED_EDGE('',*,*,#14301,.T.);
#18571=ORIENTED_EDGE('',*,*,#14302,.T.);
#18572=ORIENTED_EDGE('',*,*,#14300,.T.);
#18573=ORIENTED_EDGE('',*,*,#14303,.T.);
#18574=ORIENTED_EDGE('',*,*,#14304,.T.);
#18575=ORIENTED_EDGE('',*,*,#14305,.T.);
#18576=ORIENTED_EDGE('',*,*,#14306,.T.);
#18577=ORIENTED_EDGE('',*,*,#14307,.T.);
#18578=ORIENTED_EDGE('',*,*,#14304,.F.);
#18579=ORIENTED_EDGE('',*,*,#14308,.T.);
#18580=ORIENTED_EDGE('',*,*,#14302,.F.);
#18581=ORIENTED_EDGE('',*,*,#14309,.F.);
#18582=ORIENTED_EDGE('',*,*,#14310,.F.);
#18583=ORIENTED_EDGE('',*,*,#14311,.F.);
#18584=ORIENTED_EDGE('',*,*,#14312,.F.);
#18585=ORIENTED_EDGE('',*,*,#14313,.F.);
#18586=ORIENTED_EDGE('',*,*,#14301,.F.);
#18587=ORIENTED_EDGE('',*,*,#14305,.F.);
#18588=ORIENTED_EDGE('',*,*,#14314,.T.);
#18589=ORIENTED_EDGE('',*,*,#14315,.F.);
#18590=ORIENTED_EDGE('',*,*,#14316,.F.);
#18591=ORIENTED_EDGE('',*,*,#14309,.T.);
#18592=ORIENTED_EDGE('',*,*,#14307,.F.);
#18593=ORIENTED_EDGE('',*,*,#14317,.F.);
#18594=ORIENTED_EDGE('',*,*,#14318,.F.);
#18595=ORIENTED_EDGE('',*,*,#14314,.F.);
#18596=ORIENTED_EDGE('',*,*,#14316,.T.);
#18597=ORIENTED_EDGE('',*,*,#14319,.F.);
#18598=ORIENTED_EDGE('',*,*,#14320,.T.);
#18599=ORIENTED_EDGE('',*,*,#14310,.T.);
#18600=ORIENTED_EDGE('',*,*,#14319,.T.);
#18601=ORIENTED_EDGE('',*,*,#14315,.T.);
#18602=ORIENTED_EDGE('',*,*,#14321,.T.);
#18603=ORIENTED_EDGE('',*,*,#14322,.T.);
#18604=ORIENTED_EDGE('',*,*,#14323,.T.);
#18605=ORIENTED_EDGE('',*,*,#14324,.T.);
#18606=ORIENTED_EDGE('',*,*,#14321,.F.);
#18607=ORIENTED_EDGE('',*,*,#14318,.T.);
#18608=ORIENTED_EDGE('',*,*,#14320,.F.);
#18609=ORIENTED_EDGE('',*,*,#14322,.F.);
#18610=ORIENTED_EDGE('',*,*,#14325,.T.);
#18611=ORIENTED_EDGE('',*,*,#14326,.T.);
#18612=ORIENTED_EDGE('',*,*,#14311,.T.);
#18613=ORIENTED_EDGE('',*,*,#14324,.F.);
#18614=ORIENTED_EDGE('',*,*,#14327,.F.);
#18615=ORIENTED_EDGE('',*,*,#14328,.F.);
#18616=ORIENTED_EDGE('',*,*,#14325,.F.);
#18617=ORIENTED_EDGE('',*,*,#14329,.T.);
#18618=ORIENTED_EDGE('',*,*,#14330,.F.);
#18619=ORIENTED_EDGE('',*,*,#14331,.T.);
#18620=ORIENTED_EDGE('',*,*,#14332,.T.);
#18621=ORIENTED_EDGE('',*,*,#14330,.T.);
#18622=ORIENTED_EDGE('',*,*,#14333,.T.);
#18623=ORIENTED_EDGE('',*,*,#14334,.T.);
#18624=ORIENTED_EDGE('',*,*,#14335,.T.);
#18625=ORIENTED_EDGE('',*,*,#14336,.T.);
#18626=ORIENTED_EDGE('',*,*,#14337,.T.);
#18627=ORIENTED_EDGE('',*,*,#14334,.F.);
#18628=ORIENTED_EDGE('',*,*,#14338,.T.);
#18629=ORIENTED_EDGE('',*,*,#14332,.F.);
#18630=ORIENTED_EDGE('',*,*,#14339,.F.);
#18631=ORIENTED_EDGE('',*,*,#14340,.F.);
#18632=ORIENTED_EDGE('',*,*,#14341,.F.);
#18633=ORIENTED_EDGE('',*,*,#14342,.F.);
#18634=ORIENTED_EDGE('',*,*,#14343,.F.);
#18635=ORIENTED_EDGE('',*,*,#14331,.F.);
#18636=ORIENTED_EDGE('',*,*,#14335,.F.);
#18637=ORIENTED_EDGE('',*,*,#14344,.T.);
#18638=ORIENTED_EDGE('',*,*,#14345,.F.);
#18639=ORIENTED_EDGE('',*,*,#14346,.F.);
#18640=ORIENTED_EDGE('',*,*,#14339,.T.);
#18641=ORIENTED_EDGE('',*,*,#14337,.F.);
#18642=ORIENTED_EDGE('',*,*,#14347,.F.);
#18643=ORIENTED_EDGE('',*,*,#14348,.F.);
#18644=ORIENTED_EDGE('',*,*,#14344,.F.);
#18645=ORIENTED_EDGE('',*,*,#14346,.T.);
#18646=ORIENTED_EDGE('',*,*,#14349,.F.);
#18647=ORIENTED_EDGE('',*,*,#14350,.T.);
#18648=ORIENTED_EDGE('',*,*,#14340,.T.);
#18649=ORIENTED_EDGE('',*,*,#14349,.T.);
#18650=ORIENTED_EDGE('',*,*,#14345,.T.);
#18651=ORIENTED_EDGE('',*,*,#14351,.T.);
#18652=ORIENTED_EDGE('',*,*,#14352,.T.);
#18653=ORIENTED_EDGE('',*,*,#14353,.T.);
#18654=ORIENTED_EDGE('',*,*,#14354,.T.);
#18655=ORIENTED_EDGE('',*,*,#14351,.F.);
#18656=ORIENTED_EDGE('',*,*,#14348,.T.);
#18657=ORIENTED_EDGE('',*,*,#14350,.F.);
#18658=ORIENTED_EDGE('',*,*,#14352,.F.);
#18659=ORIENTED_EDGE('',*,*,#14355,.T.);
#18660=ORIENTED_EDGE('',*,*,#14356,.T.);
#18661=ORIENTED_EDGE('',*,*,#14341,.T.);
#18662=ORIENTED_EDGE('',*,*,#14354,.F.);
#18663=ORIENTED_EDGE('',*,*,#14357,.F.);
#18664=ORIENTED_EDGE('',*,*,#14358,.F.);
#18665=ORIENTED_EDGE('',*,*,#14355,.F.);
#18666=ORIENTED_EDGE('',*,*,#14359,.T.);
#18667=ORIENTED_EDGE('',*,*,#14360,.T.);
#18668=ORIENTED_EDGE('',*,*,#14361,.T.);
#18669=ORIENTED_EDGE('',*,*,#14360,.F.);
#18670=ORIENTED_EDGE('',*,*,#14361,.F.);
#18671=ORIENTED_EDGE('',*,*,#14362,.T.);
#18672=ORIENTED_EDGE('',*,*,#14363,.F.);
#18673=ORIENTED_EDGE('',*,*,#14362,.F.);
#18674=ORIENTED_EDGE('',*,*,#14364,.F.);
#18675=ORIENTED_EDGE('',*,*,#14365,.T.);
#18676=ORIENTED_EDGE('',*,*,#14359,.F.);
#18677=ORIENTED_EDGE('',*,*,#14365,.F.);
#18678=ORIENTED_EDGE('',*,*,#14363,.T.);
#18679=ORIENTED_EDGE('',*,*,#14366,.T.);
#18680=ORIENTED_EDGE('',*,*,#14367,.T.);
#18681=ORIENTED_EDGE('',*,*,#14366,.F.);
#18682=ORIENTED_EDGE('',*,*,#14367,.F.);
#18683=ORIENTED_EDGE('',*,*,#14368,.T.);
#18684=ORIENTED_EDGE('',*,*,#14369,.T.);
#18685=ORIENTED_EDGE('',*,*,#14370,.T.);
#18686=ORIENTED_EDGE('',*,*,#14371,.T.);
#18687=ORIENTED_EDGE('',*,*,#14372,.T.);
#18688=ORIENTED_EDGE('',*,*,#14373,.T.);
#18689=ORIENTED_EDGE('',*,*,#14374,.T.);
#18690=ORIENTED_EDGE('',*,*,#14375,.T.);
#18691=ORIENTED_EDGE('',*,*,#14376,.T.);
#18692=ORIENTED_EDGE('',*,*,#14377,.T.);
#18693=ORIENTED_EDGE('',*,*,#14378,.T.);
#18694=ORIENTED_EDGE('',*,*,#14379,.F.);
#18695=ORIENTED_EDGE('',*,*,#14297,.T.);
#18696=ORIENTED_EDGE('',*,*,#14288,.F.);
#18697=ORIENTED_EDGE('',*,*,#14380,.T.);
#18698=ORIENTED_EDGE('',*,*,#14381,.T.);
#18699=ORIENTED_EDGE('',*,*,#14327,.T.);
#18700=ORIENTED_EDGE('',*,*,#14323,.F.);
#18701=ORIENTED_EDGE('',*,*,#14317,.T.);
#18702=ORIENTED_EDGE('',*,*,#14306,.F.);
#18703=ORIENTED_EDGE('',*,*,#14382,.T.);
#18704=ORIENTED_EDGE('',*,*,#14383,.T.);
#18705=ORIENTED_EDGE('',*,*,#14357,.T.);
#18706=ORIENTED_EDGE('',*,*,#14353,.F.);
#18707=ORIENTED_EDGE('',*,*,#14347,.T.);
#18708=ORIENTED_EDGE('',*,*,#14336,.F.);
#18709=ORIENTED_EDGE('',*,*,#14384,.T.);
#18710=ORIENTED_EDGE('',*,*,#14385,.T.);
#18711=ORIENTED_EDGE('',*,*,#14279,.T.);
#18712=ORIENTED_EDGE('',*,*,#14275,.F.);
#18713=ORIENTED_EDGE('',*,*,#14269,.T.);
#18714=ORIENTED_EDGE('',*,*,#14257,.F.);
#18715=ORIENTED_EDGE('',*,*,#14329,.F.);
#18716=ORIENTED_EDGE('',*,*,#14343,.T.);
#18717=ORIENTED_EDGE('',*,*,#14386,.T.);
#18718=ORIENTED_EDGE('',*,*,#14387,.T.);
#18719=ORIENTED_EDGE('',*,*,#14333,.F.);
#18720=ORIENTED_EDGE('',*,*,#14338,.F.);
#18721=ORIENTED_EDGE('',*,*,#14387,.F.);
#18722=ORIENTED_EDGE('',*,*,#14388,.F.);
#18723=ORIENTED_EDGE('',*,*,#14384,.F.);
#18724=ORIENTED_EDGE('',*,*,#14299,.F.);
#18725=ORIENTED_EDGE('',*,*,#14313,.T.);
#18726=ORIENTED_EDGE('',*,*,#14389,.T.);
#18727=ORIENTED_EDGE('',*,*,#14390,.T.);
#18728=ORIENTED_EDGE('',*,*,#14303,.F.);
#18729=ORIENTED_EDGE('',*,*,#14308,.F.);
#18730=ORIENTED_EDGE('',*,*,#14390,.F.);
#18731=ORIENTED_EDGE('',*,*,#14391,.F.);
#18732=ORIENTED_EDGE('',*,*,#14382,.F.);
#18733=ORIENTED_EDGE('',*,*,#14392,.T.);
#18734=ORIENTED_EDGE('',*,*,#14393,.T.);
#18735=ORIENTED_EDGE('',*,*,#14364,.T.);
#18736=ORIENTED_EDGE('',*,*,#14393,.F.);
#18737=ORIENTED_EDGE('',*,*,#14392,.F.);
#18738=ORIENTED_EDGE('',*,*,#14394,.F.);
#18739=ORIENTED_EDGE('',*,*,#14395,.T.);
#18740=ORIENTED_EDGE('',*,*,#14396,.T.);
#18741=ORIENTED_EDGE('',*,*,#14397,.F.);
#18742=ORIENTED_EDGE('',*,*,#14398,.T.);
#18743=ORIENTED_EDGE('',*,*,#14399,.T.);
#18744=ORIENTED_EDGE('',*,*,#14400,.F.);
#18745=ORIENTED_EDGE('',*,*,#14401,.T.);
#18746=ORIENTED_EDGE('',*,*,#14402,.T.);
#18747=ORIENTED_EDGE('',*,*,#14403,.F.);
#18748=ORIENTED_EDGE('',*,*,#14404,.T.);
#18749=ORIENTED_EDGE('',*,*,#14405,.T.);
#18750=ORIENTED_EDGE('',*,*,#14406,.F.);
#18751=ORIENTED_EDGE('',*,*,#14407,.T.);
#18752=ORIENTED_EDGE('',*,*,#14408,.T.);
#18753=ORIENTED_EDGE('',*,*,#14409,.F.);
#18754=ORIENTED_EDGE('',*,*,#14410,.T.);
#18755=ORIENTED_EDGE('',*,*,#14411,.T.);
#18756=ORIENTED_EDGE('',*,*,#14412,.F.);
#18757=ORIENTED_EDGE('',*,*,#14413,.F.);
#18758=ORIENTED_EDGE('',*,*,#14414,.T.);
#18759=ORIENTED_EDGE('',*,*,#14415,.T.);
#18760=ORIENTED_EDGE('',*,*,#14416,.F.);
#18761=ORIENTED_EDGE('',*,*,#14417,.T.);
#18762=ORIENTED_EDGE('',*,*,#14418,.T.);
#18763=ORIENTED_EDGE('',*,*,#14419,.T.);
#18764=ORIENTED_EDGE('',*,*,#14420,.T.);
#18765=ORIENTED_EDGE('',*,*,#14421,.T.);
#18766=ORIENTED_EDGE('',*,*,#14420,.F.);
#18767=ORIENTED_EDGE('',*,*,#14422,.F.);
#18768=ORIENTED_EDGE('',*,*,#14423,.T.);
#18769=ORIENTED_EDGE('',*,*,#14419,.F.);
#18770=ORIENTED_EDGE('',*,*,#14423,.F.);
#18771=ORIENTED_EDGE('',*,*,#14421,.F.);
#18772=ORIENTED_EDGE('',*,*,#14424,.T.);
#18773=ORIENTED_EDGE('',*,*,#14425,.T.);
#18774=ORIENTED_EDGE('',*,*,#14426,.T.);
#18775=ORIENTED_EDGE('',*,*,#14427,.T.);
#18776=ORIENTED_EDGE('',*,*,#14428,.T.);
#18777=ORIENTED_EDGE('',*,*,#14429,.T.);
#18778=ORIENTED_EDGE('',*,*,#14430,.T.);
#18779=ORIENTED_EDGE('',*,*,#14431,.T.);
#18780=ORIENTED_EDGE('',*,*,#14432,.T.);
#18781=ORIENTED_EDGE('',*,*,#14433,.T.);
#18782=ORIENTED_EDGE('',*,*,#14434,.T.);
#18783=ORIENTED_EDGE('',*,*,#14435,.T.);
#18784=ORIENTED_EDGE('',*,*,#14436,.T.);
#18785=ORIENTED_EDGE('',*,*,#14437,.T.);
#18786=ORIENTED_EDGE('',*,*,#14438,.T.);
#18787=ORIENTED_EDGE('',*,*,#14439,.T.);
#18788=ORIENTED_EDGE('',*,*,#14440,.T.);
#18789=ORIENTED_EDGE('',*,*,#14441,.T.);
#18790=ORIENTED_EDGE('',*,*,#14442,.T.);
#18791=ORIENTED_EDGE('',*,*,#14443,.T.);
#18792=ORIENTED_EDGE('',*,*,#14444,.T.);
#18793=ORIENTED_EDGE('',*,*,#14445,.T.);
#18794=ORIENTED_EDGE('',*,*,#14446,.T.);
#18795=ORIENTED_EDGE('',*,*,#14447,.T.);
#18796=ORIENTED_EDGE('',*,*,#14448,.T.);
#18797=ORIENTED_EDGE('',*,*,#14449,.T.);
#18798=ORIENTED_EDGE('',*,*,#14450,.T.);
#18799=ORIENTED_EDGE('',*,*,#14451,.T.);
#18800=ORIENTED_EDGE('',*,*,#14452,.T.);
#18801=ORIENTED_EDGE('',*,*,#14453,.T.);
#18802=ORIENTED_EDGE('',*,*,#14454,.T.);
#18803=ORIENTED_EDGE('',*,*,#14455,.T.);
#18804=ORIENTED_EDGE('',*,*,#14456,.T.);
#18805=ORIENTED_EDGE('',*,*,#14457,.T.);
#18806=ORIENTED_EDGE('',*,*,#14458,.T.);
#18807=ORIENTED_EDGE('',*,*,#14459,.T.);
#18808=ORIENTED_EDGE('',*,*,#14460,.T.);
#18809=ORIENTED_EDGE('',*,*,#14461,.T.);
#18810=ORIENTED_EDGE('',*,*,#14462,.T.);
#18811=ORIENTED_EDGE('',*,*,#14463,.T.);
#18812=ORIENTED_EDGE('',*,*,#14464,.T.);
#18813=ORIENTED_EDGE('',*,*,#14465,.T.);
#18814=ORIENTED_EDGE('',*,*,#14466,.T.);
#18815=ORIENTED_EDGE('',*,*,#14467,.T.);
#18816=ORIENTED_EDGE('',*,*,#14468,.T.);
#18817=ORIENTED_EDGE('',*,*,#14469,.T.);
#18818=ORIENTED_EDGE('',*,*,#14470,.T.);
#18819=ORIENTED_EDGE('',*,*,#14471,.T.);
#18820=ORIENTED_EDGE('',*,*,#14472,.T.);
#18821=ORIENTED_EDGE('',*,*,#14473,.T.);
#18822=ORIENTED_EDGE('',*,*,#14474,.T.);
#18823=ORIENTED_EDGE('',*,*,#14475,.T.);
#18824=ORIENTED_EDGE('',*,*,#14476,.T.);
#18825=ORIENTED_EDGE('',*,*,#14477,.T.);
#18826=ORIENTED_EDGE('',*,*,#14478,.T.);
#18827=ORIENTED_EDGE('',*,*,#14479,.T.);
#18828=ORIENTED_EDGE('',*,*,#14480,.F.);
#18829=ORIENTED_EDGE('',*,*,#14481,.F.);
#18830=ORIENTED_EDGE('',*,*,#14482,.T.);
#18831=ORIENTED_EDGE('',*,*,#14483,.T.);
#18832=ORIENTED_EDGE('',*,*,#14484,.T.);
#18833=ORIENTED_EDGE('',*,*,#14485,.T.);
#18834=ORIENTED_EDGE('',*,*,#14486,.T.);
#18835=ORIENTED_EDGE('',*,*,#14487,.T.);
#18836=ORIENTED_EDGE('',*,*,#14488,.T.);
#18837=ORIENTED_EDGE('',*,*,#14489,.T.);
#18838=ORIENTED_EDGE('',*,*,#14490,.T.);
#18839=ORIENTED_EDGE('',*,*,#14491,.T.);
#18840=ORIENTED_EDGE('',*,*,#14492,.T.);
#18841=ORIENTED_EDGE('',*,*,#14493,.T.);
#18842=ORIENTED_EDGE('',*,*,#14494,.F.);
#18843=ORIENTED_EDGE('',*,*,#14495,.F.);
#18844=ORIENTED_EDGE('',*,*,#14496,.T.);
#18845=ORIENTED_EDGE('',*,*,#14497,.T.);
#18846=ORIENTED_EDGE('',*,*,#14498,.T.);
#18847=ORIENTED_EDGE('',*,*,#14499,.T.);
#18848=ORIENTED_EDGE('',*,*,#14500,.T.);
#18849=ORIENTED_EDGE('',*,*,#14501,.T.);
#18850=ORIENTED_EDGE('',*,*,#14502,.T.);
#18851=ORIENTED_EDGE('',*,*,#14503,.T.);
#18852=ORIENTED_EDGE('',*,*,#14504,.T.);
#18853=ORIENTED_EDGE('',*,*,#14505,.F.);
#18854=ORIENTED_EDGE('',*,*,#14506,.F.);
#18855=ORIENTED_EDGE('',*,*,#14507,.F.);
#18856=ORIENTED_EDGE('',*,*,#14508,.T.);
#18857=ORIENTED_EDGE('',*,*,#14509,.T.);
#18858=ORIENTED_EDGE('',*,*,#14510,.T.);
#18859=ORIENTED_EDGE('',*,*,#14511,.T.);
#18860=ORIENTED_EDGE('',*,*,#14512,.T.);
#18861=ORIENTED_EDGE('',*,*,#14513,.T.);
#18862=ORIENTED_EDGE('',*,*,#14514,.T.);
#18863=ORIENTED_EDGE('',*,*,#14515,.T.);
#18864=ORIENTED_EDGE('',*,*,#14516,.T.);
#18865=ORIENTED_EDGE('',*,*,#14517,.T.);
#18866=ORIENTED_EDGE('',*,*,#14518,.T.);
#18867=ORIENTED_EDGE('',*,*,#14519,.T.);
#18868=ORIENTED_EDGE('',*,*,#14520,.F.);
#18869=ORIENTED_EDGE('',*,*,#14521,.F.);
#18870=ORIENTED_EDGE('',*,*,#14281,.F.);
#18871=ORIENTED_EDGE('',*,*,#14294,.T.);
#18872=ORIENTED_EDGE('',*,*,#14522,.T.);
#18873=ORIENTED_EDGE('',*,*,#14523,.T.);
#18874=ORIENTED_EDGE('',*,*,#14285,.F.);
#18875=ORIENTED_EDGE('',*,*,#14524,.T.);
#18876=ORIENTED_EDGE('',*,*,#14298,.T.);
#18877=ORIENTED_EDGE('',*,*,#14379,.T.);
#18878=ORIENTED_EDGE('',*,*,#14525,.T.);
#18879=ORIENTED_EDGE('',*,*,#14524,.F.);
#18880=ORIENTED_EDGE('',*,*,#14526,.T.);
#18881=ORIENTED_EDGE('',*,*,#14296,.F.);
#18882=ORIENTED_EDGE('',*,*,#14526,.F.);
#18883=ORIENTED_EDGE('',*,*,#14527,.T.);
#18884=ORIENTED_EDGE('',*,*,#14528,.T.);
#18885=ORIENTED_EDGE('',*,*,#14292,.T.);
#18886=ORIENTED_EDGE('',*,*,#14525,.F.);
#18887=ORIENTED_EDGE('',*,*,#14378,.F.);
#18888=ORIENTED_EDGE('',*,*,#14529,.F.);
#18889=ORIENTED_EDGE('',*,*,#14527,.F.);
#18890=ORIENTED_EDGE('',*,*,#14530,.T.);
#18891=ORIENTED_EDGE('',*,*,#14531,.T.);
#18892=ORIENTED_EDGE('',*,*,#14422,.T.);
#18893=ORIENTED_EDGE('',*,*,#14531,.F.);
#18894=ORIENTED_EDGE('',*,*,#14532,.T.);
#18895=ORIENTED_EDGE('',*,*,#14533,.F.);
#18896=ORIENTED_EDGE('',*,*,#14264,.T.);
#18897=ORIENTED_EDGE('',*,*,#14534,.T.);
#18898=ORIENTED_EDGE('',*,*,#14530,.F.);
#18899=ORIENTED_EDGE('',*,*,#14534,.F.);
#18900=ORIENTED_EDGE('',*,*,#14263,.T.);
#18901=ORIENTED_EDGE('',*,*,#14278,.F.);
#18902=ORIENTED_EDGE('',*,*,#14280,.T.);
#18903=ORIENTED_EDGE('',*,*,#14385,.F.);
#18904=ORIENTED_EDGE('',*,*,#14388,.T.);
#18905=ORIENTED_EDGE('',*,*,#14386,.F.);
#18906=ORIENTED_EDGE('',*,*,#14342,.T.);
#18907=ORIENTED_EDGE('',*,*,#14356,.F.);
#18908=ORIENTED_EDGE('',*,*,#14358,.T.);
#18909=ORIENTED_EDGE('',*,*,#14383,.F.);
#18910=ORIENTED_EDGE('',*,*,#14391,.T.);
#18911=ORIENTED_EDGE('',*,*,#14389,.F.);
#18912=ORIENTED_EDGE('',*,*,#14312,.T.);
#18913=ORIENTED_EDGE('',*,*,#14326,.F.);
#18914=ORIENTED_EDGE('',*,*,#14328,.T.);
#18915=ORIENTED_EDGE('',*,*,#14381,.F.);
#18916=ORIENTED_EDGE('',*,*,#14535,.T.);
#18917=ORIENTED_EDGE('',*,*,#14522,.F.);
#18918=ORIENTED_EDGE('',*,*,#14293,.T.);
#18919=ORIENTED_EDGE('',*,*,#14528,.F.);
#18920=ORIENTED_EDGE('',*,*,#14529,.T.);
#18921=ORIENTED_EDGE('',*,*,#14377,.F.);
#18922=ORIENTED_EDGE('',*,*,#14250,.F.);
#18923=ORIENTED_EDGE('',*,*,#14265,.T.);
#18924=ORIENTED_EDGE('',*,*,#14533,.T.);
#18925=ORIENTED_EDGE('',*,*,#14536,.T.);
#18926=ORIENTED_EDGE('',*,*,#14254,.F.);
#18927=ORIENTED_EDGE('',*,*,#14259,.F.);
#18928=ORIENTED_EDGE('',*,*,#14536,.F.);
#18929=ORIENTED_EDGE('',*,*,#14532,.F.);
#18930=ORIENTED_EDGE('',*,*,#14376,.F.);
#18931=ORIENTED_EDGE('',*,*,#14537,.T.);
#18932=ORIENTED_EDGE('',*,*,#14538,.T.);
#18933=ORIENTED_EDGE('',*,*,#14539,.T.);
#18934=ORIENTED_EDGE('',*,*,#14540,.T.);
#18935=ORIENTED_EDGE('',*,*,#14541,.T.);
#18936=ORIENTED_EDGE('',*,*,#14542,.T.);
#18937=ORIENTED_EDGE('',*,*,#14543,.T.);
#18938=ORIENTED_EDGE('',*,*,#14538,.F.);
#18939=ORIENTED_EDGE('',*,*,#14544,.T.);
#18940=ORIENTED_EDGE('',*,*,#14545,.T.);
#18941=ORIENTED_EDGE('',*,*,#14546,.T.);
#18942=ORIENTED_EDGE('',*,*,#14540,.F.);
#18943=ORIENTED_EDGE('',*,*,#14541,.F.);
#18944=ORIENTED_EDGE('',*,*,#14537,.F.);
#18945=ORIENTED_EDGE('',*,*,#14546,.F.);
#18946=ORIENTED_EDGE('',*,*,#14547,.T.);
#18947=ORIENTED_EDGE('',*,*,#14548,.T.);
#18948=ORIENTED_EDGE('',*,*,#14549,.T.);
#18949=ORIENTED_EDGE('',*,*,#14550,.T.);
#18950=ORIENTED_EDGE('',*,*,#14551,.T.);
#18951=ORIENTED_EDGE('',*,*,#14550,.F.);
#18952=ORIENTED_EDGE('',*,*,#14545,.F.);
#18953=ORIENTED_EDGE('',*,*,#14552,.T.);
#18954=ORIENTED_EDGE('',*,*,#14553,.T.);
#18955=ORIENTED_EDGE('',*,*,#14554,.T.);
#18956=ORIENTED_EDGE('',*,*,#14548,.F.);
#18957=ORIENTED_EDGE('',*,*,#14549,.F.);
#18958=ORIENTED_EDGE('',*,*,#14554,.F.);
#18959=ORIENTED_EDGE('',*,*,#14555,.T.);
#18960=ORIENTED_EDGE('',*,*,#14556,.F.);
#18961=ORIENTED_EDGE('',*,*,#14542,.F.);
#18962=ORIENTED_EDGE('',*,*,#14547,.F.);
#18963=ORIENTED_EDGE('',*,*,#14557,.T.);
#18964=ORIENTED_EDGE('',*,*,#14400,.T.);
#18965=ORIENTED_EDGE('',*,*,#14558,.T.);
#18966=ORIENTED_EDGE('',*,*,#14397,.T.);
#18967=ORIENTED_EDGE('',*,*,#14559,.T.);
#18968=ORIENTED_EDGE('',*,*,#14394,.T.);
#18969=ORIENTED_EDGE('',*,*,#14560,.T.);
#18970=ORIENTED_EDGE('',*,*,#14416,.T.);
#18971=ORIENTED_EDGE('',*,*,#14561,.T.);
#18972=ORIENTED_EDGE('',*,*,#14413,.T.);
#18973=ORIENTED_EDGE('',*,*,#14562,.T.);
#18974=ORIENTED_EDGE('',*,*,#14563,.T.);
#18975=ORIENTED_EDGE('',*,*,#14564,.T.);
#18976=ORIENTED_EDGE('',*,*,#14562,.F.);
#18977=ORIENTED_EDGE('',*,*,#14412,.T.);
#18978=ORIENTED_EDGE('',*,*,#14565,.T.);
#18979=ORIENTED_EDGE('',*,*,#14409,.T.);
#18980=ORIENTED_EDGE('',*,*,#14566,.T.);
#18981=ORIENTED_EDGE('',*,*,#14406,.T.);
#18982=ORIENTED_EDGE('',*,*,#14567,.T.);
#18983=ORIENTED_EDGE('',*,*,#14403,.T.);
#18984=ORIENTED_EDGE('',*,*,#14369,.F.);
#18985=ORIENTED_EDGE('',*,*,#14568,.T.);
#18986=ORIENTED_EDGE('',*,*,#14395,.F.);
#18987=ORIENTED_EDGE('',*,*,#14559,.F.);
#18988=ORIENTED_EDGE('',*,*,#14396,.F.);
#18989=ORIENTED_EDGE('',*,*,#14568,.F.);
#18990=ORIENTED_EDGE('',*,*,#14374,.F.);
#18991=ORIENTED_EDGE('',*,*,#14569,.T.);
#18992=ORIENTED_EDGE('',*,*,#14398,.F.);
#18993=ORIENTED_EDGE('',*,*,#14558,.F.);
#18994=ORIENTED_EDGE('',*,*,#14399,.F.);
#18995=ORIENTED_EDGE('',*,*,#14569,.F.);
#18996=ORIENTED_EDGE('',*,*,#14368,.F.);
#18997=ORIENTED_EDGE('',*,*,#14570,.T.);
#18998=ORIENTED_EDGE('',*,*,#14401,.F.);
#18999=ORIENTED_EDGE('',*,*,#14557,.F.);
#19000=ORIENTED_EDGE('',*,*,#14402,.F.);
#19001=ORIENTED_EDGE('',*,*,#14570,.F.);
#19002=ORIENTED_EDGE('',*,*,#14375,.F.);
#19003=ORIENTED_EDGE('',*,*,#14571,.T.);
#19004=ORIENTED_EDGE('',*,*,#14404,.F.);
#19005=ORIENTED_EDGE('',*,*,#14567,.F.);
#19006=ORIENTED_EDGE('',*,*,#14405,.F.);
#19007=ORIENTED_EDGE('',*,*,#14571,.F.);
#19008=ORIENTED_EDGE('',*,*,#14572,.F.);
#19009=ORIENTED_EDGE('',*,*,#14573,.T.);
#19010=ORIENTED_EDGE('',*,*,#14563,.F.);
#19011=ORIENTED_EDGE('',*,*,#14564,.F.);
#19012=ORIENTED_EDGE('',*,*,#14573,.F.);
#19013=ORIENTED_EDGE('',*,*,#14574,.F.);
#19014=ORIENTED_EDGE('',*,*,#14521,.T.);
#19015=ORIENTED_EDGE('',*,*,#14575,.T.);
#19016=ORIENTED_EDGE('',*,*,#14576,.T.);
#19017=ORIENTED_EDGE('',*,*,#14577,.F.);
#19018=ORIENTED_EDGE('',*,*,#14495,.T.);
#19019=ORIENTED_EDGE('',*,*,#14578,.T.);
#19020=ORIENTED_EDGE('',*,*,#14579,.T.);
#19021=ORIENTED_EDGE('',*,*,#14580,.F.);
#19022=ORIENTED_EDGE('',*,*,#14481,.T.);
#19023=ORIENTED_EDGE('',*,*,#14581,.T.);
#19024=ORIENTED_EDGE('',*,*,#14582,.T.);
#19025=ORIENTED_EDGE('',*,*,#14583,.F.);
#19026=ORIENTED_EDGE('',*,*,#14505,.T.);
#19027=ORIENTED_EDGE('',*,*,#14584,.T.);
#19028=ORIENTED_EDGE('',*,*,#14585,.T.);
#19029=ORIENTED_EDGE('',*,*,#14586,.T.);
#19030=ORIENTED_EDGE('',*,*,#14587,.F.);
#19031=ORIENTED_EDGE('',*,*,#14507,.T.);
#19032=ORIENTED_EDGE('',*,*,#14588,.T.);
#19033=ORIENTED_EDGE('',*,*,#14589,.T.);
#19034=ORIENTED_EDGE('',*,*,#14510,.F.);
#19035=ORIENTED_EDGE('',*,*,#14590,.T.);
#19036=ORIENTED_EDGE('',*,*,#14591,.T.);
#19037=ORIENTED_EDGE('',*,*,#14592,.F.);
#19038=ORIENTED_EDGE('',*,*,#14509,.F.);
#19039=ORIENTED_EDGE('',*,*,#14593,.T.);
#19040=ORIENTED_EDGE('',*,*,#14594,.T.);
#19041=ORIENTED_EDGE('',*,*,#14590,.F.);
#19042=ORIENTED_EDGE('',*,*,#14508,.F.);
#19043=ORIENTED_EDGE('',*,*,#14587,.T.);
#19044=ORIENTED_EDGE('',*,*,#14595,.T.);
#19045=ORIENTED_EDGE('',*,*,#14593,.F.);
#19046=ORIENTED_EDGE('',*,*,#14506,.T.);
#19047=ORIENTED_EDGE('',*,*,#14583,.T.);
#19048=ORIENTED_EDGE('',*,*,#14596,.T.);
#19049=ORIENTED_EDGE('',*,*,#14588,.F.);
#19050=ORIENTED_EDGE('',*,*,#14512,.F.);
#19051=ORIENTED_EDGE('',*,*,#14597,.T.);
#19052=ORIENTED_EDGE('',*,*,#14598,.T.);
#19053=ORIENTED_EDGE('',*,*,#14585,.F.);
#19054=ORIENTED_EDGE('',*,*,#14599,.T.);
#19055=ORIENTED_EDGE('',*,*,#14600,.T.);
#19056=ORIENTED_EDGE('',*,*,#14601,.F.);
#19057=ORIENTED_EDGE('',*,*,#14511,.F.);
#19058=ORIENTED_EDGE('',*,*,#14592,.T.);
#19059=ORIENTED_EDGE('',*,*,#14602,.T.);
#19060=ORIENTED_EDGE('',*,*,#14597,.F.);
#19061=ORIENTED_EDGE('',*,*,#14602,.F.);
#19062=ORIENTED_EDGE('',*,*,#14591,.F.);
#19063=ORIENTED_EDGE('',*,*,#14594,.F.);
#19064=ORIENTED_EDGE('',*,*,#14595,.F.);
#19065=ORIENTED_EDGE('',*,*,#14589,.F.);
#19066=ORIENTED_EDGE('',*,*,#14596,.F.);
#19067=ORIENTED_EDGE('',*,*,#14586,.F.);
#19068=ORIENTED_EDGE('',*,*,#14598,.F.);
#19069=ORIENTED_EDGE('',*,*,#14478,.F.);
#19070=ORIENTED_EDGE('',*,*,#14603,.T.);
#19071=ORIENTED_EDGE('',*,*,#14604,.T.);
#19072=ORIENTED_EDGE('',*,*,#14605,.F.);
#19073=ORIENTED_EDGE('',*,*,#14477,.F.);
#19074=ORIENTED_EDGE('',*,*,#14606,.T.);
#19075=ORIENTED_EDGE('',*,*,#14607,.T.);
#19076=ORIENTED_EDGE('',*,*,#14603,.F.);
#19077=ORIENTED_EDGE('',*,*,#14476,.F.);
#19078=ORIENTED_EDGE('',*,*,#14608,.T.);
#19079=ORIENTED_EDGE('',*,*,#14609,.T.);
#19080=ORIENTED_EDGE('',*,*,#14606,.F.);
#19081=ORIENTED_EDGE('',*,*,#14475,.F.);
#19082=ORIENTED_EDGE('',*,*,#14610,.T.);
#19083=ORIENTED_EDGE('',*,*,#14611,.T.);
#19084=ORIENTED_EDGE('',*,*,#14608,.F.);
#19085=ORIENTED_EDGE('',*,*,#14474,.F.);
#19086=ORIENTED_EDGE('',*,*,#14612,.T.);
#19087=ORIENTED_EDGE('',*,*,#14613,.T.);
#19088=ORIENTED_EDGE('',*,*,#14610,.F.);
#19089=ORIENTED_EDGE('',*,*,#14473,.F.);
#19090=ORIENTED_EDGE('',*,*,#14614,.T.);
#19091=ORIENTED_EDGE('',*,*,#14615,.T.);
#19092=ORIENTED_EDGE('',*,*,#14612,.F.);
#19093=ORIENTED_EDGE('',*,*,#14472,.F.);
#19094=ORIENTED_EDGE('',*,*,#14616,.T.);
#19095=ORIENTED_EDGE('',*,*,#14617,.T.);
#19096=ORIENTED_EDGE('',*,*,#14614,.F.);
#19097=ORIENTED_EDGE('',*,*,#14471,.F.);
#19098=ORIENTED_EDGE('',*,*,#14618,.T.);
#19099=ORIENTED_EDGE('',*,*,#14619,.T.);
#19100=ORIENTED_EDGE('',*,*,#14616,.F.);
#19101=ORIENTED_EDGE('',*,*,#14470,.F.);
#19102=ORIENTED_EDGE('',*,*,#14580,.T.);
#19103=ORIENTED_EDGE('',*,*,#14620,.T.);
#19104=ORIENTED_EDGE('',*,*,#14618,.F.);
#19105=ORIENTED_EDGE('',*,*,#14480,.T.);
#19106=ORIENTED_EDGE('',*,*,#14621,.T.);
#19107=ORIENTED_EDGE('',*,*,#14622,.T.);
#19108=ORIENTED_EDGE('',*,*,#14581,.F.);
#19109=ORIENTED_EDGE('',*,*,#14479,.F.);
#19110=ORIENTED_EDGE('',*,*,#14605,.T.);
#19111=ORIENTED_EDGE('',*,*,#14623,.T.);
#19112=ORIENTED_EDGE('',*,*,#14621,.F.);
#19113=ORIENTED_EDGE('',*,*,#14623,.F.);
#19114=ORIENTED_EDGE('',*,*,#14604,.F.);
#19115=ORIENTED_EDGE('',*,*,#14607,.F.);
#19116=ORIENTED_EDGE('',*,*,#14609,.F.);
#19117=ORIENTED_EDGE('',*,*,#14611,.F.);
#19118=ORIENTED_EDGE('',*,*,#14613,.F.);
#19119=ORIENTED_EDGE('',*,*,#14615,.F.);
#19120=ORIENTED_EDGE('',*,*,#14617,.F.);
#19121=ORIENTED_EDGE('',*,*,#14619,.F.);
#19122=ORIENTED_EDGE('',*,*,#14620,.F.);
#19123=ORIENTED_EDGE('',*,*,#14582,.F.);
#19124=ORIENTED_EDGE('',*,*,#14622,.F.);
#19125=ORIENTED_EDGE('',*,*,#14492,.F.);
#19126=ORIENTED_EDGE('',*,*,#14624,.T.);
#19127=ORIENTED_EDGE('',*,*,#14625,.T.);
#19128=ORIENTED_EDGE('',*,*,#14626,.F.);
#19129=ORIENTED_EDGE('',*,*,#14491,.F.);
#19130=ORIENTED_EDGE('',*,*,#14627,.T.);
#19131=ORIENTED_EDGE('',*,*,#14628,.T.);
#19132=ORIENTED_EDGE('',*,*,#14624,.F.);
#19133=ORIENTED_EDGE('',*,*,#14490,.F.);
#19134=ORIENTED_EDGE('',*,*,#14629,.T.);
#19135=ORIENTED_EDGE('',*,*,#14630,.T.);
#19136=ORIENTED_EDGE('',*,*,#14627,.F.);
#19137=ORIENTED_EDGE('',*,*,#14489,.F.);
#19138=ORIENTED_EDGE('',*,*,#14631,.T.);
#19139=ORIENTED_EDGE('',*,*,#14632,.T.);
#19140=ORIENTED_EDGE('',*,*,#14629,.F.);
#19141=ORIENTED_EDGE('',*,*,#14488,.F.);
#19142=ORIENTED_EDGE('',*,*,#14633,.T.);
#19143=ORIENTED_EDGE('',*,*,#14634,.T.);
#19144=ORIENTED_EDGE('',*,*,#14631,.F.);
#19145=ORIENTED_EDGE('',*,*,#14487,.F.);
#19146=ORIENTED_EDGE('',*,*,#14635,.T.);
#19147=ORIENTED_EDGE('',*,*,#14636,.T.);
#19148=ORIENTED_EDGE('',*,*,#14633,.F.);
#19149=ORIENTED_EDGE('',*,*,#14486,.F.);
#19150=ORIENTED_EDGE('',*,*,#14637,.T.);
#19151=ORIENTED_EDGE('',*,*,#14638,.T.);
#19152=ORIENTED_EDGE('',*,*,#14635,.F.);
#19153=ORIENTED_EDGE('',*,*,#14485,.F.);
#19154=ORIENTED_EDGE('',*,*,#14639,.T.);
#19155=ORIENTED_EDGE('',*,*,#14640,.T.);
#19156=ORIENTED_EDGE('',*,*,#14637,.F.);
#19157=ORIENTED_EDGE('',*,*,#14484,.F.);
#19158=ORIENTED_EDGE('',*,*,#14641,.T.);
#19159=ORIENTED_EDGE('',*,*,#14642,.T.);
#19160=ORIENTED_EDGE('',*,*,#14639,.F.);
#19161=ORIENTED_EDGE('',*,*,#14483,.F.);
#19162=ORIENTED_EDGE('',*,*,#14643,.T.);
#19163=ORIENTED_EDGE('',*,*,#14644,.T.);
#19164=ORIENTED_EDGE('',*,*,#14641,.F.);
#19165=ORIENTED_EDGE('',*,*,#14482,.F.);
#19166=ORIENTED_EDGE('',*,*,#14577,.T.);
#19167=ORIENTED_EDGE('',*,*,#14645,.T.);
#19168=ORIENTED_EDGE('',*,*,#14643,.F.);
#19169=ORIENTED_EDGE('',*,*,#14494,.T.);
#19170=ORIENTED_EDGE('',*,*,#14646,.T.);
#19171=ORIENTED_EDGE('',*,*,#14647,.T.);
#19172=ORIENTED_EDGE('',*,*,#14578,.F.);
#19173=ORIENTED_EDGE('',*,*,#14493,.F.);
#19174=ORIENTED_EDGE('',*,*,#14626,.T.);
#19175=ORIENTED_EDGE('',*,*,#14648,.T.);
#19176=ORIENTED_EDGE('',*,*,#14646,.F.);
#19177=ORIENTED_EDGE('',*,*,#14648,.F.);
#19178=ORIENTED_EDGE('',*,*,#14625,.F.);
#19179=ORIENTED_EDGE('',*,*,#14628,.F.);
#19180=ORIENTED_EDGE('',*,*,#14630,.F.);
#19181=ORIENTED_EDGE('',*,*,#14632,.F.);
#19182=ORIENTED_EDGE('',*,*,#14634,.F.);
#19183=ORIENTED_EDGE('',*,*,#14636,.F.);
#19184=ORIENTED_EDGE('',*,*,#14638,.F.);
#19185=ORIENTED_EDGE('',*,*,#14640,.F.);
#19186=ORIENTED_EDGE('',*,*,#14642,.F.);
#19187=ORIENTED_EDGE('',*,*,#14644,.F.);
#19188=ORIENTED_EDGE('',*,*,#14645,.F.);
#19189=ORIENTED_EDGE('',*,*,#14579,.F.);
#19190=ORIENTED_EDGE('',*,*,#14647,.F.);
#19191=ORIENTED_EDGE('',*,*,#14424,.F.);
#19192=ORIENTED_EDGE('',*,*,#14649,.T.);
#19193=ORIENTED_EDGE('',*,*,#14650,.T.);
#19194=ORIENTED_EDGE('',*,*,#14651,.F.);
#19195=ORIENTED_EDGE('',*,*,#14458,.F.);
#19196=ORIENTED_EDGE('',*,*,#14652,.T.);
#19197=ORIENTED_EDGE('',*,*,#14653,.T.);
#19198=ORIENTED_EDGE('',*,*,#14649,.F.);
#19199=ORIENTED_EDGE('',*,*,#14457,.F.);
#19200=ORIENTED_EDGE('',*,*,#14654,.T.);
#19201=ORIENTED_EDGE('',*,*,#14655,.T.);
#19202=ORIENTED_EDGE('',*,*,#14652,.F.);
#19203=ORIENTED_EDGE('',*,*,#14456,.F.);
#19204=ORIENTED_EDGE('',*,*,#14656,.T.);
#19205=ORIENTED_EDGE('',*,*,#14657,.T.);
#19206=ORIENTED_EDGE('',*,*,#14654,.F.);
#19207=ORIENTED_EDGE('',*,*,#14455,.F.);
#19208=ORIENTED_EDGE('',*,*,#14658,.T.);
#19209=ORIENTED_EDGE('',*,*,#14659,.T.);
#19210=ORIENTED_EDGE('',*,*,#14656,.F.);
#19211=ORIENTED_EDGE('',*,*,#14454,.F.);
#19212=ORIENTED_EDGE('',*,*,#14660,.T.);
#19213=ORIENTED_EDGE('',*,*,#14661,.T.);
#19214=ORIENTED_EDGE('',*,*,#14658,.F.);
#19215=ORIENTED_EDGE('',*,*,#14453,.F.);
#19216=ORIENTED_EDGE('',*,*,#14662,.T.);
#19217=ORIENTED_EDGE('',*,*,#14663,.T.);
#19218=ORIENTED_EDGE('',*,*,#14660,.F.);
#19219=ORIENTED_EDGE('',*,*,#14452,.F.);
#19220=ORIENTED_EDGE('',*,*,#14664,.T.);
#19221=ORIENTED_EDGE('',*,*,#14665,.T.);
#19222=ORIENTED_EDGE('',*,*,#14662,.F.);
#19223=ORIENTED_EDGE('',*,*,#14451,.F.);
#19224=ORIENTED_EDGE('',*,*,#14666,.T.);
#19225=ORIENTED_EDGE('',*,*,#14667,.T.);
#19226=ORIENTED_EDGE('',*,*,#14664,.F.);
#19227=ORIENTED_EDGE('',*,*,#14450,.F.);
#19228=ORIENTED_EDGE('',*,*,#14668,.T.);
#19229=ORIENTED_EDGE('',*,*,#14669,.T.);
#19230=ORIENTED_EDGE('',*,*,#14666,.F.);
#19231=ORIENTED_EDGE('',*,*,#14449,.F.);
#19232=ORIENTED_EDGE('',*,*,#14670,.T.);
#19233=ORIENTED_EDGE('',*,*,#14671,.T.);
#19234=ORIENTED_EDGE('',*,*,#14668,.F.);
#19235=ORIENTED_EDGE('',*,*,#14448,.F.);
#19236=ORIENTED_EDGE('',*,*,#14672,.T.);
#19237=ORIENTED_EDGE('',*,*,#14673,.T.);
#19238=ORIENTED_EDGE('',*,*,#14670,.F.);
#19239=ORIENTED_EDGE('',*,*,#14447,.F.);
#19240=ORIENTED_EDGE('',*,*,#14674,.T.);
#19241=ORIENTED_EDGE('',*,*,#14675,.T.);
#19242=ORIENTED_EDGE('',*,*,#14672,.F.);
#19243=ORIENTED_EDGE('',*,*,#14446,.F.);
#19244=ORIENTED_EDGE('',*,*,#14676,.T.);
#19245=ORIENTED_EDGE('',*,*,#14677,.T.);
#19246=ORIENTED_EDGE('',*,*,#14674,.F.);
#19247=ORIENTED_EDGE('',*,*,#14445,.F.);
#19248=ORIENTED_EDGE('',*,*,#14678,.T.);
#19249=ORIENTED_EDGE('',*,*,#14679,.T.);
#19250=ORIENTED_EDGE('',*,*,#14676,.F.);
#19251=ORIENTED_EDGE('',*,*,#14444,.F.);
#19252=ORIENTED_EDGE('',*,*,#14680,.T.);
#19253=ORIENTED_EDGE('',*,*,#14681,.T.);
#19254=ORIENTED_EDGE('',*,*,#14678,.F.);
#19255=ORIENTED_EDGE('',*,*,#14443,.F.);
#19256=ORIENTED_EDGE('',*,*,#14682,.T.);
#19257=ORIENTED_EDGE('',*,*,#14683,.T.);
#19258=ORIENTED_EDGE('',*,*,#14680,.F.);
#19259=ORIENTED_EDGE('',*,*,#14442,.F.);
#19260=ORIENTED_EDGE('',*,*,#14684,.T.);
#19261=ORIENTED_EDGE('',*,*,#14685,.T.);
#19262=ORIENTED_EDGE('',*,*,#14682,.F.);
#19263=ORIENTED_EDGE('',*,*,#14441,.F.);
#19264=ORIENTED_EDGE('',*,*,#14686,.T.);
#19265=ORIENTED_EDGE('',*,*,#14687,.T.);
#19266=ORIENTED_EDGE('',*,*,#14684,.F.);
#19267=ORIENTED_EDGE('',*,*,#14440,.F.);
#19268=ORIENTED_EDGE('',*,*,#14688,.T.);
#19269=ORIENTED_EDGE('',*,*,#14689,.T.);
#19270=ORIENTED_EDGE('',*,*,#14686,.F.);
#19271=ORIENTED_EDGE('',*,*,#14439,.F.);
#19272=ORIENTED_EDGE('',*,*,#14690,.T.);
#19273=ORIENTED_EDGE('',*,*,#14691,.T.);
#19274=ORIENTED_EDGE('',*,*,#14688,.F.);
#19275=ORIENTED_EDGE('',*,*,#14438,.F.);
#19276=ORIENTED_EDGE('',*,*,#14692,.T.);
#19277=ORIENTED_EDGE('',*,*,#14693,.T.);
#19278=ORIENTED_EDGE('',*,*,#14690,.F.);
#19279=ORIENTED_EDGE('',*,*,#14437,.F.);
#19280=ORIENTED_EDGE('',*,*,#14694,.T.);
#19281=ORIENTED_EDGE('',*,*,#14695,.T.);
#19282=ORIENTED_EDGE('',*,*,#14692,.F.);
#19283=ORIENTED_EDGE('',*,*,#14436,.F.);
#19284=ORIENTED_EDGE('',*,*,#14696,.T.);
#19285=ORIENTED_EDGE('',*,*,#14697,.T.);
#19286=ORIENTED_EDGE('',*,*,#14694,.F.);
#19287=ORIENTED_EDGE('',*,*,#14435,.F.);
#19288=ORIENTED_EDGE('',*,*,#14698,.T.);
#19289=ORIENTED_EDGE('',*,*,#14699,.T.);
#19290=ORIENTED_EDGE('',*,*,#14696,.F.);
#19291=ORIENTED_EDGE('',*,*,#14434,.F.);
#19292=ORIENTED_EDGE('',*,*,#14700,.T.);
#19293=ORIENTED_EDGE('',*,*,#14701,.T.);
#19294=ORIENTED_EDGE('',*,*,#14698,.F.);
#19295=ORIENTED_EDGE('',*,*,#14433,.F.);
#19296=ORIENTED_EDGE('',*,*,#14702,.T.);
#19297=ORIENTED_EDGE('',*,*,#14703,.T.);
#19298=ORIENTED_EDGE('',*,*,#14700,.F.);
#19299=ORIENTED_EDGE('',*,*,#14432,.F.);
#19300=ORIENTED_EDGE('',*,*,#14704,.T.);
#19301=ORIENTED_EDGE('',*,*,#14705,.T.);
#19302=ORIENTED_EDGE('',*,*,#14702,.F.);
#19303=ORIENTED_EDGE('',*,*,#14431,.F.);
#19304=ORIENTED_EDGE('',*,*,#14706,.T.);
#19305=ORIENTED_EDGE('',*,*,#14707,.T.);
#19306=ORIENTED_EDGE('',*,*,#14704,.F.);
#19307=ORIENTED_EDGE('',*,*,#14430,.F.);
#19308=ORIENTED_EDGE('',*,*,#14708,.T.);
#19309=ORIENTED_EDGE('',*,*,#14709,.T.);
#19310=ORIENTED_EDGE('',*,*,#14706,.F.);
#19311=ORIENTED_EDGE('',*,*,#14429,.F.);
#19312=ORIENTED_EDGE('',*,*,#14710,.T.);
#19313=ORIENTED_EDGE('',*,*,#14711,.T.);
#19314=ORIENTED_EDGE('',*,*,#14708,.F.);
#19315=ORIENTED_EDGE('',*,*,#14428,.F.);
#19316=ORIENTED_EDGE('',*,*,#14712,.T.);
#19317=ORIENTED_EDGE('',*,*,#14713,.T.);
#19318=ORIENTED_EDGE('',*,*,#14710,.F.);
#19319=ORIENTED_EDGE('',*,*,#14427,.F.);
#19320=ORIENTED_EDGE('',*,*,#14714,.T.);
#19321=ORIENTED_EDGE('',*,*,#14715,.T.);
#19322=ORIENTED_EDGE('',*,*,#14712,.F.);
#19323=ORIENTED_EDGE('',*,*,#14426,.F.);
#19324=ORIENTED_EDGE('',*,*,#14716,.T.);
#19325=ORIENTED_EDGE('',*,*,#14717,.T.);
#19326=ORIENTED_EDGE('',*,*,#14714,.F.);
#19327=ORIENTED_EDGE('',*,*,#14425,.F.);
#19328=ORIENTED_EDGE('',*,*,#14651,.T.);
#19329=ORIENTED_EDGE('',*,*,#14718,.T.);
#19330=ORIENTED_EDGE('',*,*,#14716,.F.);
#19331=ORIENTED_EDGE('',*,*,#14718,.F.);
#19332=ORIENTED_EDGE('',*,*,#14650,.F.);
#19333=ORIENTED_EDGE('',*,*,#14653,.F.);
#19334=ORIENTED_EDGE('',*,*,#14655,.F.);
#19335=ORIENTED_EDGE('',*,*,#14657,.F.);
#19336=ORIENTED_EDGE('',*,*,#14659,.F.);
#19337=ORIENTED_EDGE('',*,*,#14661,.F.);
#19338=ORIENTED_EDGE('',*,*,#14663,.F.);
#19339=ORIENTED_EDGE('',*,*,#14665,.F.);
#19340=ORIENTED_EDGE('',*,*,#14667,.F.);
#19341=ORIENTED_EDGE('',*,*,#14669,.F.);
#19342=ORIENTED_EDGE('',*,*,#14671,.F.);
#19343=ORIENTED_EDGE('',*,*,#14673,.F.);
#19344=ORIENTED_EDGE('',*,*,#14675,.F.);
#19345=ORIENTED_EDGE('',*,*,#14677,.F.);
#19346=ORIENTED_EDGE('',*,*,#14679,.F.);
#19347=ORIENTED_EDGE('',*,*,#14681,.F.);
#19348=ORIENTED_EDGE('',*,*,#14683,.F.);
#19349=ORIENTED_EDGE('',*,*,#14685,.F.);
#19350=ORIENTED_EDGE('',*,*,#14687,.F.);
#19351=ORIENTED_EDGE('',*,*,#14689,.F.);
#19352=ORIENTED_EDGE('',*,*,#14691,.F.);
#19353=ORIENTED_EDGE('',*,*,#14693,.F.);
#19354=ORIENTED_EDGE('',*,*,#14695,.F.);
#19355=ORIENTED_EDGE('',*,*,#14697,.F.);
#19356=ORIENTED_EDGE('',*,*,#14699,.F.);
#19357=ORIENTED_EDGE('',*,*,#14701,.F.);
#19358=ORIENTED_EDGE('',*,*,#14703,.F.);
#19359=ORIENTED_EDGE('',*,*,#14705,.F.);
#19360=ORIENTED_EDGE('',*,*,#14707,.F.);
#19361=ORIENTED_EDGE('',*,*,#14709,.F.);
#19362=ORIENTED_EDGE('',*,*,#14711,.F.);
#19363=ORIENTED_EDGE('',*,*,#14713,.F.);
#19364=ORIENTED_EDGE('',*,*,#14715,.F.);
#19365=ORIENTED_EDGE('',*,*,#14717,.F.);
#19366=ORIENTED_EDGE('',*,*,#14518,.F.);
#19367=ORIENTED_EDGE('',*,*,#14719,.T.);
#19368=ORIENTED_EDGE('',*,*,#14720,.T.);
#19369=ORIENTED_EDGE('',*,*,#14721,.F.);
#19370=ORIENTED_EDGE('',*,*,#14517,.F.);
#19371=ORIENTED_EDGE('',*,*,#14722,.T.);
#19372=ORIENTED_EDGE('',*,*,#14723,.T.);
#19373=ORIENTED_EDGE('',*,*,#14719,.F.);
#19374=ORIENTED_EDGE('',*,*,#14516,.F.);
#19375=ORIENTED_EDGE('',*,*,#14724,.T.);
#19376=ORIENTED_EDGE('',*,*,#14725,.T.);
#19377=ORIENTED_EDGE('',*,*,#14722,.F.);
#19378=ORIENTED_EDGE('',*,*,#14515,.F.);
#19379=ORIENTED_EDGE('',*,*,#14726,.T.);
#19380=ORIENTED_EDGE('',*,*,#14727,.T.);
#19381=ORIENTED_EDGE('',*,*,#14724,.F.);
#19382=ORIENTED_EDGE('',*,*,#14514,.F.);
#19383=ORIENTED_EDGE('',*,*,#14728,.T.);
#19384=ORIENTED_EDGE('',*,*,#14729,.T.);
#19385=ORIENTED_EDGE('',*,*,#14726,.F.);
#19386=ORIENTED_EDGE('',*,*,#14513,.F.);
#19387=ORIENTED_EDGE('',*,*,#14601,.T.);
#19388=ORIENTED_EDGE('',*,*,#14730,.T.);
#19389=ORIENTED_EDGE('',*,*,#14728,.F.);
#19390=ORIENTED_EDGE('',*,*,#14584,.F.);
#19391=ORIENTED_EDGE('',*,*,#14504,.F.);
#19392=ORIENTED_EDGE('',*,*,#14731,.T.);
#19393=ORIENTED_EDGE('',*,*,#14732,.T.);
#19394=ORIENTED_EDGE('',*,*,#14599,.F.);
#19395=ORIENTED_EDGE('',*,*,#14503,.F.);
#19396=ORIENTED_EDGE('',*,*,#14733,.T.);
#19397=ORIENTED_EDGE('',*,*,#14734,.T.);
#19398=ORIENTED_EDGE('',*,*,#14731,.F.);
#19399=ORIENTED_EDGE('',*,*,#14502,.F.);
#19400=ORIENTED_EDGE('',*,*,#14735,.T.);
#19401=ORIENTED_EDGE('',*,*,#14736,.T.);
#19402=ORIENTED_EDGE('',*,*,#14733,.F.);
#19403=ORIENTED_EDGE('',*,*,#14501,.F.);
#19404=ORIENTED_EDGE('',*,*,#14737,.T.);
#19405=ORIENTED_EDGE('',*,*,#14738,.T.);
#19406=ORIENTED_EDGE('',*,*,#14735,.F.);
#19407=ORIENTED_EDGE('',*,*,#14500,.F.);
#19408=ORIENTED_EDGE('',*,*,#14739,.T.);
#19409=ORIENTED_EDGE('',*,*,#14740,.T.);
#19410=ORIENTED_EDGE('',*,*,#14737,.F.);
#19411=ORIENTED_EDGE('',*,*,#14499,.F.);
#19412=ORIENTED_EDGE('',*,*,#14741,.T.);
#19413=ORIENTED_EDGE('',*,*,#14742,.T.);
#19414=ORIENTED_EDGE('',*,*,#14739,.F.);
#19415=ORIENTED_EDGE('',*,*,#14498,.F.);
#19416=ORIENTED_EDGE('',*,*,#14743,.T.);
#19417=ORIENTED_EDGE('',*,*,#14744,.T.);
#19418=ORIENTED_EDGE('',*,*,#14741,.F.);
#19419=ORIENTED_EDGE('',*,*,#14497,.F.);
#19420=ORIENTED_EDGE('',*,*,#14745,.T.);
#19421=ORIENTED_EDGE('',*,*,#14746,.T.);
#19422=ORIENTED_EDGE('',*,*,#14743,.F.);
#19423=ORIENTED_EDGE('',*,*,#14496,.F.);
#19424=ORIENTED_EDGE('',*,*,#14574,.T.);
#19425=ORIENTED_EDGE('',*,*,#14747,.T.);
#19426=ORIENTED_EDGE('',*,*,#14745,.F.);
#19427=ORIENTED_EDGE('',*,*,#14520,.T.);
#19428=ORIENTED_EDGE('',*,*,#14748,.T.);
#19429=ORIENTED_EDGE('',*,*,#14749,.T.);
#19430=ORIENTED_EDGE('',*,*,#14575,.F.);
#19431=ORIENTED_EDGE('',*,*,#14519,.F.);
#19432=ORIENTED_EDGE('',*,*,#14721,.T.);
#19433=ORIENTED_EDGE('',*,*,#14750,.T.);
#19434=ORIENTED_EDGE('',*,*,#14748,.F.);
#19435=ORIENTED_EDGE('',*,*,#14750,.F.);
#19436=ORIENTED_EDGE('',*,*,#14720,.F.);
#19437=ORIENTED_EDGE('',*,*,#14723,.F.);
#19438=ORIENTED_EDGE('',*,*,#14725,.F.);
#19439=ORIENTED_EDGE('',*,*,#14727,.F.);
#19440=ORIENTED_EDGE('',*,*,#14729,.F.);
#19441=ORIENTED_EDGE('',*,*,#14730,.F.);
#19442=ORIENTED_EDGE('',*,*,#14600,.F.);
#19443=ORIENTED_EDGE('',*,*,#14732,.F.);
#19444=ORIENTED_EDGE('',*,*,#14734,.F.);
#19445=ORIENTED_EDGE('',*,*,#14736,.F.);
#19446=ORIENTED_EDGE('',*,*,#14738,.F.);
#19447=ORIENTED_EDGE('',*,*,#14740,.F.);
#19448=ORIENTED_EDGE('',*,*,#14742,.F.);
#19449=ORIENTED_EDGE('',*,*,#14744,.F.);
#19450=ORIENTED_EDGE('',*,*,#14746,.F.);
#19451=ORIENTED_EDGE('',*,*,#14747,.F.);
#19452=ORIENTED_EDGE('',*,*,#14576,.F.);
#19453=ORIENTED_EDGE('',*,*,#14749,.F.);
#19454=ORIENTED_EDGE('',*,*,#14459,.F.);
#19455=ORIENTED_EDGE('',*,*,#14751,.T.);
#19456=ORIENTED_EDGE('',*,*,#14752,.T.);
#19457=ORIENTED_EDGE('',*,*,#14753,.F.);
#19458=ORIENTED_EDGE('',*,*,#14469,.F.);
#19459=ORIENTED_EDGE('',*,*,#14754,.T.);
#19460=ORIENTED_EDGE('',*,*,#14755,.T.);
#19461=ORIENTED_EDGE('',*,*,#14751,.F.);
#19462=ORIENTED_EDGE('',*,*,#14468,.F.);
#19463=ORIENTED_EDGE('',*,*,#14756,.T.);
#19464=ORIENTED_EDGE('',*,*,#14757,.T.);
#19465=ORIENTED_EDGE('',*,*,#14754,.F.);
#19466=ORIENTED_EDGE('',*,*,#14467,.F.);
#19467=ORIENTED_EDGE('',*,*,#14758,.T.);
#19468=ORIENTED_EDGE('',*,*,#14759,.T.);
#19469=ORIENTED_EDGE('',*,*,#14756,.F.);
#19470=ORIENTED_EDGE('',*,*,#14466,.F.);
#19471=ORIENTED_EDGE('',*,*,#14760,.T.);
#19472=ORIENTED_EDGE('',*,*,#14761,.T.);
#19473=ORIENTED_EDGE('',*,*,#14758,.F.);
#19474=ORIENTED_EDGE('',*,*,#14465,.F.);
#19475=ORIENTED_EDGE('',*,*,#14762,.T.);
#19476=ORIENTED_EDGE('',*,*,#14763,.T.);
#19477=ORIENTED_EDGE('',*,*,#14760,.F.);
#19478=ORIENTED_EDGE('',*,*,#14464,.F.);
#19479=ORIENTED_EDGE('',*,*,#14764,.T.);
#19480=ORIENTED_EDGE('',*,*,#14765,.T.);
#19481=ORIENTED_EDGE('',*,*,#14762,.F.);
#19482=ORIENTED_EDGE('',*,*,#14463,.F.);
#19483=ORIENTED_EDGE('',*,*,#14766,.T.);
#19484=ORIENTED_EDGE('',*,*,#14767,.T.);
#19485=ORIENTED_EDGE('',*,*,#14764,.F.);
#19486=ORIENTED_EDGE('',*,*,#14462,.F.);
#19487=ORIENTED_EDGE('',*,*,#14768,.T.);
#19488=ORIENTED_EDGE('',*,*,#14769,.T.);
#19489=ORIENTED_EDGE('',*,*,#14766,.F.);
#19490=ORIENTED_EDGE('',*,*,#14461,.F.);
#19491=ORIENTED_EDGE('',*,*,#14770,.T.);
#19492=ORIENTED_EDGE('',*,*,#14771,.T.);
#19493=ORIENTED_EDGE('',*,*,#14768,.F.);
#19494=ORIENTED_EDGE('',*,*,#14460,.F.);
#19495=ORIENTED_EDGE('',*,*,#14753,.T.);
#19496=ORIENTED_EDGE('',*,*,#14772,.T.);
#19497=ORIENTED_EDGE('',*,*,#14770,.F.);
#19498=ORIENTED_EDGE('',*,*,#14772,.F.);
#19499=ORIENTED_EDGE('',*,*,#14752,.F.);
#19500=ORIENTED_EDGE('',*,*,#14755,.F.);
#19501=ORIENTED_EDGE('',*,*,#14757,.F.);
#19502=ORIENTED_EDGE('',*,*,#14759,.F.);
#19503=ORIENTED_EDGE('',*,*,#14761,.F.);
#19504=ORIENTED_EDGE('',*,*,#14763,.F.);
#19505=ORIENTED_EDGE('',*,*,#14765,.F.);
#19506=ORIENTED_EDGE('',*,*,#14767,.F.);
#19507=ORIENTED_EDGE('',*,*,#14769,.F.);
#19508=ORIENTED_EDGE('',*,*,#14771,.F.);
#19509=ORIENTED_EDGE('',*,*,#14370,.F.);
#19510=ORIENTED_EDGE('',*,*,#14773,.T.);
#19511=ORIENTED_EDGE('',*,*,#14417,.F.);
#19512=ORIENTED_EDGE('',*,*,#14560,.F.);
#19513=ORIENTED_EDGE('',*,*,#14418,.F.);
#19514=ORIENTED_EDGE('',*,*,#14773,.F.);
#19515=ORIENTED_EDGE('',*,*,#14371,.F.);
#19516=ORIENTED_EDGE('',*,*,#14774,.T.);
#19517=ORIENTED_EDGE('',*,*,#14410,.F.);
#19518=ORIENTED_EDGE('',*,*,#14565,.F.);
#19519=ORIENTED_EDGE('',*,*,#14411,.F.);
#19520=ORIENTED_EDGE('',*,*,#14774,.F.);
#19521=ORIENTED_EDGE('',*,*,#14372,.F.);
#19522=ORIENTED_EDGE('',*,*,#14775,.T.);
#19523=ORIENTED_EDGE('',*,*,#14414,.F.);
#19524=ORIENTED_EDGE('',*,*,#14561,.F.);
#19525=ORIENTED_EDGE('',*,*,#14415,.F.);
#19526=ORIENTED_EDGE('',*,*,#14775,.F.);
#19527=ORIENTED_EDGE('',*,*,#14373,.F.);
#19528=ORIENTED_EDGE('',*,*,#14776,.T.);
#19529=ORIENTED_EDGE('',*,*,#14407,.F.);
#19530=ORIENTED_EDGE('',*,*,#14566,.F.);
#19531=ORIENTED_EDGE('',*,*,#14408,.F.);
#19532=ORIENTED_EDGE('',*,*,#14776,.F.);
#19533=ORIENTED_EDGE('',*,*,#14572,.T.);
#19534=ORIENTED_EDGE('',*,*,#14551,.F.);
#19535=ORIENTED_EDGE('',*,*,#14539,.F.);
#19536=ORIENTED_EDGE('',*,*,#14777,.T.);
#19537=ORIENTED_EDGE('',*,*,#14778,.T.);
#19538=ORIENTED_EDGE('',*,*,#14779,.F.);
#19539=ORIENTED_EDGE('',*,*,#14543,.F.);
#19540=ORIENTED_EDGE('',*,*,#14556,.T.);
#19541=ORIENTED_EDGE('',*,*,#14780,.T.);
#19542=ORIENTED_EDGE('',*,*,#14777,.F.);
#19543=ORIENTED_EDGE('',*,*,#14544,.F.);
#19544=ORIENTED_EDGE('',*,*,#14779,.T.);
#19545=ORIENTED_EDGE('',*,*,#14781,.T.);
#19546=ORIENTED_EDGE('',*,*,#14552,.F.);
#19547=ORIENTED_EDGE('',*,*,#14781,.F.);
#19548=ORIENTED_EDGE('',*,*,#14778,.F.);
#19549=ORIENTED_EDGE('',*,*,#14780,.F.);
#19550=ORIENTED_EDGE('',*,*,#14555,.F.);
#19551=ORIENTED_EDGE('',*,*,#14553,.F.);
#19552=ORIENTED_EDGE('',*,*,#14290,.F.);
#19553=ORIENTED_EDGE('',*,*,#14523,.F.);
#19554=ORIENTED_EDGE('',*,*,#14535,.F.);
#19555=ORIENTED_EDGE('',*,*,#14380,.F.);
#19556=ORIENTED_EDGE('',*,*,#14782,.T.);
#19557=ORIENTED_EDGE('',*,*,#14783,.T.);
#19558=ORIENTED_EDGE('',*,*,#14784,.T.);
#19559=ORIENTED_EDGE('',*,*,#14783,.F.);
#19560=ORIENTED_EDGE('',*,*,#14785,.F.);
#19561=ORIENTED_EDGE('',*,*,#14786,.T.);
#19562=ORIENTED_EDGE('',*,*,#14784,.F.);
#19563=ORIENTED_EDGE('',*,*,#14786,.F.);
#19564=ORIENTED_EDGE('',*,*,#14787,.T.);
#19565=ORIENTED_EDGE('',*,*,#14788,.F.);
#19566=ORIENTED_EDGE('',*,*,#14789,.T.);
#19567=ORIENTED_EDGE('',*,*,#14790,.F.);
#19568=ORIENTED_EDGE('',*,*,#14791,.T.);
#19569=ORIENTED_EDGE('',*,*,#14792,.F.);
#19570=ORIENTED_EDGE('',*,*,#14793,.T.);
#19571=ORIENTED_EDGE('',*,*,#14794,.F.);
#19572=ORIENTED_EDGE('',*,*,#14782,.F.);
#19573=ORIENTED_EDGE('',*,*,#14785,.T.);
#19574=ORIENTED_EDGE('',*,*,#14795,.T.);
#19575=ORIENTED_EDGE('',*,*,#14796,.T.);
#19576=ORIENTED_EDGE('',*,*,#14795,.F.);
#19577=ORIENTED_EDGE('',*,*,#14797,.F.);
#19578=ORIENTED_EDGE('',*,*,#14796,.F.);
#19579=ORIENTED_EDGE('',*,*,#14798,.T.);
#19580=ORIENTED_EDGE('',*,*,#14799,.T.);
#19581=ORIENTED_EDGE('',*,*,#14800,.T.);
#19582=ORIENTED_EDGE('',*,*,#14799,.F.);
#19583=ORIENTED_EDGE('',*,*,#14801,.T.);
#19584=ORIENTED_EDGE('',*,*,#14802,.T.);
#19585=ORIENTED_EDGE('',*,*,#14803,.T.);
#19586=ORIENTED_EDGE('',*,*,#14804,.T.);
#19587=ORIENTED_EDGE('',*,*,#14805,.T.);
#19588=ORIENTED_EDGE('',*,*,#14806,.T.);
#19589=ORIENTED_EDGE('',*,*,#14807,.F.);
#19590=ORIENTED_EDGE('',*,*,#14807,.T.);
#19591=ORIENTED_EDGE('',*,*,#14808,.T.);
#19592=ORIENTED_EDGE('',*,*,#14809,.T.);
#19593=ORIENTED_EDGE('',*,*,#14810,.T.);
#19594=ORIENTED_EDGE('',*,*,#14811,.F.);
#19595=ORIENTED_EDGE('',*,*,#14812,.F.);
#19596=ORIENTED_EDGE('',*,*,#14813,.F.);
#19597=ORIENTED_EDGE('',*,*,#14814,.F.);
#19598=ORIENTED_EDGE('',*,*,#14815,.F.);
#19599=ORIENTED_EDGE('',*,*,#14816,.F.);
#19600=ORIENTED_EDGE('',*,*,#14817,.F.);
#19601=ORIENTED_EDGE('',*,*,#14818,.F.);
#19602=ORIENTED_EDGE('',*,*,#14819,.F.);
#19603=ORIENTED_EDGE('',*,*,#14798,.F.);
#19604=ORIENTED_EDGE('',*,*,#14800,.F.);
#19605=ORIENTED_EDGE('',*,*,#14820,.T.);
#19606=ORIENTED_EDGE('',*,*,#14821,.F.);
#19607=ORIENTED_EDGE('',*,*,#14820,.F.);
#19608=ORIENTED_EDGE('',*,*,#14811,.T.);
#19609=ORIENTED_EDGE('',*,*,#14822,.T.);
#19610=ORIENTED_EDGE('',*,*,#14823,.T.);
#19611=ORIENTED_EDGE('',*,*,#14822,.F.);
#19612=ORIENTED_EDGE('',*,*,#14823,.F.);
#19613=ORIENTED_EDGE('',*,*,#14824,.T.);
#19614=ORIENTED_EDGE('',*,*,#14825,.F.);
#19615=ORIENTED_EDGE('',*,*,#14824,.F.);
#19616=ORIENTED_EDGE('',*,*,#14826,.T.);
#19617=ORIENTED_EDGE('',*,*,#14827,.T.);
#19618=ORIENTED_EDGE('',*,*,#14828,.T.);
#19619=ORIENTED_EDGE('',*,*,#14829,.T.);
#19620=ORIENTED_EDGE('',*,*,#14826,.F.);
#19621=ORIENTED_EDGE('',*,*,#14830,.T.);
#19622=ORIENTED_EDGE('',*,*,#14828,.F.);
#19623=ORIENTED_EDGE('',*,*,#14831,.T.);
#19624=ORIENTED_EDGE('',*,*,#14832,.T.);
#19625=ORIENTED_EDGE('',*,*,#14829,.F.);
#19626=ORIENTED_EDGE('',*,*,#14833,.F.);
#19627=ORIENTED_EDGE('',*,*,#14834,.F.);
#19628=ORIENTED_EDGE('',*,*,#14835,.F.);
#19629=ORIENTED_EDGE('',*,*,#14790,.T.);
#19630=ORIENTED_EDGE('',*,*,#14836,.T.);
#19631=ORIENTED_EDGE('',*,*,#14837,.F.);
#19632=ORIENTED_EDGE('',*,*,#14838,.T.);
#19633=ORIENTED_EDGE('',*,*,#14839,.F.);
#19634=ORIENTED_EDGE('',*,*,#14840,.T.);
#19635=ORIENTED_EDGE('',*,*,#14841,.T.);
#19636=ORIENTED_EDGE('',*,*,#14842,.T.);
#19637=ORIENTED_EDGE('',*,*,#14843,.F.);
#19638=ORIENTED_EDGE('',*,*,#14844,.F.);
#19639=ORIENTED_EDGE('',*,*,#14845,.F.);
#19640=ORIENTED_EDGE('',*,*,#14846,.F.);
#19641=ORIENTED_EDGE('',*,*,#14847,.F.);
#19642=ORIENTED_EDGE('',*,*,#14848,.F.);
#19643=ORIENTED_EDGE('',*,*,#14849,.F.);
#19644=ORIENTED_EDGE('',*,*,#14850,.F.);
#19645=ORIENTED_EDGE('',*,*,#14851,.F.);
#19646=ORIENTED_EDGE('',*,*,#14852,.F.);
#19647=ORIENTED_EDGE('',*,*,#14853,.T.);
#19648=ORIENTED_EDGE('',*,*,#14831,.F.);
#19649=ORIENTED_EDGE('',*,*,#14827,.F.);
#19650=ORIENTED_EDGE('',*,*,#14832,.F.);
#19651=ORIENTED_EDGE('',*,*,#14853,.F.);
#19652=ORIENTED_EDGE('',*,*,#14854,.T.);
#19653=ORIENTED_EDGE('',*,*,#14855,.T.);
#19654=ORIENTED_EDGE('',*,*,#14856,.T.);
#19655=ORIENTED_EDGE('',*,*,#14857,.T.);
#19656=ORIENTED_EDGE('',*,*,#14837,.T.);
#19657=ORIENTED_EDGE('',*,*,#14854,.F.);
#19658=ORIENTED_EDGE('',*,*,#14858,.T.);
#19659=ORIENTED_EDGE('',*,*,#14857,.F.);
#19660=ORIENTED_EDGE('',*,*,#14859,.T.);
#19661=ORIENTED_EDGE('',*,*,#14858,.F.);
#19662=ORIENTED_EDGE('',*,*,#14836,.F.);
#19663=ORIENTED_EDGE('',*,*,#14789,.F.);
#19664=ORIENTED_EDGE('',*,*,#14860,.T.);
#19665=ORIENTED_EDGE('',*,*,#14861,.T.);
#19666=ORIENTED_EDGE('',*,*,#14840,.F.);
#19667=ORIENTED_EDGE('',*,*,#14862,.F.);
#19668=ORIENTED_EDGE('',*,*,#14838,.F.);
#19669=ORIENTED_EDGE('',*,*,#14863,.F.);
#19670=ORIENTED_EDGE('',*,*,#14864,.T.);
#19671=ORIENTED_EDGE('',*,*,#14855,.F.);
#19672=ORIENTED_EDGE('',*,*,#14859,.F.);
#19673=ORIENTED_EDGE('',*,*,#14856,.F.);
#19674=ORIENTED_EDGE('',*,*,#14864,.F.);
#19675=ORIENTED_EDGE('',*,*,#14865,.T.);
#19676=ORIENTED_EDGE('',*,*,#14866,.T.);
#19677=ORIENTED_EDGE('',*,*,#14867,.T.);
#19678=ORIENTED_EDGE('',*,*,#14834,.T.);
#19679=ORIENTED_EDGE('',*,*,#14865,.F.);
#19680=ORIENTED_EDGE('',*,*,#14868,.T.);
#19681=ORIENTED_EDGE('',*,*,#14867,.F.);
#19682=ORIENTED_EDGE('',*,*,#14869,.T.);
#19683=ORIENTED_EDGE('',*,*,#14870,.T.);
#19684=ORIENTED_EDGE('',*,*,#14871,.F.);
#19685=ORIENTED_EDGE('',*,*,#14872,.T.);
#19686=ORIENTED_EDGE('',*,*,#14869,.F.);
#19687=ORIENTED_EDGE('',*,*,#14866,.F.);
#19688=ORIENTED_EDGE('',*,*,#14870,.F.);
#19689=ORIENTED_EDGE('',*,*,#14872,.F.);
#19690=ORIENTED_EDGE('',*,*,#14873,.T.);
#19691=ORIENTED_EDGE('',*,*,#14874,.T.);
#19692=ORIENTED_EDGE('',*,*,#14875,.T.);
#19693=ORIENTED_EDGE('',*,*,#14876,.T.);
#19694=ORIENTED_EDGE('',*,*,#14839,.T.);
#19695=ORIENTED_EDGE('',*,*,#14873,.F.);
#19696=ORIENTED_EDGE('',*,*,#14862,.T.);
#19697=ORIENTED_EDGE('',*,*,#14876,.F.);
#19698=ORIENTED_EDGE('',*,*,#14877,.T.);
#19699=ORIENTED_EDGE('',*,*,#14878,.F.);
#19700=ORIENTED_EDGE('',*,*,#14879,.T.);
#19701=ORIENTED_EDGE('',*,*,#14874,.F.);
#19702=ORIENTED_EDGE('',*,*,#14877,.F.);
#19703=ORIENTED_EDGE('',*,*,#14875,.F.);
#19704=ORIENTED_EDGE('',*,*,#14879,.F.);
#19705=ORIENTED_EDGE('',*,*,#14880,.T.);
#19706=ORIENTED_EDGE('',*,*,#14881,.T.);
#19707=ORIENTED_EDGE('',*,*,#14878,.T.);
#19708=ORIENTED_EDGE('',*,*,#14881,.F.);
#19709=ORIENTED_EDGE('',*,*,#14882,.F.);
#19710=ORIENTED_EDGE('',*,*,#14883,.T.);
#19711=ORIENTED_EDGE('',*,*,#14884,.T.);
#19712=ORIENTED_EDGE('',*,*,#14885,.F.);
#19713=ORIENTED_EDGE('',*,*,#14886,.T.);
#19714=ORIENTED_EDGE('',*,*,#14887,.F.);
#19715=ORIENTED_EDGE('',*,*,#14888,.T.);
#19716=ORIENTED_EDGE('',*,*,#14889,.F.);
#19717=ORIENTED_EDGE('',*,*,#14890,.F.);
#19718=ORIENTED_EDGE('',*,*,#14891,.F.);
#19719=ORIENTED_EDGE('',*,*,#14892,.F.);
#19720=ORIENTED_EDGE('',*,*,#14893,.F.);
#19721=ORIENTED_EDGE('',*,*,#14894,.F.);
#19722=ORIENTED_EDGE('',*,*,#14895,.F.);
#19723=ORIENTED_EDGE('',*,*,#14896,.F.);
#19724=ORIENTED_EDGE('',*,*,#14897,.F.);
#19725=ORIENTED_EDGE('',*,*,#14898,.F.);
#19726=ORIENTED_EDGE('',*,*,#14899,.F.);
#19727=ORIENTED_EDGE('',*,*,#14900,.F.);
#19728=ORIENTED_EDGE('',*,*,#14880,.F.);
#19729=ORIENTED_EDGE('',*,*,#14890,.T.);
#19730=ORIENTED_EDGE('',*,*,#14901,.T.);
#19731=ORIENTED_EDGE('',*,*,#14871,.T.);
#19732=ORIENTED_EDGE('',*,*,#14901,.F.);
#19733=ORIENTED_EDGE('',*,*,#14900,.T.);
#19734=ORIENTED_EDGE('',*,*,#14902,.T.);
#19735=ORIENTED_EDGE('',*,*,#14863,.T.);
#19736=ORIENTED_EDGE('',*,*,#14902,.F.);
#19737=ORIENTED_EDGE('',*,*,#14891,.T.);
#19738=ORIENTED_EDGE('',*,*,#14903,.T.);
#19739=ORIENTED_EDGE('',*,*,#14852,.T.);
#19740=ORIENTED_EDGE('',*,*,#14903,.F.);
#19741=ORIENTED_EDGE('',*,*,#14904,.T.);
#19742=ORIENTED_EDGE('',*,*,#14905,.T.);
#19743=ORIENTED_EDGE('',*,*,#14906,.T.);
#19744=ORIENTED_EDGE('',*,*,#14905,.F.);
#19745=ORIENTED_EDGE('',*,*,#14907,.F.);
#19746=ORIENTED_EDGE('',*,*,#14908,.F.);
#19747=ORIENTED_EDGE('',*,*,#14909,.F.);
#19748=ORIENTED_EDGE('',*,*,#14910,.F.);
#19749=ORIENTED_EDGE('',*,*,#14911,.F.);
#19750=ORIENTED_EDGE('',*,*,#14904,.F.);
#19751=ORIENTED_EDGE('',*,*,#14912,.F.);
#19752=ORIENTED_EDGE('',*,*,#14913,.T.);
#19753=ORIENTED_EDGE('',*,*,#14906,.F.);
#19754=ORIENTED_EDGE('',*,*,#14913,.F.);
#19755=ORIENTED_EDGE('',*,*,#14908,.T.);
#19756=ORIENTED_EDGE('',*,*,#14914,.T.);
#19757=ORIENTED_EDGE('',*,*,#14915,.T.);
#19758=ORIENTED_EDGE('',*,*,#14914,.F.);
#19759=ORIENTED_EDGE('',*,*,#14916,.F.);
#19760=ORIENTED_EDGE('',*,*,#14917,.T.);
#19761=ORIENTED_EDGE('',*,*,#14915,.F.);
#19762=ORIENTED_EDGE('',*,*,#14917,.F.);
#19763=ORIENTED_EDGE('',*,*,#14911,.T.);
#19764=ORIENTED_EDGE('',*,*,#14918,.T.);
#19765=ORIENTED_EDGE('',*,*,#14919,.T.);
#19766=ORIENTED_EDGE('',*,*,#14918,.F.);
#19767=ORIENTED_EDGE('',*,*,#14920,.F.);
#19768=ORIENTED_EDGE('',*,*,#14921,.T.);
#19769=ORIENTED_EDGE('',*,*,#14919,.F.);
#19770=ORIENTED_EDGE('',*,*,#14921,.F.);
#19771=ORIENTED_EDGE('',*,*,#14909,.T.);
#19772=ORIENTED_EDGE('',*,*,#14922,.T.);
#19773=ORIENTED_EDGE('',*,*,#14923,.T.);
#19774=ORIENTED_EDGE('',*,*,#14922,.F.);
#19775=ORIENTED_EDGE('',*,*,#14924,.F.);
#19776=ORIENTED_EDGE('',*,*,#14925,.T.);
#19777=ORIENTED_EDGE('',*,*,#14923,.F.);
#19778=ORIENTED_EDGE('',*,*,#14925,.F.);
#19779=ORIENTED_EDGE('',*,*,#14926,.T.);
#19780=ORIENTED_EDGE('',*,*,#14927,.T.);
#19781=ORIENTED_EDGE('',*,*,#14825,.T.);
#19782=ORIENTED_EDGE('',*,*,#14927,.F.);
#19783=ORIENTED_EDGE('',*,*,#14928,.F.);
#19784=ORIENTED_EDGE('',*,*,#14929,.F.);
#19785=ORIENTED_EDGE('',*,*,#14930,.F.);
#19786=ORIENTED_EDGE('',*,*,#14931,.F.);
#19787=ORIENTED_EDGE('',*,*,#14932,.F.);
#19788=ORIENTED_EDGE('',*,*,#14933,.F.);
#19789=ORIENTED_EDGE('',*,*,#14934,.F.);
#19790=ORIENTED_EDGE('',*,*,#14935,.F.);
#19791=ORIENTED_EDGE('',*,*,#14936,.F.);
#19792=ORIENTED_EDGE('',*,*,#14926,.F.);
#19793=ORIENTED_EDGE('',*,*,#14936,.T.);
#19794=ORIENTED_EDGE('',*,*,#14937,.T.);
#19795=ORIENTED_EDGE('',*,*,#14821,.T.);
#19796=ORIENTED_EDGE('',*,*,#14937,.F.);
#19797=ORIENTED_EDGE('',*,*,#14938,.T.);
#19798=ORIENTED_EDGE('',*,*,#14939,.T.);
#19799=ORIENTED_EDGE('',*,*,#14940,.T.);
#19800=ORIENTED_EDGE('',*,*,#14939,.F.);
#19801=ORIENTED_EDGE('',*,*,#14938,.F.);
#19802=ORIENTED_EDGE('',*,*,#14941,.T.);
#19803=ORIENTED_EDGE('',*,*,#14942,.F.);
#19804=ORIENTED_EDGE('',*,*,#14941,.F.);
#19805=ORIENTED_EDGE('',*,*,#14940,.F.);
#19806=ORIENTED_EDGE('',*,*,#14943,.T.);
#19807=ORIENTED_EDGE('',*,*,#14944,.T.);
#19808=ORIENTED_EDGE('',*,*,#14945,.T.);
#19809=ORIENTED_EDGE('',*,*,#14946,.T.);
#19810=ORIENTED_EDGE('',*,*,#14947,.F.);
#19811=ORIENTED_EDGE('',*,*,#14942,.T.);
#19812=ORIENTED_EDGE('',*,*,#14948,.T.);
#19813=ORIENTED_EDGE('',*,*,#14949,.T.);
#19814=ORIENTED_EDGE('',*,*,#14948,.F.);
#19815=ORIENTED_EDGE('',*,*,#14949,.F.);
#19816=ORIENTED_EDGE('',*,*,#14950,.T.);
#19817=ORIENTED_EDGE('',*,*,#14951,.T.);
#19818=ORIENTED_EDGE('',*,*,#14952,.T.);
#19819=ORIENTED_EDGE('',*,*,#14953,.T.);
#19820=ORIENTED_EDGE('',*,*,#14954,.T.);
#19821=ORIENTED_EDGE('',*,*,#14955,.T.);
#19822=ORIENTED_EDGE('',*,*,#14956,.T.);
#19823=ORIENTED_EDGE('',*,*,#14957,.T.);
#19824=ORIENTED_EDGE('',*,*,#14956,.F.);
#19825=ORIENTED_EDGE('',*,*,#14957,.F.);
#19826=ORIENTED_EDGE('',*,*,#14958,.T.);
#19827=ORIENTED_EDGE('',*,*,#14959,.F.);
#19828=ORIENTED_EDGE('',*,*,#14958,.F.);
#19829=ORIENTED_EDGE('',*,*,#14960,.F.);
#19830=ORIENTED_EDGE('',*,*,#14961,.T.);
#19831=ORIENTED_EDGE('',*,*,#14955,.F.);
#19832=ORIENTED_EDGE('',*,*,#14961,.F.);
#19833=ORIENTED_EDGE('',*,*,#14959,.T.);
#19834=ORIENTED_EDGE('',*,*,#14962,.T.);
#19835=ORIENTED_EDGE('',*,*,#14963,.T.);
#19836=ORIENTED_EDGE('',*,*,#14962,.F.);
#19837=ORIENTED_EDGE('',*,*,#14963,.F.);
#19838=ORIENTED_EDGE('',*,*,#14964,.T.);
#19839=ORIENTED_EDGE('',*,*,#14965,.T.);
#19840=ORIENTED_EDGE('',*,*,#14966,.T.);
#19841=ORIENTED_EDGE('',*,*,#14967,.F.);
#19842=ORIENTED_EDGE('',*,*,#14968,.T.);
#19843=ORIENTED_EDGE('',*,*,#14888,.F.);
#19844=ORIENTED_EDGE('',*,*,#14969,.F.);
#19845=ORIENTED_EDGE('',*,*,#14884,.F.);
#19846=ORIENTED_EDGE('',*,*,#14970,.T.);
#19847=ORIENTED_EDGE('',*,*,#14971,.F.);
#19848=ORIENTED_EDGE('',*,*,#14972,.F.);
#19849=ORIENTED_EDGE('',*,*,#14973,.F.);
#19850=ORIENTED_EDGE('',*,*,#14974,.T.);
#19851=ORIENTED_EDGE('',*,*,#14975,.F.);
#19852=ORIENTED_EDGE('',*,*,#14976,.F.);
#19853=ORIENTED_EDGE('',*,*,#14977,.F.);
#19854=ORIENTED_EDGE('',*,*,#14978,.T.);
#19855=ORIENTED_EDGE('',*,*,#14979,.F.);
#19856=ORIENTED_EDGE('',*,*,#14980,.T.);
#19857=ORIENTED_EDGE('',*,*,#14981,.T.);
#19858=ORIENTED_EDGE('',*,*,#14964,.F.);
#19859=ORIENTED_EDGE('',*,*,#14982,.T.);
#19860=ORIENTED_EDGE('',*,*,#14983,.T.);
#19861=ORIENTED_EDGE('',*,*,#14984,.T.);
#19862=ORIENTED_EDGE('',*,*,#14976,.T.);
#19863=ORIENTED_EDGE('',*,*,#14983,.F.);
#19864=ORIENTED_EDGE('',*,*,#14985,.F.);
#19865=ORIENTED_EDGE('',*,*,#14986,.T.);
#19866=ORIENTED_EDGE('',*,*,#14987,.T.);
#19867=ORIENTED_EDGE('',*,*,#14988,.T.);
#19868=ORIENTED_EDGE('',*,*,#14972,.T.);
#19869=ORIENTED_EDGE('',*,*,#14987,.F.);
#19870=ORIENTED_EDGE('',*,*,#14989,.F.);
#19871=ORIENTED_EDGE('',*,*,#14887,.T.);
#19872=ORIENTED_EDGE('',*,*,#14990,.T.);
#19873=ORIENTED_EDGE('',*,*,#14885,.T.);
#19874=ORIENTED_EDGE('',*,*,#14969,.T.);
#19875=ORIENTED_EDGE('',*,*,#14990,.F.);
#19876=ORIENTED_EDGE('',*,*,#14886,.F.);
#19877=ORIENTED_EDGE('',*,*,#14991,.T.);
#19878=ORIENTED_EDGE('',*,*,#14928,.T.);
#19879=ORIENTED_EDGE('',*,*,#14992,.T.);
#19880=ORIENTED_EDGE('',*,*,#14993,.T.);
#19881=ORIENTED_EDGE('',*,*,#14994,.T.);
#19882=ORIENTED_EDGE('',*,*,#14995,.T.);
#19883=ORIENTED_EDGE('',*,*,#14992,.F.);
#19884=ORIENTED_EDGE('',*,*,#14935,.T.);
#19885=ORIENTED_EDGE('',*,*,#14996,.T.);
#19886=ORIENTED_EDGE('',*,*,#14997,.T.);
#19887=ORIENTED_EDGE('',*,*,#14994,.F.);
#19888=ORIENTED_EDGE('',*,*,#14934,.T.);
#19889=ORIENTED_EDGE('',*,*,#14998,.T.);
#19890=ORIENTED_EDGE('',*,*,#14999,.T.);
#19891=ORIENTED_EDGE('',*,*,#14996,.F.);
#19892=ORIENTED_EDGE('',*,*,#14933,.T.);
#19893=ORIENTED_EDGE('',*,*,#15000,.T.);
#19894=ORIENTED_EDGE('',*,*,#15001,.T.);
#19895=ORIENTED_EDGE('',*,*,#14998,.F.);
#19896=ORIENTED_EDGE('',*,*,#14932,.T.);
#19897=ORIENTED_EDGE('',*,*,#15002,.T.);
#19898=ORIENTED_EDGE('',*,*,#15003,.T.);
#19899=ORIENTED_EDGE('',*,*,#15000,.F.);
#19900=ORIENTED_EDGE('',*,*,#14931,.T.);
#19901=ORIENTED_EDGE('',*,*,#15004,.T.);
#19902=ORIENTED_EDGE('',*,*,#15005,.T.);
#19903=ORIENTED_EDGE('',*,*,#15002,.F.);
#19904=ORIENTED_EDGE('',*,*,#14930,.T.);
#19905=ORIENTED_EDGE('',*,*,#14991,.F.);
#19906=ORIENTED_EDGE('',*,*,#15006,.T.);
#19907=ORIENTED_EDGE('',*,*,#15004,.F.);
#19908=ORIENTED_EDGE('',*,*,#14929,.T.);
#19909=ORIENTED_EDGE('',*,*,#15003,.F.);
#19910=ORIENTED_EDGE('',*,*,#15007,.T.);
#19911=ORIENTED_EDGE('',*,*,#14805,.F.);
#19912=ORIENTED_EDGE('',*,*,#15008,.F.);
#19913=ORIENTED_EDGE('',*,*,#15005,.F.);
#19914=ORIENTED_EDGE('',*,*,#15009,.T.);
#19915=ORIENTED_EDGE('',*,*,#14808,.F.);
#19916=ORIENTED_EDGE('',*,*,#14806,.F.);
#19917=ORIENTED_EDGE('',*,*,#15007,.F.);
#19918=ORIENTED_EDGE('',*,*,#15006,.F.);
#19919=ORIENTED_EDGE('',*,*,#15010,.T.);
#19920=ORIENTED_EDGE('',*,*,#14809,.F.);
#19921=ORIENTED_EDGE('',*,*,#15009,.F.);
#19922=ORIENTED_EDGE('',*,*,#14993,.F.);
#19923=ORIENTED_EDGE('',*,*,#15011,.T.);
#19924=ORIENTED_EDGE('',*,*,#14810,.F.);
#19925=ORIENTED_EDGE('',*,*,#15010,.F.);
#19926=ORIENTED_EDGE('',*,*,#14907,.T.);
#19927=ORIENTED_EDGE('',*,*,#15012,.T.);
#19928=ORIENTED_EDGE('',*,*,#15013,.T.);
#19929=ORIENTED_EDGE('',*,*,#15012,.F.);
#19930=ORIENTED_EDGE('',*,*,#15013,.F.);
#19931=ORIENTED_EDGE('',*,*,#15014,.T.);
#19932=ORIENTED_EDGE('',*,*,#15015,.F.);
#19933=ORIENTED_EDGE('',*,*,#14960,.T.);
#19934=ORIENTED_EDGE('',*,*,#15015,.T.);
#19935=ORIENTED_EDGE('',*,*,#15014,.F.);
#19936=ORIENTED_EDGE('',*,*,#15016,.T.);
#19937=ORIENTED_EDGE('',*,*,#15017,.T.);
#19938=ORIENTED_EDGE('',*,*,#15018,.T.);
#19939=ORIENTED_EDGE('',*,*,#15017,.F.);
#19940=ORIENTED_EDGE('',*,*,#15019,.T.);
#19941=ORIENTED_EDGE('',*,*,#15020,.T.);
#19942=ORIENTED_EDGE('',*,*,#15021,.T.);
#19943=ORIENTED_EDGE('',*,*,#15020,.F.);
#19944=ORIENTED_EDGE('',*,*,#15022,.F.);
#19945=ORIENTED_EDGE('',*,*,#15023,.F.);
#19946=ORIENTED_EDGE('',*,*,#15024,.F.);
#19947=ORIENTED_EDGE('',*,*,#15019,.F.);
#19948=ORIENTED_EDGE('',*,*,#15025,.F.);
#19949=ORIENTED_EDGE('',*,*,#15026,.F.);
#19950=ORIENTED_EDGE('',*,*,#15027,.F.);
#19951=ORIENTED_EDGE('',*,*,#15016,.F.);
#19952=ORIENTED_EDGE('',*,*,#14841,.F.);
#19953=ORIENTED_EDGE('',*,*,#14861,.F.);
#19954=ORIENTED_EDGE('',*,*,#15028,.F.);
#19955=ORIENTED_EDGE('',*,*,#15021,.F.);
#19956=ORIENTED_EDGE('',*,*,#15029,.F.);
#19957=ORIENTED_EDGE('',*,*,#15030,.F.);
#19958=ORIENTED_EDGE('',*,*,#14842,.F.);
#19959=ORIENTED_EDGE('',*,*,#15031,.F.);
#19960=ORIENTED_EDGE('',*,*,#15032,.T.);
#19961=ORIENTED_EDGE('',*,*,#15018,.F.);
#19962=ORIENTED_EDGE('',*,*,#15032,.F.);
#19963=ORIENTED_EDGE('',*,*,#14910,.T.);
#19964=ORIENTED_EDGE('',*,*,#15033,.T.);
#19965=ORIENTED_EDGE('',*,*,#15034,.T.);
#19966=ORIENTED_EDGE('',*,*,#15035,.T.);
#19967=ORIENTED_EDGE('',*,*,#15033,.F.);
#19968=ORIENTED_EDGE('',*,*,#15036,.F.);
#19969=ORIENTED_EDGE('',*,*,#15037,.T.);
#19970=ORIENTED_EDGE('',*,*,#15034,.F.);
#19971=ORIENTED_EDGE('',*,*,#15035,.F.);
#19972=ORIENTED_EDGE('',*,*,#15037,.F.);
#19973=ORIENTED_EDGE('',*,*,#15031,.T.);
#19974=ORIENTED_EDGE('',*,*,#15038,.T.);
#19975=ORIENTED_EDGE('',*,*,#15039,.T.);
#19976=ORIENTED_EDGE('',*,*,#15038,.F.);
#19977=ORIENTED_EDGE('',*,*,#15036,.T.);
#19978=ORIENTED_EDGE('',*,*,#15039,.F.);
#19979=ORIENTED_EDGE('',*,*,#15040,.T.);
#19980=ORIENTED_EDGE('',*,*,#15041,.T.);
#19981=ORIENTED_EDGE('',*,*,#15042,.T.);
#19982=ORIENTED_EDGE('',*,*,#15043,.T.);
#19983=ORIENTED_EDGE('',*,*,#15044,.T.);
#19984=ORIENTED_EDGE('',*,*,#15045,.T.);
#19985=ORIENTED_EDGE('',*,*,#15042,.F.);
#19986=ORIENTED_EDGE('',*,*,#15046,.T.);
#19987=ORIENTED_EDGE('',*,*,#15047,.T.);
#19988=ORIENTED_EDGE('',*,*,#15048,.T.);
#19989=ORIENTED_EDGE('',*,*,#15044,.F.);
#19990=ORIENTED_EDGE('',*,*,#15049,.T.);
#19991=ORIENTED_EDGE('',*,*,#15050,.T.);
#19992=ORIENTED_EDGE('',*,*,#15051,.T.);
#19993=ORIENTED_EDGE('',*,*,#15047,.F.);
#19994=ORIENTED_EDGE('',*,*,#15052,.T.);
#19995=ORIENTED_EDGE('',*,*,#15053,.T.);
#19996=ORIENTED_EDGE('',*,*,#15054,.T.);
#19997=ORIENTED_EDGE('',*,*,#15050,.F.);
#19998=ORIENTED_EDGE('',*,*,#15055,.T.);
#19999=ORIENTED_EDGE('',*,*,#15056,.T.);
#20000=ORIENTED_EDGE('',*,*,#15057,.T.);
#20001=ORIENTED_EDGE('',*,*,#15053,.F.);
#20002=ORIENTED_EDGE('',*,*,#15058,.T.);
#20003=ORIENTED_EDGE('',*,*,#15059,.T.);
#20004=ORIENTED_EDGE('',*,*,#15060,.T.);
#20005=ORIENTED_EDGE('',*,*,#15056,.F.);
#20006=ORIENTED_EDGE('',*,*,#15061,.T.);
#20007=ORIENTED_EDGE('',*,*,#15040,.F.);
#20008=ORIENTED_EDGE('',*,*,#15062,.T.);
#20009=ORIENTED_EDGE('',*,*,#15059,.F.);
#20010=ORIENTED_EDGE('',*,*,#15063,.T.);
#20011=ORIENTED_EDGE('',*,*,#15052,.F.);
#20012=ORIENTED_EDGE('',*,*,#15064,.T.);
#20013=ORIENTED_EDGE('',*,*,#15065,.F.);
#20014=ORIENTED_EDGE('',*,*,#15066,.F.);
#20015=ORIENTED_EDGE('',*,*,#15049,.F.);
#20016=ORIENTED_EDGE('',*,*,#15067,.T.);
#20017=ORIENTED_EDGE('',*,*,#15068,.F.);
#20018=ORIENTED_EDGE('',*,*,#15064,.F.);
#20019=ORIENTED_EDGE('',*,*,#15046,.F.);
#20020=ORIENTED_EDGE('',*,*,#15069,.T.);
#20021=ORIENTED_EDGE('',*,*,#15070,.F.);
#20022=ORIENTED_EDGE('',*,*,#15067,.F.);
#20023=ORIENTED_EDGE('',*,*,#15041,.F.);
#20024=ORIENTED_EDGE('',*,*,#15071,.T.);
#20025=ORIENTED_EDGE('',*,*,#15072,.F.);
#20026=ORIENTED_EDGE('',*,*,#15069,.F.);
#20027=ORIENTED_EDGE('',*,*,#15073,.F.);
#20028=ORIENTED_EDGE('',*,*,#15074,.T.);
#20029=ORIENTED_EDGE('',*,*,#14977,.T.);
#20030=ORIENTED_EDGE('',*,*,#14984,.F.);
#20031=ORIENTED_EDGE('',*,*,#14985,.T.);
#20032=ORIENTED_EDGE('',*,*,#14982,.F.);
#20033=ORIENTED_EDGE('',*,*,#14975,.T.);
#20034=ORIENTED_EDGE('',*,*,#15075,.F.);
#20035=ORIENTED_EDGE('',*,*,#15043,.F.);
#20036=ORIENTED_EDGE('',*,*,#15045,.F.);
#20037=ORIENTED_EDGE('',*,*,#15048,.F.);
#20038=ORIENTED_EDGE('',*,*,#15051,.F.);
#20039=ORIENTED_EDGE('',*,*,#15054,.F.);
#20040=ORIENTED_EDGE('',*,*,#15057,.F.);
#20041=ORIENTED_EDGE('',*,*,#15060,.F.);
#20042=ORIENTED_EDGE('',*,*,#15062,.F.);
#20043=ORIENTED_EDGE('',*,*,#15076,.T.);
#20044=ORIENTED_EDGE('',*,*,#15072,.T.);
#20045=ORIENTED_EDGE('',*,*,#15077,.T.);
#20046=ORIENTED_EDGE('',*,*,#15078,.T.);
#20047=ORIENTED_EDGE('',*,*,#15079,.T.);
#20048=ORIENTED_EDGE('',*,*,#15080,.T.);
#20049=ORIENTED_EDGE('',*,*,#15077,.F.);
#20050=ORIENTED_EDGE('',*,*,#15081,.T.);
#20051=ORIENTED_EDGE('',*,*,#15082,.T.);
#20052=ORIENTED_EDGE('',*,*,#15083,.T.);
#20053=ORIENTED_EDGE('',*,*,#15079,.F.);
#20054=ORIENTED_EDGE('',*,*,#15084,.T.);
#20055=ORIENTED_EDGE('',*,*,#15085,.T.);
#20056=ORIENTED_EDGE('',*,*,#15086,.T.);
#20057=ORIENTED_EDGE('',*,*,#15082,.F.);
#20058=ORIENTED_EDGE('',*,*,#15087,.T.);
#20059=ORIENTED_EDGE('',*,*,#15088,.T.);
#20060=ORIENTED_EDGE('',*,*,#15089,.T.);
#20061=ORIENTED_EDGE('',*,*,#15085,.F.);
#20062=ORIENTED_EDGE('',*,*,#15090,.T.);
#20063=ORIENTED_EDGE('',*,*,#15091,.T.);
#20064=ORIENTED_EDGE('',*,*,#15092,.T.);
#20065=ORIENTED_EDGE('',*,*,#15088,.F.);
#20066=ORIENTED_EDGE('',*,*,#15065,.T.);
#20067=ORIENTED_EDGE('',*,*,#15093,.T.);
#20068=ORIENTED_EDGE('',*,*,#15094,.T.);
#20069=ORIENTED_EDGE('',*,*,#15091,.F.);
#20070=ORIENTED_EDGE('',*,*,#15068,.T.);
#20071=ORIENTED_EDGE('',*,*,#15076,.F.);
#20072=ORIENTED_EDGE('',*,*,#15095,.T.);
#20073=ORIENTED_EDGE('',*,*,#15093,.F.);
#20074=ORIENTED_EDGE('',*,*,#15070,.T.);
#20075=ORIENTED_EDGE('',*,*,#15058,.F.);
#20076=ORIENTED_EDGE('',*,*,#15096,.T.);
#20077=ORIENTED_EDGE('',*,*,#15087,.F.);
#20078=ORIENTED_EDGE('',*,*,#15097,.F.);
#20079=ORIENTED_EDGE('',*,*,#15061,.F.);
#20080=ORIENTED_EDGE('',*,*,#15097,.T.);
#20081=ORIENTED_EDGE('',*,*,#15084,.F.);
#20082=ORIENTED_EDGE('',*,*,#15098,.F.);
#20083=ORIENTED_EDGE('',*,*,#15063,.F.);
#20084=ORIENTED_EDGE('',*,*,#15098,.T.);
#20085=ORIENTED_EDGE('',*,*,#15081,.F.);
#20086=ORIENTED_EDGE('',*,*,#15071,.F.);
#20087=ORIENTED_EDGE('',*,*,#14794,.T.);
#20088=ORIENTED_EDGE('',*,*,#15099,.T.);
#20089=ORIENTED_EDGE('',*,*,#15022,.T.);
#20090=ORIENTED_EDGE('',*,*,#15027,.T.);
#20091=ORIENTED_EDGE('',*,*,#15100,.F.);
#20092=ORIENTED_EDGE('',*,*,#15078,.F.);
#20093=ORIENTED_EDGE('',*,*,#15080,.F.);
#20094=ORIENTED_EDGE('',*,*,#15083,.F.);
#20095=ORIENTED_EDGE('',*,*,#15086,.F.);
#20096=ORIENTED_EDGE('',*,*,#15089,.F.);
#20097=ORIENTED_EDGE('',*,*,#15092,.F.);
#20098=ORIENTED_EDGE('',*,*,#15094,.F.);
#20099=ORIENTED_EDGE('',*,*,#15095,.F.);
#20100=ORIENTED_EDGE('',*,*,#15101,.T.);
#20101=ORIENTED_EDGE('',*,*,#14882,.T.);
#20102=ORIENTED_EDGE('',*,*,#15102,.T.);
#20103=ORIENTED_EDGE('',*,*,#15103,.T.);
#20104=ORIENTED_EDGE('',*,*,#15104,.T.);
#20105=ORIENTED_EDGE('',*,*,#15105,.T.);
#20106=ORIENTED_EDGE('',*,*,#15102,.F.);
#20107=ORIENTED_EDGE('',*,*,#15106,.T.);
#20108=ORIENTED_EDGE('',*,*,#15107,.T.);
#20109=ORIENTED_EDGE('',*,*,#15108,.T.);
#20110=ORIENTED_EDGE('',*,*,#15104,.F.);
#20111=ORIENTED_EDGE('',*,*,#15109,.T.);
#20112=ORIENTED_EDGE('',*,*,#15110,.T.);
#20113=ORIENTED_EDGE('',*,*,#15111,.T.);
#20114=ORIENTED_EDGE('',*,*,#15107,.F.);
#20115=ORIENTED_EDGE('',*,*,#15112,.T.);
#20116=ORIENTED_EDGE('',*,*,#15113,.T.);
#20117=ORIENTED_EDGE('',*,*,#15114,.T.);
#20118=ORIENTED_EDGE('',*,*,#15110,.F.);
#20119=ORIENTED_EDGE('',*,*,#15073,.T.);
#20120=ORIENTED_EDGE('',*,*,#15115,.T.);
#20121=ORIENTED_EDGE('',*,*,#15116,.T.);
#20122=ORIENTED_EDGE('',*,*,#15113,.F.);
#20123=ORIENTED_EDGE('',*,*,#15117,.T.);
#20124=ORIENTED_EDGE('',*,*,#15118,.T.);
#20125=ORIENTED_EDGE('',*,*,#15119,.T.);
#20126=ORIENTED_EDGE('',*,*,#15115,.F.);
#20127=ORIENTED_EDGE('',*,*,#15120,.T.);
#20128=ORIENTED_EDGE('',*,*,#15118,.F.);
#20129=ORIENTED_EDGE('',*,*,#15121,.T.);
#20130=ORIENTED_EDGE('',*,*,#15101,.F.);
#20131=ORIENTED_EDGE('',*,*,#15122,.T.);
#20132=ORIENTED_EDGE('',*,*,#15112,.F.);
#20133=ORIENTED_EDGE('',*,*,#15123,.T.);
#20134=ORIENTED_EDGE('',*,*,#14978,.F.);
#20135=ORIENTED_EDGE('',*,*,#15074,.F.);
#20136=ORIENTED_EDGE('',*,*,#15109,.F.);
#20137=ORIENTED_EDGE('',*,*,#15124,.T.);
#20138=ORIENTED_EDGE('',*,*,#14967,.T.);
#20139=ORIENTED_EDGE('',*,*,#15125,.T.);
#20140=ORIENTED_EDGE('',*,*,#15126,.T.);
#20141=ORIENTED_EDGE('',*,*,#15127,.T.);
#20142=ORIENTED_EDGE('',*,*,#15128,.T.);
#20143=ORIENTED_EDGE('',*,*,#15129,.T.);
#20144=ORIENTED_EDGE('',*,*,#15130,.T.);
#20145=ORIENTED_EDGE('',*,*,#15131,.T.);
#20146=ORIENTED_EDGE('',*,*,#14979,.T.);
#20147=ORIENTED_EDGE('',*,*,#15123,.F.);
#20148=ORIENTED_EDGE('',*,*,#15106,.F.);
#20149=ORIENTED_EDGE('',*,*,#14889,.T.);
#20150=ORIENTED_EDGE('',*,*,#14968,.F.);
#20151=ORIENTED_EDGE('',*,*,#15124,.F.);
#20152=ORIENTED_EDGE('',*,*,#15103,.F.);
#20153=ORIENTED_EDGE('',*,*,#15105,.F.);
#20154=ORIENTED_EDGE('',*,*,#15108,.F.);
#20155=ORIENTED_EDGE('',*,*,#15111,.F.);
#20156=ORIENTED_EDGE('',*,*,#15114,.F.);
#20157=ORIENTED_EDGE('',*,*,#15116,.F.);
#20158=ORIENTED_EDGE('',*,*,#15119,.F.);
#20159=ORIENTED_EDGE('',*,*,#15122,.F.);
#20160=ORIENTED_EDGE('',*,*,#15132,.F.);
#20161=ORIENTED_EDGE('',*,*,#15133,.T.);
#20162=ORIENTED_EDGE('',*,*,#15134,.T.);
#20163=ORIENTED_EDGE('',*,*,#15135,.T.);
#20164=ORIENTED_EDGE('',*,*,#14892,.T.);
#20165=ORIENTED_EDGE('',*,*,#15136,.T.);
#20166=ORIENTED_EDGE('',*,*,#14893,.T.);
#20167=ORIENTED_EDGE('',*,*,#15135,.F.);
#20168=ORIENTED_EDGE('',*,*,#15137,.T.);
#20169=ORIENTED_EDGE('',*,*,#15138,.T.);
#20170=ORIENTED_EDGE('',*,*,#14894,.T.);
#20171=ORIENTED_EDGE('',*,*,#15136,.F.);
#20172=ORIENTED_EDGE('',*,*,#15139,.T.);
#20173=ORIENTED_EDGE('',*,*,#15140,.T.);
#20174=ORIENTED_EDGE('',*,*,#14895,.T.);
#20175=ORIENTED_EDGE('',*,*,#15138,.F.);
#20176=ORIENTED_EDGE('',*,*,#15141,.T.);
#20177=ORIENTED_EDGE('',*,*,#15142,.T.);
#20178=ORIENTED_EDGE('',*,*,#14896,.T.);
#20179=ORIENTED_EDGE('',*,*,#15140,.F.);
#20180=ORIENTED_EDGE('',*,*,#15143,.T.);
#20181=ORIENTED_EDGE('',*,*,#15144,.T.);
#20182=ORIENTED_EDGE('',*,*,#14897,.T.);
#20183=ORIENTED_EDGE('',*,*,#15142,.F.);
#20184=ORIENTED_EDGE('',*,*,#15145,.T.);
#20185=ORIENTED_EDGE('',*,*,#15146,.T.);
#20186=ORIENTED_EDGE('',*,*,#14898,.T.);
#20187=ORIENTED_EDGE('',*,*,#15144,.F.);
#20188=ORIENTED_EDGE('',*,*,#15147,.T.);
#20189=ORIENTED_EDGE('',*,*,#15133,.F.);
#20190=ORIENTED_EDGE('',*,*,#14899,.T.);
#20191=ORIENTED_EDGE('',*,*,#15146,.F.);
#20192=ORIENTED_EDGE('',*,*,#15148,.T.);
#20193=ORIENTED_EDGE('',*,*,#15141,.F.);
#20194=ORIENTED_EDGE('',*,*,#15149,.T.);
#20195=ORIENTED_EDGE('',*,*,#15150,.F.);
#20196=ORIENTED_EDGE('',*,*,#15151,.F.);
#20197=ORIENTED_EDGE('',*,*,#15139,.F.);
#20198=ORIENTED_EDGE('',*,*,#15152,.T.);
#20199=ORIENTED_EDGE('',*,*,#15153,.F.);
#20200=ORIENTED_EDGE('',*,*,#15149,.F.);
#20201=ORIENTED_EDGE('',*,*,#15137,.F.);
#20202=ORIENTED_EDGE('',*,*,#15154,.T.);
#20203=ORIENTED_EDGE('',*,*,#15155,.F.);
#20204=ORIENTED_EDGE('',*,*,#15152,.F.);
#20205=ORIENTED_EDGE('',*,*,#15134,.F.);
#20206=ORIENTED_EDGE('',*,*,#15156,.T.);
#20207=ORIENTED_EDGE('',*,*,#15157,.F.);
#20208=ORIENTED_EDGE('',*,*,#15154,.F.);
#20209=ORIENTED_EDGE('',*,*,#15158,.T.);
#20210=ORIENTED_EDGE('',*,*,#15157,.T.);
#20211=ORIENTED_EDGE('',*,*,#15159,.T.);
#20212=ORIENTED_EDGE('',*,*,#14844,.T.);
#20213=ORIENTED_EDGE('',*,*,#15160,.T.);
#20214=ORIENTED_EDGE('',*,*,#14845,.T.);
#20215=ORIENTED_EDGE('',*,*,#15159,.F.);
#20216=ORIENTED_EDGE('',*,*,#15161,.T.);
#20217=ORIENTED_EDGE('',*,*,#15162,.T.);
#20218=ORIENTED_EDGE('',*,*,#14846,.T.);
#20219=ORIENTED_EDGE('',*,*,#15160,.F.);
#20220=ORIENTED_EDGE('',*,*,#15163,.T.);
#20221=ORIENTED_EDGE('',*,*,#15164,.T.);
#20222=ORIENTED_EDGE('',*,*,#14847,.T.);
#20223=ORIENTED_EDGE('',*,*,#15162,.F.);
#20224=ORIENTED_EDGE('',*,*,#15165,.T.);
#20225=ORIENTED_EDGE('',*,*,#15166,.T.);
#20226=ORIENTED_EDGE('',*,*,#14848,.T.);
#20227=ORIENTED_EDGE('',*,*,#15164,.F.);
#20228=ORIENTED_EDGE('',*,*,#15167,.T.);
#20229=ORIENTED_EDGE('',*,*,#15168,.T.);
#20230=ORIENTED_EDGE('',*,*,#14849,.T.);
#20231=ORIENTED_EDGE('',*,*,#15166,.F.);
#20232=ORIENTED_EDGE('',*,*,#15150,.T.);
#20233=ORIENTED_EDGE('',*,*,#15169,.T.);
#20234=ORIENTED_EDGE('',*,*,#14850,.T.);
#20235=ORIENTED_EDGE('',*,*,#15168,.F.);
#20236=ORIENTED_EDGE('',*,*,#15153,.T.);
#20237=ORIENTED_EDGE('',*,*,#15158,.F.);
#20238=ORIENTED_EDGE('',*,*,#14851,.T.);
#20239=ORIENTED_EDGE('',*,*,#15169,.F.);
#20240=ORIENTED_EDGE('',*,*,#15155,.T.);
#20241=ORIENTED_EDGE('',*,*,#15145,.F.);
#20242=ORIENTED_EDGE('',*,*,#15170,.T.);
#20243=ORIENTED_EDGE('',*,*,#15165,.F.);
#20244=ORIENTED_EDGE('',*,*,#15171,.F.);
#20245=ORIENTED_EDGE('',*,*,#15147,.F.);
#20246=ORIENTED_EDGE('',*,*,#15171,.T.);
#20247=ORIENTED_EDGE('',*,*,#15163,.F.);
#20248=ORIENTED_EDGE('',*,*,#15172,.F.);
#20249=ORIENTED_EDGE('',*,*,#15148,.F.);
#20250=ORIENTED_EDGE('',*,*,#15172,.T.);
#20251=ORIENTED_EDGE('',*,*,#15161,.F.);
#20252=ORIENTED_EDGE('',*,*,#15156,.F.);
#20253=ORIENTED_EDGE('',*,*,#14912,.T.);
#20254=ORIENTED_EDGE('',*,*,#14916,.T.);
#20255=ORIENTED_EDGE('',*,*,#14920,.T.);
#20256=ORIENTED_EDGE('',*,*,#14924,.T.);
#20257=ORIENTED_EDGE('',*,*,#14943,.F.);
#20258=ORIENTED_EDGE('',*,*,#15173,.T.);
#20259=ORIENTED_EDGE('',*,*,#14954,.F.);
#20260=ORIENTED_EDGE('',*,*,#15173,.F.);
#20261=ORIENTED_EDGE('',*,*,#14944,.F.);
#20262=ORIENTED_EDGE('',*,*,#15174,.T.);
#20263=ORIENTED_EDGE('',*,*,#14953,.F.);
#20264=ORIENTED_EDGE('',*,*,#15174,.F.);
#20265=ORIENTED_EDGE('',*,*,#14945,.F.);
#20266=ORIENTED_EDGE('',*,*,#15175,.T.);
#20267=ORIENTED_EDGE('',*,*,#14952,.F.);
#20268=ORIENTED_EDGE('',*,*,#15175,.F.);
#20269=ORIENTED_EDGE('',*,*,#14946,.F.);
#20270=ORIENTED_EDGE('',*,*,#15176,.T.);
#20271=ORIENTED_EDGE('',*,*,#14951,.F.);
#20272=ORIENTED_EDGE('',*,*,#15176,.F.);
#20273=ORIENTED_EDGE('',*,*,#15143,.F.);
#20274=ORIENTED_EDGE('',*,*,#15151,.T.);
#20275=ORIENTED_EDGE('',*,*,#15167,.F.);
#20276=ORIENTED_EDGE('',*,*,#15170,.F.);
#20277=ORIENTED_EDGE('',*,*,#15055,.F.);
#20278=ORIENTED_EDGE('',*,*,#15066,.T.);
#20279=ORIENTED_EDGE('',*,*,#15090,.F.);
#20280=ORIENTED_EDGE('',*,*,#15096,.F.);
#20281=ORIENTED_EDGE('',*,*,#15177,.T.);
#20282=ORIENTED_EDGE('',*,*,#15178,.F.);
#20283=ORIENTED_EDGE('',*,*,#15177,.F.);
#20284=ORIENTED_EDGE('',*,*,#15179,.T.);
#20285=ORIENTED_EDGE('',*,*,#14797,.T.);
#20286=ORIENTED_EDGE('',*,*,#15179,.F.);
#20287=ORIENTED_EDGE('',*,*,#15180,.T.);
#20288=ORIENTED_EDGE('',*,*,#15181,.F.);
#20289=ORIENTED_EDGE('',*,*,#15180,.F.);
#20290=ORIENTED_EDGE('',*,*,#15182,.T.);
#20291=ORIENTED_EDGE('',*,*,#15178,.T.);
#20292=ORIENTED_EDGE('',*,*,#15182,.F.);
#20293=ORIENTED_EDGE('',*,*,#14793,.F.);
#20294=ORIENTED_EDGE('',*,*,#15183,.T.);
#20295=ORIENTED_EDGE('',*,*,#15023,.T.);
#20296=ORIENTED_EDGE('',*,*,#15099,.F.);
#20297=ORIENTED_EDGE('',*,*,#14792,.T.);
#20298=ORIENTED_EDGE('',*,*,#15184,.T.);
#20299=ORIENTED_EDGE('',*,*,#15029,.T.);
#20300=ORIENTED_EDGE('',*,*,#15024,.T.);
#20301=ORIENTED_EDGE('',*,*,#15183,.F.);
#20302=ORIENTED_EDGE('',*,*,#14830,.F.);
#20303=ORIENTED_EDGE('',*,*,#14843,.T.);
#20304=ORIENTED_EDGE('',*,*,#15030,.T.);
#20305=ORIENTED_EDGE('',*,*,#15184,.F.);
#20306=ORIENTED_EDGE('',*,*,#14791,.F.);
#20307=ORIENTED_EDGE('',*,*,#14835,.T.);
#20308=ORIENTED_EDGE('',*,*,#14868,.F.);
#20309=ORIENTED_EDGE('',*,*,#14833,.T.);
#20310=ORIENTED_EDGE('',*,*,#14788,.T.);
#20311=ORIENTED_EDGE('',*,*,#15185,.T.);
#20312=ORIENTED_EDGE('',*,*,#15025,.T.);
#20313=ORIENTED_EDGE('',*,*,#15028,.T.);
#20314=ORIENTED_EDGE('',*,*,#14860,.F.);
#20315=ORIENTED_EDGE('',*,*,#14787,.F.);
#20316=ORIENTED_EDGE('',*,*,#15100,.T.);
#20317=ORIENTED_EDGE('',*,*,#15026,.T.);
#20318=ORIENTED_EDGE('',*,*,#15185,.F.);
#20319=ORIENTED_EDGE('',*,*,#15001,.F.);
#20320=ORIENTED_EDGE('',*,*,#15008,.T.);
#20321=ORIENTED_EDGE('',*,*,#14804,.F.);
#20322=ORIENTED_EDGE('',*,*,#15186,.F.);
#20323=ORIENTED_EDGE('',*,*,#14999,.F.);
#20324=ORIENTED_EDGE('',*,*,#15186,.T.);
#20325=ORIENTED_EDGE('',*,*,#14803,.F.);
#20326=ORIENTED_EDGE('',*,*,#15187,.F.);
#20327=ORIENTED_EDGE('',*,*,#14997,.F.);
#20328=ORIENTED_EDGE('',*,*,#15187,.T.);
#20329=ORIENTED_EDGE('',*,*,#14802,.F.);
#20330=ORIENTED_EDGE('',*,*,#15188,.F.);
#20331=ORIENTED_EDGE('',*,*,#14995,.F.);
#20332=ORIENTED_EDGE('',*,*,#15188,.T.);
#20333=ORIENTED_EDGE('',*,*,#14801,.F.);
#20334=ORIENTED_EDGE('',*,*,#15011,.F.);
#20335=ORIENTED_EDGE('',*,*,#15128,.F.);
#20336=ORIENTED_EDGE('',*,*,#15189,.F.);
#20337=ORIENTED_EDGE('',*,*,#14812,.T.);
#20338=ORIENTED_EDGE('',*,*,#15190,.T.);
#20339=ORIENTED_EDGE('',*,*,#15127,.F.);
#20340=ORIENTED_EDGE('',*,*,#15191,.F.);
#20341=ORIENTED_EDGE('',*,*,#14813,.T.);
#20342=ORIENTED_EDGE('',*,*,#15189,.T.);
#20343=ORIENTED_EDGE('',*,*,#15126,.F.);
#20344=ORIENTED_EDGE('',*,*,#15192,.F.);
#20345=ORIENTED_EDGE('',*,*,#14814,.T.);
#20346=ORIENTED_EDGE('',*,*,#15191,.T.);
#20347=ORIENTED_EDGE('',*,*,#15125,.F.);
#20348=ORIENTED_EDGE('',*,*,#14966,.F.);
#20349=ORIENTED_EDGE('',*,*,#15193,.F.);
#20350=ORIENTED_EDGE('',*,*,#14815,.T.);
#20351=ORIENTED_EDGE('',*,*,#15192,.T.);
#20352=ORIENTED_EDGE('',*,*,#14981,.F.);
#20353=ORIENTED_EDGE('',*,*,#15194,.F.);
#20354=ORIENTED_EDGE('',*,*,#14816,.T.);
#20355=ORIENTED_EDGE('',*,*,#15193,.T.);
#20356=ORIENTED_EDGE('',*,*,#14965,.F.);
#20357=ORIENTED_EDGE('',*,*,#15131,.F.);
#20358=ORIENTED_EDGE('',*,*,#15195,.F.);
#20359=ORIENTED_EDGE('',*,*,#14817,.T.);
#20360=ORIENTED_EDGE('',*,*,#15194,.T.);
#20361=ORIENTED_EDGE('',*,*,#14980,.F.);
#20362=ORIENTED_EDGE('',*,*,#15130,.F.);
#20363=ORIENTED_EDGE('',*,*,#15196,.F.);
#20364=ORIENTED_EDGE('',*,*,#14818,.T.);
#20365=ORIENTED_EDGE('',*,*,#15195,.T.);
#20366=ORIENTED_EDGE('',*,*,#15129,.F.);
#20367=ORIENTED_EDGE('',*,*,#15190,.F.);
#20368=ORIENTED_EDGE('',*,*,#14819,.T.);
#20369=ORIENTED_EDGE('',*,*,#15196,.T.);
#20370=ORIENTED_EDGE('',*,*,#15120,.F.);
#20371=ORIENTED_EDGE('',*,*,#15197,.T.);
#20372=ORIENTED_EDGE('',*,*,#14973,.T.);
#20373=ORIENTED_EDGE('',*,*,#14988,.F.);
#20374=ORIENTED_EDGE('',*,*,#14989,.T.);
#20375=ORIENTED_EDGE('',*,*,#14986,.F.);
#20376=ORIENTED_EDGE('',*,*,#14971,.T.);
#20377=ORIENTED_EDGE('',*,*,#15198,.F.);
#20378=ORIENTED_EDGE('',*,*,#15121,.F.);
#20379=ORIENTED_EDGE('',*,*,#15198,.T.);
#20380=ORIENTED_EDGE('',*,*,#14970,.F.);
#20381=ORIENTED_EDGE('',*,*,#14883,.F.);
#20382=ORIENTED_EDGE('',*,*,#15117,.F.);
#20383=ORIENTED_EDGE('',*,*,#15075,.T.);
#20384=ORIENTED_EDGE('',*,*,#14974,.F.);
#20385=ORIENTED_EDGE('',*,*,#15197,.F.);
#20386=ORIENTED_EDGE('',*,*,#15181,.T.);
#20387=ORIENTED_EDGE('',*,*,#15199,.T.);
#20388=ORIENTED_EDGE('',*,*,#14950,.F.);
#20389=ORIENTED_EDGE('',*,*,#15199,.F.);
#20390=ORIENTED_EDGE('',*,*,#15132,.T.);
#20391=ORIENTED_EDGE('',*,*,#15200,.T.);
#20392=ORIENTED_EDGE('',*,*,#14947,.T.);
#20393=ORIENTED_EDGE('',*,*,#15200,.F.);
#20394=ORIENTED_EDGE('',*,*,#15201,.T.);
#20395=ORIENTED_EDGE('',*,*,#15202,.T.);
#20396=ORIENTED_EDGE('',*,*,#15203,.T.);
#20397=ORIENTED_EDGE('',*,*,#15204,.T.);
#20398=ORIENTED_EDGE('',*,*,#15202,.F.);
#20399=ORIENTED_EDGE('',*,*,#15205,.F.);
#20400=ORIENTED_EDGE('',*,*,#15206,.T.);
#20401=ORIENTED_EDGE('',*,*,#15207,.F.);
#20402=ORIENTED_EDGE('',*,*,#15201,.F.);
#20403=ORIENTED_EDGE('',*,*,#15208,.F.);
#20404=ORIENTED_EDGE('',*,*,#15209,.F.);
#20405=ORIENTED_EDGE('',*,*,#15210,.T.);
#20406=ORIENTED_EDGE('',*,*,#15211,.T.);
#20407=ORIENTED_EDGE('',*,*,#15212,.T.);
#20408=ORIENTED_EDGE('',*,*,#15213,.F.);
#20409=ORIENTED_EDGE('',*,*,#15214,.F.);
#20410=ORIENTED_EDGE('',*,*,#15215,.F.);
#20411=ORIENTED_EDGE('',*,*,#15216,.T.);
#20412=ORIENTED_EDGE('',*,*,#15217,.T.);
#20413=ORIENTED_EDGE('',*,*,#15218,.T.);
#20414=ORIENTED_EDGE('',*,*,#15219,.F.);
#20415=ORIENTED_EDGE('',*,*,#15220,.F.);
#20416=ORIENTED_EDGE('',*,*,#15221,.T.);
#20417=ORIENTED_EDGE('',*,*,#15222,.T.);
#20418=ORIENTED_EDGE('',*,*,#15223,.F.);
#20419=ORIENTED_EDGE('',*,*,#15224,.T.);
#20420=ORIENTED_EDGE('',*,*,#15225,.T.);
#20421=ORIENTED_EDGE('',*,*,#15226,.T.);
#20422=ORIENTED_EDGE('',*,*,#15227,.F.);
#20423=ORIENTED_EDGE('',*,*,#15228,.T.);
#20424=ORIENTED_EDGE('',*,*,#15229,.F.);
#20425=ORIENTED_EDGE('',*,*,#15230,.T.);
#20426=ORIENTED_EDGE('',*,*,#15231,.T.);
#20427=ORIENTED_EDGE('',*,*,#15232,.T.);
#20428=ORIENTED_EDGE('',*,*,#15233,.F.);
#20429=ORIENTED_EDGE('',*,*,#15234,.T.);
#20430=ORIENTED_EDGE('',*,*,#15235,.F.);
#20431=ORIENTED_EDGE('',*,*,#15236,.T.);
#20432=ORIENTED_EDGE('',*,*,#15237,.T.);
#20433=ORIENTED_EDGE('',*,*,#15238,.T.);
#20434=ORIENTED_EDGE('',*,*,#15239,.F.);
#20435=ORIENTED_EDGE('',*,*,#15240,.T.);
#20436=ORIENTED_EDGE('',*,*,#15241,.F.);
#20437=ORIENTED_EDGE('',*,*,#15242,.T.);
#20438=ORIENTED_EDGE('',*,*,#15243,.T.);
#20439=ORIENTED_EDGE('',*,*,#15244,.T.);
#20440=ORIENTED_EDGE('',*,*,#15245,.F.);
#20441=ORIENTED_EDGE('',*,*,#15246,.T.);
#20442=ORIENTED_EDGE('',*,*,#15247,.F.);
#20443=ORIENTED_EDGE('',*,*,#15248,.T.);
#20444=ORIENTED_EDGE('',*,*,#15249,.T.);
#20445=ORIENTED_EDGE('',*,*,#15250,.T.);
#20446=ORIENTED_EDGE('',*,*,#15251,.F.);
#20447=ORIENTED_EDGE('',*,*,#15252,.T.);
#20448=ORIENTED_EDGE('',*,*,#15253,.F.);
#20449=ORIENTED_EDGE('',*,*,#15254,.T.);
#20450=ORIENTED_EDGE('',*,*,#15255,.T.);
#20451=ORIENTED_EDGE('',*,*,#15256,.T.);
#20452=ORIENTED_EDGE('',*,*,#15257,.F.);
#20453=ORIENTED_EDGE('',*,*,#15258,.T.);
#20454=ORIENTED_EDGE('',*,*,#15259,.F.);
#20455=ORIENTED_EDGE('',*,*,#15260,.T.);
#20456=ORIENTED_EDGE('',*,*,#15261,.T.);
#20457=ORIENTED_EDGE('',*,*,#15262,.T.);
#20458=ORIENTED_EDGE('',*,*,#15263,.F.);
#20459=ORIENTED_EDGE('',*,*,#15264,.T.);
#20460=ORIENTED_EDGE('',*,*,#15265,.F.);
#20461=ORIENTED_EDGE('',*,*,#15266,.T.);
#20462=ORIENTED_EDGE('',*,*,#15267,.T.);
#20463=ORIENTED_EDGE('',*,*,#15268,.T.);
#20464=ORIENTED_EDGE('',*,*,#15269,.F.);
#20465=ORIENTED_EDGE('',*,*,#15270,.T.);
#20466=ORIENTED_EDGE('',*,*,#15271,.F.);
#20467=ORIENTED_EDGE('',*,*,#15272,.T.);
#20468=ORIENTED_EDGE('',*,*,#15273,.T.);
#20469=ORIENTED_EDGE('',*,*,#15274,.T.);
#20470=ORIENTED_EDGE('',*,*,#15275,.F.);
#20471=ORIENTED_EDGE('',*,*,#15276,.T.);
#20472=ORIENTED_EDGE('',*,*,#15277,.F.);
#20473=ORIENTED_EDGE('',*,*,#15278,.T.);
#20474=ORIENTED_EDGE('',*,*,#15279,.T.);
#20475=ORIENTED_EDGE('',*,*,#15280,.T.);
#20476=ORIENTED_EDGE('',*,*,#15281,.F.);
#20477=ORIENTED_EDGE('',*,*,#15282,.T.);
#20478=ORIENTED_EDGE('',*,*,#15283,.F.);
#20479=ORIENTED_EDGE('',*,*,#15284,.T.);
#20480=ORIENTED_EDGE('',*,*,#15285,.T.);
#20481=ORIENTED_EDGE('',*,*,#15286,.T.);
#20482=ORIENTED_EDGE('',*,*,#15287,.F.);
#20483=ORIENTED_EDGE('',*,*,#15288,.T.);
#20484=ORIENTED_EDGE('',*,*,#15289,.F.);
#20485=ORIENTED_EDGE('',*,*,#15290,.T.);
#20486=ORIENTED_EDGE('',*,*,#15291,.T.);
#20487=ORIENTED_EDGE('',*,*,#15292,.T.);
#20488=ORIENTED_EDGE('',*,*,#15293,.F.);
#20489=ORIENTED_EDGE('',*,*,#15294,.T.);
#20490=ORIENTED_EDGE('',*,*,#15295,.F.);
#20491=ORIENTED_EDGE('',*,*,#15296,.T.);
#20492=ORIENTED_EDGE('',*,*,#15297,.T.);
#20493=ORIENTED_EDGE('',*,*,#15298,.T.);
#20494=ORIENTED_EDGE('',*,*,#15299,.F.);
#20495=ORIENTED_EDGE('',*,*,#15300,.T.);
#20496=ORIENTED_EDGE('',*,*,#15301,.F.);
#20497=ORIENTED_EDGE('',*,*,#15302,.T.);
#20498=ORIENTED_EDGE('',*,*,#15303,.T.);
#20499=ORIENTED_EDGE('',*,*,#15304,.T.);
#20500=ORIENTED_EDGE('',*,*,#15305,.F.);
#20501=ORIENTED_EDGE('',*,*,#15306,.T.);
#20502=ORIENTED_EDGE('',*,*,#15307,.F.);
#20503=ORIENTED_EDGE('',*,*,#15308,.T.);
#20504=ORIENTED_EDGE('',*,*,#15309,.T.);
#20505=ORIENTED_EDGE('',*,*,#15310,.T.);
#20506=ORIENTED_EDGE('',*,*,#15311,.F.);
#20507=ORIENTED_EDGE('',*,*,#15312,.T.);
#20508=ORIENTED_EDGE('',*,*,#15313,.F.);
#20509=ORIENTED_EDGE('',*,*,#15314,.T.);
#20510=ORIENTED_EDGE('',*,*,#15315,.T.);
#20511=ORIENTED_EDGE('',*,*,#15316,.T.);
#20512=ORIENTED_EDGE('',*,*,#15317,.F.);
#20513=ORIENTED_EDGE('',*,*,#15318,.T.);
#20514=ORIENTED_EDGE('',*,*,#15319,.F.);
#20515=ORIENTED_EDGE('',*,*,#15320,.T.);
#20516=ORIENTED_EDGE('',*,*,#15321,.T.);
#20517=ORIENTED_EDGE('',*,*,#15322,.T.);
#20518=ORIENTED_EDGE('',*,*,#15323,.F.);
#20519=ORIENTED_EDGE('',*,*,#15324,.T.);
#20520=ORIENTED_EDGE('',*,*,#15325,.F.);
#20521=ORIENTED_EDGE('',*,*,#15326,.T.);
#20522=ORIENTED_EDGE('',*,*,#15327,.T.);
#20523=ORIENTED_EDGE('',*,*,#15328,.T.);
#20524=ORIENTED_EDGE('',*,*,#15329,.F.);
#20525=ORIENTED_EDGE('',*,*,#15330,.T.);
#20526=ORIENTED_EDGE('',*,*,#15331,.F.);
#20527=ORIENTED_EDGE('',*,*,#15332,.T.);
#20528=ORIENTED_EDGE('',*,*,#15333,.T.);
#20529=ORIENTED_EDGE('',*,*,#15334,.T.);
#20530=ORIENTED_EDGE('',*,*,#15335,.F.);
#20531=ORIENTED_EDGE('',*,*,#15336,.T.);
#20532=ORIENTED_EDGE('',*,*,#15337,.F.);
#20533=ORIENTED_EDGE('',*,*,#15338,.T.);
#20534=ORIENTED_EDGE('',*,*,#15339,.T.);
#20535=ORIENTED_EDGE('',*,*,#15340,.T.);
#20536=ORIENTED_EDGE('',*,*,#15341,.F.);
#20537=ORIENTED_EDGE('',*,*,#15342,.T.);
#20538=ORIENTED_EDGE('',*,*,#15343,.F.);
#20539=ORIENTED_EDGE('',*,*,#15344,.T.);
#20540=ORIENTED_EDGE('',*,*,#15345,.T.);
#20541=ORIENTED_EDGE('',*,*,#15346,.T.);
#20542=ORIENTED_EDGE('',*,*,#15347,.F.);
#20543=ORIENTED_EDGE('',*,*,#15348,.T.);
#20544=ORIENTED_EDGE('',*,*,#15349,.F.);
#20545=ORIENTED_EDGE('',*,*,#15350,.T.);
#20546=ORIENTED_EDGE('',*,*,#15351,.T.);
#20547=ORIENTED_EDGE('',*,*,#15352,.T.);
#20548=ORIENTED_EDGE('',*,*,#15353,.F.);
#20549=ORIENTED_EDGE('',*,*,#15354,.T.);
#20550=ORIENTED_EDGE('',*,*,#15355,.F.);
#20551=ORIENTED_EDGE('',*,*,#15356,.T.);
#20552=ORIENTED_EDGE('',*,*,#15357,.T.);
#20553=ORIENTED_EDGE('',*,*,#15358,.T.);
#20554=ORIENTED_EDGE('',*,*,#15359,.F.);
#20555=ORIENTED_EDGE('',*,*,#15360,.T.);
#20556=ORIENTED_EDGE('',*,*,#15361,.F.);
#20557=ORIENTED_EDGE('',*,*,#15362,.T.);
#20558=ORIENTED_EDGE('',*,*,#15363,.T.);
#20559=ORIENTED_EDGE('',*,*,#15364,.T.);
#20560=ORIENTED_EDGE('',*,*,#15365,.F.);
#20561=ORIENTED_EDGE('',*,*,#15366,.T.);
#20562=ORIENTED_EDGE('',*,*,#15367,.F.);
#20563=ORIENTED_EDGE('',*,*,#15368,.T.);
#20564=ORIENTED_EDGE('',*,*,#15369,.T.);
#20565=ORIENTED_EDGE('',*,*,#15370,.T.);
#20566=ORIENTED_EDGE('',*,*,#15371,.F.);
#20567=ORIENTED_EDGE('',*,*,#15372,.T.);
#20568=ORIENTED_EDGE('',*,*,#15373,.F.);
#20569=ORIENTED_EDGE('',*,*,#15374,.T.);
#20570=ORIENTED_EDGE('',*,*,#15375,.T.);
#20571=ORIENTED_EDGE('',*,*,#15376,.T.);
#20572=ORIENTED_EDGE('',*,*,#15377,.F.);
#20573=ORIENTED_EDGE('',*,*,#15378,.T.);
#20574=ORIENTED_EDGE('',*,*,#15379,.F.);
#20575=ORIENTED_EDGE('',*,*,#15380,.T.);
#20576=ORIENTED_EDGE('',*,*,#15381,.T.);
#20577=ORIENTED_EDGE('',*,*,#15382,.T.);
#20578=ORIENTED_EDGE('',*,*,#15383,.F.);
#20579=ORIENTED_EDGE('',*,*,#15384,.T.);
#20580=ORIENTED_EDGE('',*,*,#15385,.F.);
#20581=ORIENTED_EDGE('',*,*,#15386,.T.);
#20582=ORIENTED_EDGE('',*,*,#15387,.T.);
#20583=ORIENTED_EDGE('',*,*,#15388,.T.);
#20584=ORIENTED_EDGE('',*,*,#15389,.F.);
#20585=ORIENTED_EDGE('',*,*,#15390,.T.);
#20586=ORIENTED_EDGE('',*,*,#15391,.F.);
#20587=ORIENTED_EDGE('',*,*,#15392,.T.);
#20588=ORIENTED_EDGE('',*,*,#15393,.T.);
#20589=ORIENTED_EDGE('',*,*,#15394,.T.);
#20590=ORIENTED_EDGE('',*,*,#15395,.F.);
#20591=ORIENTED_EDGE('',*,*,#15396,.T.);
#20592=ORIENTED_EDGE('',*,*,#15397,.F.);
#20593=ORIENTED_EDGE('',*,*,#15398,.T.);
#20594=ORIENTED_EDGE('',*,*,#15399,.T.);
#20595=ORIENTED_EDGE('',*,*,#15400,.T.);
#20596=ORIENTED_EDGE('',*,*,#15401,.F.);
#20597=ORIENTED_EDGE('',*,*,#15402,.T.);
#20598=ORIENTED_EDGE('',*,*,#15221,.F.);
#20599=ORIENTED_EDGE('',*,*,#15403,.F.);
#20600=ORIENTED_EDGE('',*,*,#15404,.F.);
#20601=ORIENTED_EDGE('',*,*,#15405,.T.);
#20602=ORIENTED_EDGE('',*,*,#15406,.T.);
#20603=ORIENTED_EDGE('',*,*,#15407,.T.);
#20604=ORIENTED_EDGE('',*,*,#15408,.F.);
#20605=ORIENTED_EDGE('',*,*,#15409,.F.);
#20606=ORIENTED_EDGE('',*,*,#15410,.F.);
#20607=ORIENTED_EDGE('',*,*,#15411,.T.);
#20608=ORIENTED_EDGE('',*,*,#15412,.T.);
#20609=ORIENTED_EDGE('',*,*,#15413,.T.);
#20610=ORIENTED_EDGE('',*,*,#15414,.F.);
#20611=ORIENTED_EDGE('',*,*,#15415,.F.);
#20612=ORIENTED_EDGE('',*,*,#15416,.F.);
#20613=ORIENTED_EDGE('',*,*,#15417,.T.);
#20614=ORIENTED_EDGE('',*,*,#15418,.T.);
#20615=ORIENTED_EDGE('',*,*,#15419,.T.);
#20616=ORIENTED_EDGE('',*,*,#15420,.F.);
#20617=ORIENTED_EDGE('',*,*,#15421,.F.);
#20618=ORIENTED_EDGE('',*,*,#15422,.F.);
#20619=ORIENTED_EDGE('',*,*,#15423,.T.);
#20620=ORIENTED_EDGE('',*,*,#15424,.T.);
#20621=ORIENTED_EDGE('',*,*,#15425,.T.);
#20622=ORIENTED_EDGE('',*,*,#15426,.F.);
#20623=ORIENTED_EDGE('',*,*,#15427,.F.);
#20624=ORIENTED_EDGE('',*,*,#15428,.F.);
#20625=ORIENTED_EDGE('',*,*,#15429,.T.);
#20626=ORIENTED_EDGE('',*,*,#15430,.T.);
#20627=ORIENTED_EDGE('',*,*,#15431,.T.);
#20628=ORIENTED_EDGE('',*,*,#15432,.F.);
#20629=ORIENTED_EDGE('',*,*,#15433,.F.);
#20630=ORIENTED_EDGE('',*,*,#15434,.F.);
#20631=ORIENTED_EDGE('',*,*,#15435,.T.);
#20632=ORIENTED_EDGE('',*,*,#15436,.T.);
#20633=ORIENTED_EDGE('',*,*,#15437,.T.);
#20634=ORIENTED_EDGE('',*,*,#15438,.F.);
#20635=ORIENTED_EDGE('',*,*,#15439,.F.);
#20636=ORIENTED_EDGE('',*,*,#15440,.F.);
#20637=ORIENTED_EDGE('',*,*,#15441,.T.);
#20638=ORIENTED_EDGE('',*,*,#15442,.T.);
#20639=ORIENTED_EDGE('',*,*,#15443,.T.);
#20640=ORIENTED_EDGE('',*,*,#15444,.F.);
#20641=ORIENTED_EDGE('',*,*,#15445,.F.);
#20642=ORIENTED_EDGE('',*,*,#15446,.F.);
#20643=ORIENTED_EDGE('',*,*,#15447,.T.);
#20644=ORIENTED_EDGE('',*,*,#15448,.T.);
#20645=ORIENTED_EDGE('',*,*,#15449,.T.);
#20646=ORIENTED_EDGE('',*,*,#15450,.F.);
#20647=ORIENTED_EDGE('',*,*,#15451,.F.);
#20648=ORIENTED_EDGE('',*,*,#15452,.F.);
#20649=ORIENTED_EDGE('',*,*,#15453,.T.);
#20650=ORIENTED_EDGE('',*,*,#15454,.T.);
#20651=ORIENTED_EDGE('',*,*,#15455,.T.);
#20652=ORIENTED_EDGE('',*,*,#15456,.F.);
#20653=ORIENTED_EDGE('',*,*,#15457,.F.);
#20654=ORIENTED_EDGE('',*,*,#15458,.F.);
#20655=ORIENTED_EDGE('',*,*,#15459,.T.);
#20656=ORIENTED_EDGE('',*,*,#15460,.T.);
#20657=ORIENTED_EDGE('',*,*,#15461,.T.);
#20658=ORIENTED_EDGE('',*,*,#15462,.F.);
#20659=ORIENTED_EDGE('',*,*,#15463,.F.);
#20660=ORIENTED_EDGE('',*,*,#15464,.F.);
#20661=ORIENTED_EDGE('',*,*,#15465,.T.);
#20662=ORIENTED_EDGE('',*,*,#15466,.T.);
#20663=ORIENTED_EDGE('',*,*,#15467,.T.);
#20664=ORIENTED_EDGE('',*,*,#15468,.F.);
#20665=ORIENTED_EDGE('',*,*,#15469,.F.);
#20666=ORIENTED_EDGE('',*,*,#15470,.F.);
#20667=ORIENTED_EDGE('',*,*,#15471,.T.);
#20668=ORIENTED_EDGE('',*,*,#15472,.T.);
#20669=ORIENTED_EDGE('',*,*,#15473,.T.);
#20670=ORIENTED_EDGE('',*,*,#15474,.F.);
#20671=ORIENTED_EDGE('',*,*,#15475,.F.);
#20672=ORIENTED_EDGE('',*,*,#15476,.F.);
#20673=ORIENTED_EDGE('',*,*,#15477,.T.);
#20674=ORIENTED_EDGE('',*,*,#15478,.T.);
#20675=ORIENTED_EDGE('',*,*,#15479,.T.);
#20676=ORIENTED_EDGE('',*,*,#15480,.F.);
#20677=ORIENTED_EDGE('',*,*,#15481,.F.);
#20678=ORIENTED_EDGE('',*,*,#15482,.F.);
#20679=ORIENTED_EDGE('',*,*,#15483,.T.);
#20680=ORIENTED_EDGE('',*,*,#15484,.T.);
#20681=ORIENTED_EDGE('',*,*,#15485,.T.);
#20682=ORIENTED_EDGE('',*,*,#15486,.F.);
#20683=ORIENTED_EDGE('',*,*,#15487,.F.);
#20684=ORIENTED_EDGE('',*,*,#15488,.F.);
#20685=ORIENTED_EDGE('',*,*,#15489,.T.);
#20686=ORIENTED_EDGE('',*,*,#15490,.T.);
#20687=ORIENTED_EDGE('',*,*,#15491,.T.);
#20688=ORIENTED_EDGE('',*,*,#15492,.F.);
#20689=ORIENTED_EDGE('',*,*,#15493,.F.);
#20690=ORIENTED_EDGE('',*,*,#15494,.F.);
#20691=ORIENTED_EDGE('',*,*,#15495,.T.);
#20692=ORIENTED_EDGE('',*,*,#15496,.T.);
#20693=ORIENTED_EDGE('',*,*,#15497,.T.);
#20694=ORIENTED_EDGE('',*,*,#15498,.F.);
#20695=ORIENTED_EDGE('',*,*,#15499,.F.);
#20696=ORIENTED_EDGE('',*,*,#15500,.F.);
#20697=ORIENTED_EDGE('',*,*,#15501,.T.);
#20698=ORIENTED_EDGE('',*,*,#15502,.T.);
#20699=ORIENTED_EDGE('',*,*,#15503,.T.);
#20700=ORIENTED_EDGE('',*,*,#15504,.F.);
#20701=ORIENTED_EDGE('',*,*,#15505,.F.);
#20702=ORIENTED_EDGE('',*,*,#15506,.F.);
#20703=ORIENTED_EDGE('',*,*,#15507,.T.);
#20704=ORIENTED_EDGE('',*,*,#15508,.T.);
#20705=ORIENTED_EDGE('',*,*,#15509,.T.);
#20706=ORIENTED_EDGE('',*,*,#15510,.F.);
#20707=ORIENTED_EDGE('',*,*,#15511,.F.);
#20708=ORIENTED_EDGE('',*,*,#15512,.F.);
#20709=ORIENTED_EDGE('',*,*,#15513,.T.);
#20710=ORIENTED_EDGE('',*,*,#15514,.T.);
#20711=ORIENTED_EDGE('',*,*,#15515,.T.);
#20712=ORIENTED_EDGE('',*,*,#15516,.F.);
#20713=ORIENTED_EDGE('',*,*,#15517,.F.);
#20714=ORIENTED_EDGE('',*,*,#15518,.F.);
#20715=ORIENTED_EDGE('',*,*,#15519,.T.);
#20716=ORIENTED_EDGE('',*,*,#15520,.T.);
#20717=ORIENTED_EDGE('',*,*,#15521,.T.);
#20718=ORIENTED_EDGE('',*,*,#15522,.F.);
#20719=ORIENTED_EDGE('',*,*,#15523,.F.);
#20720=ORIENTED_EDGE('',*,*,#15524,.F.);
#20721=ORIENTED_EDGE('',*,*,#15525,.T.);
#20722=ORIENTED_EDGE('',*,*,#15526,.T.);
#20723=ORIENTED_EDGE('',*,*,#15527,.T.);
#20724=ORIENTED_EDGE('',*,*,#15528,.F.);
#20725=ORIENTED_EDGE('',*,*,#15529,.F.);
#20726=ORIENTED_EDGE('',*,*,#15530,.F.);
#20727=ORIENTED_EDGE('',*,*,#15531,.T.);
#20728=ORIENTED_EDGE('',*,*,#15532,.T.);
#20729=ORIENTED_EDGE('',*,*,#15533,.T.);
#20730=ORIENTED_EDGE('',*,*,#15534,.F.);
#20731=ORIENTED_EDGE('',*,*,#15535,.F.);
#20732=ORIENTED_EDGE('',*,*,#15536,.F.);
#20733=ORIENTED_EDGE('',*,*,#15537,.T.);
#20734=ORIENTED_EDGE('',*,*,#15538,.T.);
#20735=ORIENTED_EDGE('',*,*,#15539,.T.);
#20736=ORIENTED_EDGE('',*,*,#15540,.F.);
#20737=ORIENTED_EDGE('',*,*,#15541,.F.);
#20738=ORIENTED_EDGE('',*,*,#15542,.F.);
#20739=ORIENTED_EDGE('',*,*,#15543,.T.);
#20740=ORIENTED_EDGE('',*,*,#15544,.T.);
#20741=ORIENTED_EDGE('',*,*,#15545,.T.);
#20742=ORIENTED_EDGE('',*,*,#15546,.F.);
#20743=ORIENTED_EDGE('',*,*,#15547,.F.);
#20744=ORIENTED_EDGE('',*,*,#15548,.F.);
#20745=ORIENTED_EDGE('',*,*,#15549,.T.);
#20746=ORIENTED_EDGE('',*,*,#15550,.T.);
#20747=ORIENTED_EDGE('',*,*,#15551,.T.);
#20748=ORIENTED_EDGE('',*,*,#15552,.F.);
#20749=ORIENTED_EDGE('',*,*,#15553,.F.);
#20750=ORIENTED_EDGE('',*,*,#15554,.F.);
#20751=ORIENTED_EDGE('',*,*,#15555,.T.);
#20752=ORIENTED_EDGE('',*,*,#15556,.T.);
#20753=ORIENTED_EDGE('',*,*,#15557,.T.);
#20754=ORIENTED_EDGE('',*,*,#15558,.F.);
#20755=ORIENTED_EDGE('',*,*,#15559,.F.);
#20756=ORIENTED_EDGE('',*,*,#15560,.F.);
#20757=ORIENTED_EDGE('',*,*,#15561,.T.);
#20758=ORIENTED_EDGE('',*,*,#15562,.T.);
#20759=ORIENTED_EDGE('',*,*,#15563,.T.);
#20760=ORIENTED_EDGE('',*,*,#15564,.F.);
#20761=ORIENTED_EDGE('',*,*,#15565,.F.);
#20762=ORIENTED_EDGE('',*,*,#15566,.F.);
#20763=ORIENTED_EDGE('',*,*,#15567,.T.);
#20764=ORIENTED_EDGE('',*,*,#15568,.T.);
#20765=ORIENTED_EDGE('',*,*,#15205,.T.);
#20766=ORIENTED_EDGE('',*,*,#15569,.T.);
#20767=ORIENTED_EDGE('',*,*,#15209,.T.);
#20768=ORIENTED_EDGE('',*,*,#15570,.T.);
#20769=ORIENTED_EDGE('',*,*,#15571,.T.);
#20770=ORIENTED_EDGE('',*,*,#15572,.T.);
#20771=ORIENTED_EDGE('',*,*,#15573,.T.);
#20772=ORIENTED_EDGE('',*,*,#15574,.T.);
#20773=ORIENTED_EDGE('',*,*,#15571,.F.);
#20774=ORIENTED_EDGE('',*,*,#15575,.T.);
#20775=ORIENTED_EDGE('',*,*,#15213,.T.);
#20776=ORIENTED_EDGE('',*,*,#15576,.T.);
#20777=ORIENTED_EDGE('',*,*,#15573,.F.);
#20778=ORIENTED_EDGE('',*,*,#15569,.F.);
#20779=ORIENTED_EDGE('',*,*,#15577,.T.);
#20780=ORIENTED_EDGE('',*,*,#15578,.T.);
#20781=ORIENTED_EDGE('',*,*,#15210,.F.);
#20782=ORIENTED_EDGE('',*,*,#15574,.F.);
#20783=ORIENTED_EDGE('',*,*,#15579,.T.);
#20784=ORIENTED_EDGE('',*,*,#15580,.T.);
#20785=ORIENTED_EDGE('',*,*,#15577,.F.);
#20786=ORIENTED_EDGE('',*,*,#15576,.F.);
#20787=ORIENTED_EDGE('',*,*,#15212,.F.);
#20788=ORIENTED_EDGE('',*,*,#15581,.T.);
#20789=ORIENTED_EDGE('',*,*,#15579,.F.);
#20790=ORIENTED_EDGE('',*,*,#15582,.T.);
#20791=ORIENTED_EDGE('',*,*,#15215,.T.);
#20792=ORIENTED_EDGE('',*,*,#15583,.T.);
#20793=ORIENTED_EDGE('',*,*,#15584,.T.);
#20794=ORIENTED_EDGE('',*,*,#15585,.T.);
#20795=ORIENTED_EDGE('',*,*,#15586,.T.);
#20796=ORIENTED_EDGE('',*,*,#15587,.T.);
#20797=ORIENTED_EDGE('',*,*,#15584,.F.);
#20798=ORIENTED_EDGE('',*,*,#15588,.T.);
#20799=ORIENTED_EDGE('',*,*,#15219,.T.);
#20800=ORIENTED_EDGE('',*,*,#15589,.T.);
#20801=ORIENTED_EDGE('',*,*,#15586,.F.);
#20802=ORIENTED_EDGE('',*,*,#15582,.F.);
#20803=ORIENTED_EDGE('',*,*,#15590,.T.);
#20804=ORIENTED_EDGE('',*,*,#15591,.T.);
#20805=ORIENTED_EDGE('',*,*,#15216,.F.);
#20806=ORIENTED_EDGE('',*,*,#15587,.F.);
#20807=ORIENTED_EDGE('',*,*,#15592,.T.);
#20808=ORIENTED_EDGE('',*,*,#15593,.T.);
#20809=ORIENTED_EDGE('',*,*,#15590,.F.);
#20810=ORIENTED_EDGE('',*,*,#15589,.F.);
#20811=ORIENTED_EDGE('',*,*,#15218,.F.);
#20812=ORIENTED_EDGE('',*,*,#15594,.T.);
#20813=ORIENTED_EDGE('',*,*,#15592,.F.);
#20814=ORIENTED_EDGE('',*,*,#15595,.T.);
#20815=ORIENTED_EDGE('',*,*,#15404,.T.);
#20816=ORIENTED_EDGE('',*,*,#15596,.T.);
#20817=ORIENTED_EDGE('',*,*,#15597,.T.);
#20818=ORIENTED_EDGE('',*,*,#15598,.T.);
#20819=ORIENTED_EDGE('',*,*,#15599,.T.);
#20820=ORIENTED_EDGE('',*,*,#15600,.T.);
#20821=ORIENTED_EDGE('',*,*,#15597,.F.);
#20822=ORIENTED_EDGE('',*,*,#15601,.T.);
#20823=ORIENTED_EDGE('',*,*,#15408,.T.);
#20824=ORIENTED_EDGE('',*,*,#15602,.T.);
#20825=ORIENTED_EDGE('',*,*,#15599,.F.);
#20826=ORIENTED_EDGE('',*,*,#15595,.F.);
#20827=ORIENTED_EDGE('',*,*,#15603,.T.);
#20828=ORIENTED_EDGE('',*,*,#15604,.T.);
#20829=ORIENTED_EDGE('',*,*,#15405,.F.);
#20830=ORIENTED_EDGE('',*,*,#15600,.F.);
#20831=ORIENTED_EDGE('',*,*,#15605,.T.);
#20832=ORIENTED_EDGE('',*,*,#15606,.T.);
#20833=ORIENTED_EDGE('',*,*,#15603,.F.);
#20834=ORIENTED_EDGE('',*,*,#15602,.F.);
#20835=ORIENTED_EDGE('',*,*,#15407,.F.);
#20836=ORIENTED_EDGE('',*,*,#15607,.T.);
#20837=ORIENTED_EDGE('',*,*,#15605,.F.);
#20838=ORIENTED_EDGE('',*,*,#15608,.T.);
#20839=ORIENTED_EDGE('',*,*,#15410,.T.);
#20840=ORIENTED_EDGE('',*,*,#15609,.T.);
#20841=ORIENTED_EDGE('',*,*,#15610,.T.);
#20842=ORIENTED_EDGE('',*,*,#15611,.T.);
#20843=ORIENTED_EDGE('',*,*,#15612,.T.);
#20844=ORIENTED_EDGE('',*,*,#15613,.T.);
#20845=ORIENTED_EDGE('',*,*,#15610,.F.);
#20846=ORIENTED_EDGE('',*,*,#15608,.F.);
#20847=ORIENTED_EDGE('',*,*,#15614,.T.);
#20848=ORIENTED_EDGE('',*,*,#15615,.T.);
#20849=ORIENTED_EDGE('',*,*,#15411,.F.);
#20850=ORIENTED_EDGE('',*,*,#15613,.F.);
#20851=ORIENTED_EDGE('',*,*,#15616,.T.);
#20852=ORIENTED_EDGE('',*,*,#15617,.T.);
#20853=ORIENTED_EDGE('',*,*,#15614,.F.);
#20854=ORIENTED_EDGE('',*,*,#15414,.T.);
#20855=ORIENTED_EDGE('',*,*,#15618,.T.);
#20856=ORIENTED_EDGE('',*,*,#15612,.F.);
#20857=ORIENTED_EDGE('',*,*,#15619,.T.);
#20858=ORIENTED_EDGE('',*,*,#15620,.F.);
#20859=ORIENTED_EDGE('',*,*,#15621,.F.);
#20860=ORIENTED_EDGE('',*,*,#15565,.T.);
#20861=ORIENTED_EDGE('',*,*,#15622,.F.);
#20862=ORIENTED_EDGE('',*,*,#15623,.F.);
#20863=ORIENTED_EDGE('',*,*,#15624,.F.);
#20864=ORIENTED_EDGE('',*,*,#15559,.T.);
#20865=ORIENTED_EDGE('',*,*,#15625,.F.);
#20866=ORIENTED_EDGE('',*,*,#15626,.F.);
#20867=ORIENTED_EDGE('',*,*,#15627,.F.);
#20868=ORIENTED_EDGE('',*,*,#15553,.T.);
#20869=ORIENTED_EDGE('',*,*,#15628,.F.);
#20870=ORIENTED_EDGE('',*,*,#15629,.F.);
#20871=ORIENTED_EDGE('',*,*,#15630,.F.);
#20872=ORIENTED_EDGE('',*,*,#15547,.T.);
#20873=ORIENTED_EDGE('',*,*,#15631,.F.);
#20874=ORIENTED_EDGE('',*,*,#15632,.F.);
#20875=ORIENTED_EDGE('',*,*,#15633,.F.);
#20876=ORIENTED_EDGE('',*,*,#15541,.T.);
#20877=ORIENTED_EDGE('',*,*,#15634,.F.);
#20878=ORIENTED_EDGE('',*,*,#15635,.F.);
#20879=ORIENTED_EDGE('',*,*,#15636,.F.);
#20880=ORIENTED_EDGE('',*,*,#15535,.T.);
#20881=ORIENTED_EDGE('',*,*,#15637,.F.);
#20882=ORIENTED_EDGE('',*,*,#15638,.F.);
#20883=ORIENTED_EDGE('',*,*,#15639,.F.);
#20884=ORIENTED_EDGE('',*,*,#15529,.T.);
#20885=ORIENTED_EDGE('',*,*,#15640,.F.);
#20886=ORIENTED_EDGE('',*,*,#15641,.F.);
#20887=ORIENTED_EDGE('',*,*,#15642,.F.);
#20888=ORIENTED_EDGE('',*,*,#15523,.T.);
#20889=ORIENTED_EDGE('',*,*,#15643,.F.);
#20890=ORIENTED_EDGE('',*,*,#15644,.F.);
#20891=ORIENTED_EDGE('',*,*,#15645,.F.);
#20892=ORIENTED_EDGE('',*,*,#15517,.T.);
#20893=ORIENTED_EDGE('',*,*,#15646,.F.);
#20894=ORIENTED_EDGE('',*,*,#15647,.F.);
#20895=ORIENTED_EDGE('',*,*,#15648,.F.);
#20896=ORIENTED_EDGE('',*,*,#15511,.T.);
#20897=ORIENTED_EDGE('',*,*,#15649,.F.);
#20898=ORIENTED_EDGE('',*,*,#15650,.F.);
#20899=ORIENTED_EDGE('',*,*,#15651,.F.);
#20900=ORIENTED_EDGE('',*,*,#15505,.T.);
#20901=ORIENTED_EDGE('',*,*,#15652,.F.);
#20902=ORIENTED_EDGE('',*,*,#15653,.F.);
#20903=ORIENTED_EDGE('',*,*,#15654,.F.);
#20904=ORIENTED_EDGE('',*,*,#15499,.T.);
#20905=ORIENTED_EDGE('',*,*,#15655,.F.);
#20906=ORIENTED_EDGE('',*,*,#15656,.F.);
#20907=ORIENTED_EDGE('',*,*,#15657,.F.);
#20908=ORIENTED_EDGE('',*,*,#15493,.T.);
#20909=ORIENTED_EDGE('',*,*,#15658,.F.);
#20910=ORIENTED_EDGE('',*,*,#15659,.F.);
#20911=ORIENTED_EDGE('',*,*,#15660,.F.);
#20912=ORIENTED_EDGE('',*,*,#15487,.T.);
#20913=ORIENTED_EDGE('',*,*,#15661,.F.);
#20914=ORIENTED_EDGE('',*,*,#15662,.F.);
#20915=ORIENTED_EDGE('',*,*,#15663,.F.);
#20916=ORIENTED_EDGE('',*,*,#15481,.T.);
#20917=ORIENTED_EDGE('',*,*,#15664,.F.);
#20918=ORIENTED_EDGE('',*,*,#15665,.F.);
#20919=ORIENTED_EDGE('',*,*,#15666,.F.);
#20920=ORIENTED_EDGE('',*,*,#15475,.T.);
#20921=ORIENTED_EDGE('',*,*,#15667,.F.);
#20922=ORIENTED_EDGE('',*,*,#15668,.F.);
#20923=ORIENTED_EDGE('',*,*,#15669,.F.);
#20924=ORIENTED_EDGE('',*,*,#15469,.T.);
#20925=ORIENTED_EDGE('',*,*,#15670,.F.);
#20926=ORIENTED_EDGE('',*,*,#15671,.F.);
#20927=ORIENTED_EDGE('',*,*,#15672,.F.);
#20928=ORIENTED_EDGE('',*,*,#15463,.T.);
#20929=ORIENTED_EDGE('',*,*,#15673,.F.);
#20930=ORIENTED_EDGE('',*,*,#15674,.F.);
#20931=ORIENTED_EDGE('',*,*,#15675,.F.);
#20932=ORIENTED_EDGE('',*,*,#15457,.T.);
#20933=ORIENTED_EDGE('',*,*,#15676,.F.);
#20934=ORIENTED_EDGE('',*,*,#15677,.F.);
#20935=ORIENTED_EDGE('',*,*,#15678,.F.);
#20936=ORIENTED_EDGE('',*,*,#15451,.T.);
#20937=ORIENTED_EDGE('',*,*,#15679,.F.);
#20938=ORIENTED_EDGE('',*,*,#15680,.F.);
#20939=ORIENTED_EDGE('',*,*,#15681,.F.);
#20940=ORIENTED_EDGE('',*,*,#15445,.T.);
#20941=ORIENTED_EDGE('',*,*,#15682,.F.);
#20942=ORIENTED_EDGE('',*,*,#15683,.F.);
#20943=ORIENTED_EDGE('',*,*,#15684,.F.);
#20944=ORIENTED_EDGE('',*,*,#15439,.T.);
#20945=ORIENTED_EDGE('',*,*,#15685,.F.);
#20946=ORIENTED_EDGE('',*,*,#15686,.F.);
#20947=ORIENTED_EDGE('',*,*,#15687,.F.);
#20948=ORIENTED_EDGE('',*,*,#15433,.T.);
#20949=ORIENTED_EDGE('',*,*,#15688,.F.);
#20950=ORIENTED_EDGE('',*,*,#15689,.F.);
#20951=ORIENTED_EDGE('',*,*,#15690,.F.);
#20952=ORIENTED_EDGE('',*,*,#15427,.T.);
#20953=ORIENTED_EDGE('',*,*,#15691,.F.);
#20954=ORIENTED_EDGE('',*,*,#15692,.F.);
#20955=ORIENTED_EDGE('',*,*,#15693,.F.);
#20956=ORIENTED_EDGE('',*,*,#15421,.T.);
#20957=ORIENTED_EDGE('',*,*,#15694,.F.);
#20958=ORIENTED_EDGE('',*,*,#15695,.F.);
#20959=ORIENTED_EDGE('',*,*,#15696,.F.);
#20960=ORIENTED_EDGE('',*,*,#15415,.T.);
#20961=ORIENTED_EDGE('',*,*,#15619,.F.);
#20962=ORIENTED_EDGE('',*,*,#15611,.F.);
#20963=ORIENTED_EDGE('',*,*,#15609,.F.);
#20964=ORIENTED_EDGE('',*,*,#15409,.T.);
#20965=ORIENTED_EDGE('',*,*,#15601,.F.);
#20966=ORIENTED_EDGE('',*,*,#15598,.F.);
#20967=ORIENTED_EDGE('',*,*,#15596,.F.);
#20968=ORIENTED_EDGE('',*,*,#15403,.T.);
#20969=ORIENTED_EDGE('',*,*,#15220,.T.);
#20970=ORIENTED_EDGE('',*,*,#15588,.F.);
#20971=ORIENTED_EDGE('',*,*,#15585,.F.);
#20972=ORIENTED_EDGE('',*,*,#15583,.F.);
#20973=ORIENTED_EDGE('',*,*,#15214,.T.);
#20974=ORIENTED_EDGE('',*,*,#15575,.F.);
#20975=ORIENTED_EDGE('',*,*,#15572,.F.);
#20976=ORIENTED_EDGE('',*,*,#15570,.F.);
#20977=ORIENTED_EDGE('',*,*,#15208,.T.);
#20978=ORIENTED_EDGE('',*,*,#15204,.F.);
#20979=ORIENTED_EDGE('',*,*,#15697,.F.);
#20980=ORIENTED_EDGE('',*,*,#15698,.F.);
#20981=ORIENTED_EDGE('',*,*,#15699,.F.);
#20982=ORIENTED_EDGE('',*,*,#15700,.F.);
#20983=ORIENTED_EDGE('',*,*,#15701,.F.);
#20984=ORIENTED_EDGE('',*,*,#15702,.F.);
#20985=ORIENTED_EDGE('',*,*,#15703,.F.);
#20986=ORIENTED_EDGE('',*,*,#15704,.F.);
#20987=ORIENTED_EDGE('',*,*,#15705,.T.);
#20988=ORIENTED_EDGE('',*,*,#15416,.T.);
#20989=ORIENTED_EDGE('',*,*,#15696,.T.);
#20990=ORIENTED_EDGE('',*,*,#15706,.T.);
#20991=ORIENTED_EDGE('',*,*,#15695,.T.);
#20992=ORIENTED_EDGE('',*,*,#15707,.T.);
#20993=ORIENTED_EDGE('',*,*,#15708,.T.);
#20994=ORIENTED_EDGE('',*,*,#15706,.F.);
#20995=ORIENTED_EDGE('',*,*,#15694,.T.);
#20996=ORIENTED_EDGE('',*,*,#15420,.T.);
#20997=ORIENTED_EDGE('',*,*,#15709,.T.);
#20998=ORIENTED_EDGE('',*,*,#15707,.F.);
#20999=ORIENTED_EDGE('',*,*,#15710,.T.);
#21000=ORIENTED_EDGE('',*,*,#15422,.T.);
#21001=ORIENTED_EDGE('',*,*,#15693,.T.);
#21002=ORIENTED_EDGE('',*,*,#15711,.T.);
#21003=ORIENTED_EDGE('',*,*,#15692,.T.);
#21004=ORIENTED_EDGE('',*,*,#15712,.T.);
#21005=ORIENTED_EDGE('',*,*,#15713,.T.);
#21006=ORIENTED_EDGE('',*,*,#15711,.F.);
#21007=ORIENTED_EDGE('',*,*,#15691,.T.);
#21008=ORIENTED_EDGE('',*,*,#15426,.T.);
#21009=ORIENTED_EDGE('',*,*,#15714,.T.);
#21010=ORIENTED_EDGE('',*,*,#15712,.F.);
#21011=ORIENTED_EDGE('',*,*,#15715,.T.);
#21012=ORIENTED_EDGE('',*,*,#15428,.T.);
#21013=ORIENTED_EDGE('',*,*,#15690,.T.);
#21014=ORIENTED_EDGE('',*,*,#15716,.T.);
#21015=ORIENTED_EDGE('',*,*,#15689,.T.);
#21016=ORIENTED_EDGE('',*,*,#15717,.T.);
#21017=ORIENTED_EDGE('',*,*,#15718,.T.);
#21018=ORIENTED_EDGE('',*,*,#15716,.F.);
#21019=ORIENTED_EDGE('',*,*,#15688,.T.);
#21020=ORIENTED_EDGE('',*,*,#15432,.T.);
#21021=ORIENTED_EDGE('',*,*,#15719,.T.);
#21022=ORIENTED_EDGE('',*,*,#15717,.F.);
#21023=ORIENTED_EDGE('',*,*,#15720,.T.);
#21024=ORIENTED_EDGE('',*,*,#15434,.T.);
#21025=ORIENTED_EDGE('',*,*,#15687,.T.);
#21026=ORIENTED_EDGE('',*,*,#15721,.T.);
#21027=ORIENTED_EDGE('',*,*,#15686,.T.);
#21028=ORIENTED_EDGE('',*,*,#15722,.T.);
#21029=ORIENTED_EDGE('',*,*,#15723,.T.);
#21030=ORIENTED_EDGE('',*,*,#15721,.F.);
#21031=ORIENTED_EDGE('',*,*,#15685,.T.);
#21032=ORIENTED_EDGE('',*,*,#15438,.T.);
#21033=ORIENTED_EDGE('',*,*,#15724,.T.);
#21034=ORIENTED_EDGE('',*,*,#15722,.F.);
#21035=ORIENTED_EDGE('',*,*,#15725,.T.);
#21036=ORIENTED_EDGE('',*,*,#15440,.T.);
#21037=ORIENTED_EDGE('',*,*,#15684,.T.);
#21038=ORIENTED_EDGE('',*,*,#15726,.T.);
#21039=ORIENTED_EDGE('',*,*,#15683,.T.);
#21040=ORIENTED_EDGE('',*,*,#15727,.T.);
#21041=ORIENTED_EDGE('',*,*,#15728,.T.);
#21042=ORIENTED_EDGE('',*,*,#15726,.F.);
#21043=ORIENTED_EDGE('',*,*,#15682,.T.);
#21044=ORIENTED_EDGE('',*,*,#15444,.T.);
#21045=ORIENTED_EDGE('',*,*,#15729,.T.);
#21046=ORIENTED_EDGE('',*,*,#15727,.F.);
#21047=ORIENTED_EDGE('',*,*,#15730,.T.);
#21048=ORIENTED_EDGE('',*,*,#15446,.T.);
#21049=ORIENTED_EDGE('',*,*,#15681,.T.);
#21050=ORIENTED_EDGE('',*,*,#15731,.T.);
#21051=ORIENTED_EDGE('',*,*,#15680,.T.);
#21052=ORIENTED_EDGE('',*,*,#15732,.T.);
#21053=ORIENTED_EDGE('',*,*,#15733,.T.);
#21054=ORIENTED_EDGE('',*,*,#15731,.F.);
#21055=ORIENTED_EDGE('',*,*,#15679,.T.);
#21056=ORIENTED_EDGE('',*,*,#15450,.T.);
#21057=ORIENTED_EDGE('',*,*,#15734,.T.);
#21058=ORIENTED_EDGE('',*,*,#15732,.F.);
#21059=ORIENTED_EDGE('',*,*,#15735,.T.);
#21060=ORIENTED_EDGE('',*,*,#15736,.T.);
#21061=ORIENTED_EDGE('',*,*,#15620,.T.);
#21062=ORIENTED_EDGE('',*,*,#15203,.F.);
#21063=ORIENTED_EDGE('',*,*,#15735,.F.);
#21064=ORIENTED_EDGE('',*,*,#15207,.T.);
#21065=ORIENTED_EDGE('',*,*,#15737,.T.);
#21066=ORIENTED_EDGE('',*,*,#15738,.F.);
#21067=ORIENTED_EDGE('',*,*,#15566,.T.);
#21068=ORIENTED_EDGE('',*,*,#15621,.T.);
#21069=ORIENTED_EDGE('',*,*,#15736,.F.);
#21070=ORIENTED_EDGE('',*,*,#15739,.T.);
#21071=ORIENTED_EDGE('',*,*,#15740,.T.);
#21072=ORIENTED_EDGE('',*,*,#15560,.T.);
#21073=ORIENTED_EDGE('',*,*,#15624,.T.);
#21074=ORIENTED_EDGE('',*,*,#15741,.T.);
#21075=ORIENTED_EDGE('',*,*,#15742,.T.);
#21076=ORIENTED_EDGE('',*,*,#15741,.F.);
#21077=ORIENTED_EDGE('',*,*,#15623,.T.);
#21078=ORIENTED_EDGE('',*,*,#15743,.T.);
#21079=ORIENTED_EDGE('',*,*,#15622,.T.);
#21080=ORIENTED_EDGE('',*,*,#15564,.T.);
#21081=ORIENTED_EDGE('',*,*,#15744,.T.);
#21082=ORIENTED_EDGE('',*,*,#15743,.F.);
#21083=ORIENTED_EDGE('',*,*,#15740,.F.);
#21084=ORIENTED_EDGE('',*,*,#15745,.T.);
#21085=ORIENTED_EDGE('',*,*,#15746,.T.);
#21086=ORIENTED_EDGE('',*,*,#15561,.F.);
#21087=ORIENTED_EDGE('',*,*,#15742,.F.);
#21088=ORIENTED_EDGE('',*,*,#15747,.T.);
#21089=ORIENTED_EDGE('',*,*,#15748,.T.);
#21090=ORIENTED_EDGE('',*,*,#15745,.F.);
#21091=ORIENTED_EDGE('',*,*,#15744,.F.);
#21092=ORIENTED_EDGE('',*,*,#15563,.F.);
#21093=ORIENTED_EDGE('',*,*,#15749,.T.);
#21094=ORIENTED_EDGE('',*,*,#15747,.F.);
#21095=ORIENTED_EDGE('',*,*,#15750,.T.);
#21096=ORIENTED_EDGE('',*,*,#15554,.T.);
#21097=ORIENTED_EDGE('',*,*,#15627,.T.);
#21098=ORIENTED_EDGE('',*,*,#15751,.T.);
#21099=ORIENTED_EDGE('',*,*,#15752,.T.);
#21100=ORIENTED_EDGE('',*,*,#15751,.F.);
#21101=ORIENTED_EDGE('',*,*,#15626,.T.);
#21102=ORIENTED_EDGE('',*,*,#15753,.T.);
#21103=ORIENTED_EDGE('',*,*,#15625,.T.);
#21104=ORIENTED_EDGE('',*,*,#15558,.T.);
#21105=ORIENTED_EDGE('',*,*,#15754,.T.);
#21106=ORIENTED_EDGE('',*,*,#15753,.F.);
#21107=ORIENTED_EDGE('',*,*,#15750,.F.);
#21108=ORIENTED_EDGE('',*,*,#15755,.T.);
#21109=ORIENTED_EDGE('',*,*,#15756,.T.);
#21110=ORIENTED_EDGE('',*,*,#15555,.F.);
#21111=ORIENTED_EDGE('',*,*,#15752,.F.);
#21112=ORIENTED_EDGE('',*,*,#15757,.T.);
#21113=ORIENTED_EDGE('',*,*,#15758,.T.);
#21114=ORIENTED_EDGE('',*,*,#15755,.F.);
#21115=ORIENTED_EDGE('',*,*,#15754,.F.);
#21116=ORIENTED_EDGE('',*,*,#15557,.F.);
#21117=ORIENTED_EDGE('',*,*,#15759,.T.);
#21118=ORIENTED_EDGE('',*,*,#15757,.F.);
#21119=ORIENTED_EDGE('',*,*,#15760,.T.);
#21120=ORIENTED_EDGE('',*,*,#15548,.T.);
#21121=ORIENTED_EDGE('',*,*,#15630,.T.);
#21122=ORIENTED_EDGE('',*,*,#15761,.T.);
#21123=ORIENTED_EDGE('',*,*,#15762,.T.);
#21124=ORIENTED_EDGE('',*,*,#15761,.F.);
#21125=ORIENTED_EDGE('',*,*,#15629,.T.);
#21126=ORIENTED_EDGE('',*,*,#15763,.T.);
#21127=ORIENTED_EDGE('',*,*,#15628,.T.);
#21128=ORIENTED_EDGE('',*,*,#15552,.T.);
#21129=ORIENTED_EDGE('',*,*,#15764,.T.);
#21130=ORIENTED_EDGE('',*,*,#15763,.F.);
#21131=ORIENTED_EDGE('',*,*,#15760,.F.);
#21132=ORIENTED_EDGE('',*,*,#15765,.T.);
#21133=ORIENTED_EDGE('',*,*,#15766,.T.);
#21134=ORIENTED_EDGE('',*,*,#15549,.F.);
#21135=ORIENTED_EDGE('',*,*,#15762,.F.);
#21136=ORIENTED_EDGE('',*,*,#15767,.T.);
#21137=ORIENTED_EDGE('',*,*,#15768,.T.);
#21138=ORIENTED_EDGE('',*,*,#15765,.F.);
#21139=ORIENTED_EDGE('',*,*,#15764,.F.);
#21140=ORIENTED_EDGE('',*,*,#15551,.F.);
#21141=ORIENTED_EDGE('',*,*,#15769,.T.);
#21142=ORIENTED_EDGE('',*,*,#15767,.F.);
#21143=ORIENTED_EDGE('',*,*,#15770,.T.);
#21144=ORIENTED_EDGE('',*,*,#15542,.T.);
#21145=ORIENTED_EDGE('',*,*,#15633,.T.);
#21146=ORIENTED_EDGE('',*,*,#15771,.T.);
#21147=ORIENTED_EDGE('',*,*,#15772,.T.);
#21148=ORIENTED_EDGE('',*,*,#15771,.F.);
#21149=ORIENTED_EDGE('',*,*,#15632,.T.);
#21150=ORIENTED_EDGE('',*,*,#15773,.T.);
#21151=ORIENTED_EDGE('',*,*,#15631,.T.);
#21152=ORIENTED_EDGE('',*,*,#15546,.T.);
#21153=ORIENTED_EDGE('',*,*,#15774,.T.);
#21154=ORIENTED_EDGE('',*,*,#15773,.F.);
#21155=ORIENTED_EDGE('',*,*,#15770,.F.);
#21156=ORIENTED_EDGE('',*,*,#15775,.T.);
#21157=ORIENTED_EDGE('',*,*,#15776,.T.);
#21158=ORIENTED_EDGE('',*,*,#15543,.F.);
#21159=ORIENTED_EDGE('',*,*,#15772,.F.);
#21160=ORIENTED_EDGE('',*,*,#15777,.T.);
#21161=ORIENTED_EDGE('',*,*,#15778,.T.);
#21162=ORIENTED_EDGE('',*,*,#15775,.F.);
#21163=ORIENTED_EDGE('',*,*,#15774,.F.);
#21164=ORIENTED_EDGE('',*,*,#15545,.F.);
#21165=ORIENTED_EDGE('',*,*,#15779,.T.);
#21166=ORIENTED_EDGE('',*,*,#15777,.F.);
#21167=ORIENTED_EDGE('',*,*,#15780,.T.);
#21168=ORIENTED_EDGE('',*,*,#15536,.T.);
#21169=ORIENTED_EDGE('',*,*,#15636,.T.);
#21170=ORIENTED_EDGE('',*,*,#15781,.T.);
#21171=ORIENTED_EDGE('',*,*,#15782,.T.);
#21172=ORIENTED_EDGE('',*,*,#15781,.F.);
#21173=ORIENTED_EDGE('',*,*,#15635,.T.);
#21174=ORIENTED_EDGE('',*,*,#15783,.T.);
#21175=ORIENTED_EDGE('',*,*,#15634,.T.);
#21176=ORIENTED_EDGE('',*,*,#15540,.T.);
#21177=ORIENTED_EDGE('',*,*,#15784,.T.);
#21178=ORIENTED_EDGE('',*,*,#15783,.F.);
#21179=ORIENTED_EDGE('',*,*,#15780,.F.);
#21180=ORIENTED_EDGE('',*,*,#15785,.T.);
#21181=ORIENTED_EDGE('',*,*,#15786,.T.);
#21182=ORIENTED_EDGE('',*,*,#15537,.F.);
#21183=ORIENTED_EDGE('',*,*,#15782,.F.);
#21184=ORIENTED_EDGE('',*,*,#15787,.T.);
#21185=ORIENTED_EDGE('',*,*,#15788,.T.);
#21186=ORIENTED_EDGE('',*,*,#15785,.F.);
#21187=ORIENTED_EDGE('',*,*,#15784,.F.);
#21188=ORIENTED_EDGE('',*,*,#15539,.F.);
#21189=ORIENTED_EDGE('',*,*,#15789,.T.);
#21190=ORIENTED_EDGE('',*,*,#15787,.F.);
#21191=ORIENTED_EDGE('',*,*,#15790,.T.);
#21192=ORIENTED_EDGE('',*,*,#15530,.T.);
#21193=ORIENTED_EDGE('',*,*,#15639,.T.);
#21194=ORIENTED_EDGE('',*,*,#15791,.T.);
#21195=ORIENTED_EDGE('',*,*,#15792,.T.);
#21196=ORIENTED_EDGE('',*,*,#15791,.F.);
#21197=ORIENTED_EDGE('',*,*,#15638,.T.);
#21198=ORIENTED_EDGE('',*,*,#15793,.T.);
#21199=ORIENTED_EDGE('',*,*,#15637,.T.);
#21200=ORIENTED_EDGE('',*,*,#15534,.T.);
#21201=ORIENTED_EDGE('',*,*,#15794,.T.);
#21202=ORIENTED_EDGE('',*,*,#15793,.F.);
#21203=ORIENTED_EDGE('',*,*,#15790,.F.);
#21204=ORIENTED_EDGE('',*,*,#15795,.T.);
#21205=ORIENTED_EDGE('',*,*,#15796,.T.);
#21206=ORIENTED_EDGE('',*,*,#15531,.F.);
#21207=ORIENTED_EDGE('',*,*,#15792,.F.);
#21208=ORIENTED_EDGE('',*,*,#15797,.T.);
#21209=ORIENTED_EDGE('',*,*,#15798,.T.);
#21210=ORIENTED_EDGE('',*,*,#15795,.F.);
#21211=ORIENTED_EDGE('',*,*,#15794,.F.);
#21212=ORIENTED_EDGE('',*,*,#15533,.F.);
#21213=ORIENTED_EDGE('',*,*,#15799,.T.);
#21214=ORIENTED_EDGE('',*,*,#15797,.F.);
#21215=ORIENTED_EDGE('',*,*,#15528,.T.);
#21216=ORIENTED_EDGE('',*,*,#15800,.T.);
#21217=ORIENTED_EDGE('',*,*,#15801,.T.);
#21218=ORIENTED_EDGE('',*,*,#15640,.T.);
#21219=ORIENTED_EDGE('',*,*,#15800,.F.);
#21220=ORIENTED_EDGE('',*,*,#15527,.F.);
#21221=ORIENTED_EDGE('',*,*,#15802,.T.);
#21222=ORIENTED_EDGE('',*,*,#15803,.F.);
#21223=ORIENTED_EDGE('',*,*,#15804,.T.);
#21224=ORIENTED_EDGE('',*,*,#15524,.T.);
#21225=ORIENTED_EDGE('',*,*,#15642,.T.);
#21226=ORIENTED_EDGE('',*,*,#15805,.T.);
#21227=ORIENTED_EDGE('',*,*,#15641,.T.);
#21228=ORIENTED_EDGE('',*,*,#15801,.F.);
#21229=ORIENTED_EDGE('',*,*,#15806,.T.);
#21230=ORIENTED_EDGE('',*,*,#15805,.F.);
#21231=ORIENTED_EDGE('',*,*,#15804,.F.);
#21232=ORIENTED_EDGE('',*,*,#15807,.T.);
#21233=ORIENTED_EDGE('',*,*,#15808,.T.);
#21234=ORIENTED_EDGE('',*,*,#15525,.F.);
#21235=ORIENTED_EDGE('',*,*,#15806,.F.);
#21236=ORIENTED_EDGE('',*,*,#15803,.T.);
#21237=ORIENTED_EDGE('',*,*,#15809,.T.);
#21238=ORIENTED_EDGE('',*,*,#15807,.F.);
#21239=ORIENTED_EDGE('',*,*,#15810,.T.);
#21240=ORIENTED_EDGE('',*,*,#15518,.T.);
#21241=ORIENTED_EDGE('',*,*,#15645,.T.);
#21242=ORIENTED_EDGE('',*,*,#15811,.T.);
#21243=ORIENTED_EDGE('',*,*,#15812,.T.);
#21244=ORIENTED_EDGE('',*,*,#15811,.F.);
#21245=ORIENTED_EDGE('',*,*,#15644,.T.);
#21246=ORIENTED_EDGE('',*,*,#15813,.T.);
#21247=ORIENTED_EDGE('',*,*,#15643,.T.);
#21248=ORIENTED_EDGE('',*,*,#15522,.T.);
#21249=ORIENTED_EDGE('',*,*,#15814,.T.);
#21250=ORIENTED_EDGE('',*,*,#15813,.F.);
#21251=ORIENTED_EDGE('',*,*,#15810,.F.);
#21252=ORIENTED_EDGE('',*,*,#15815,.T.);
#21253=ORIENTED_EDGE('',*,*,#15816,.T.);
#21254=ORIENTED_EDGE('',*,*,#15519,.F.);
#21255=ORIENTED_EDGE('',*,*,#15812,.F.);
#21256=ORIENTED_EDGE('',*,*,#15817,.T.);
#21257=ORIENTED_EDGE('',*,*,#15818,.T.);
#21258=ORIENTED_EDGE('',*,*,#15815,.F.);
#21259=ORIENTED_EDGE('',*,*,#15814,.F.);
#21260=ORIENTED_EDGE('',*,*,#15521,.F.);
#21261=ORIENTED_EDGE('',*,*,#15819,.T.);
#21262=ORIENTED_EDGE('',*,*,#15817,.F.);
#21263=ORIENTED_EDGE('',*,*,#15820,.T.);
#21264=ORIENTED_EDGE('',*,*,#15512,.T.);
#21265=ORIENTED_EDGE('',*,*,#15648,.T.);
#21266=ORIENTED_EDGE('',*,*,#15821,.T.);
#21267=ORIENTED_EDGE('',*,*,#15822,.T.);
#21268=ORIENTED_EDGE('',*,*,#15821,.F.);
#21269=ORIENTED_EDGE('',*,*,#15647,.T.);
#21270=ORIENTED_EDGE('',*,*,#15823,.T.);
#21271=ORIENTED_EDGE('',*,*,#15646,.T.);
#21272=ORIENTED_EDGE('',*,*,#15516,.T.);
#21273=ORIENTED_EDGE('',*,*,#15824,.T.);
#21274=ORIENTED_EDGE('',*,*,#15823,.F.);
#21275=ORIENTED_EDGE('',*,*,#15820,.F.);
#21276=ORIENTED_EDGE('',*,*,#15825,.T.);
#21277=ORIENTED_EDGE('',*,*,#15826,.T.);
#21278=ORIENTED_EDGE('',*,*,#15513,.F.);
#21279=ORIENTED_EDGE('',*,*,#15822,.F.);
#21280=ORIENTED_EDGE('',*,*,#15827,.T.);
#21281=ORIENTED_EDGE('',*,*,#15828,.T.);
#21282=ORIENTED_EDGE('',*,*,#15825,.F.);
#21283=ORIENTED_EDGE('',*,*,#15824,.F.);
#21284=ORIENTED_EDGE('',*,*,#15515,.F.);
#21285=ORIENTED_EDGE('',*,*,#15829,.T.);
#21286=ORIENTED_EDGE('',*,*,#15827,.F.);
#21287=ORIENTED_EDGE('',*,*,#15830,.T.);
#21288=ORIENTED_EDGE('',*,*,#15506,.T.);
#21289=ORIENTED_EDGE('',*,*,#15651,.T.);
#21290=ORIENTED_EDGE('',*,*,#15831,.T.);
#21291=ORIENTED_EDGE('',*,*,#15832,.T.);
#21292=ORIENTED_EDGE('',*,*,#15831,.F.);
#21293=ORIENTED_EDGE('',*,*,#15650,.T.);
#21294=ORIENTED_EDGE('',*,*,#15833,.T.);
#21295=ORIENTED_EDGE('',*,*,#15649,.T.);
#21296=ORIENTED_EDGE('',*,*,#15510,.T.);
#21297=ORIENTED_EDGE('',*,*,#15834,.T.);
#21298=ORIENTED_EDGE('',*,*,#15833,.F.);
#21299=ORIENTED_EDGE('',*,*,#15830,.F.);
#21300=ORIENTED_EDGE('',*,*,#15835,.T.);
#21301=ORIENTED_EDGE('',*,*,#15836,.T.);
#21302=ORIENTED_EDGE('',*,*,#15507,.F.);
#21303=ORIENTED_EDGE('',*,*,#15832,.F.);
#21304=ORIENTED_EDGE('',*,*,#15837,.T.);
#21305=ORIENTED_EDGE('',*,*,#15838,.T.);
#21306=ORIENTED_EDGE('',*,*,#15835,.F.);
#21307=ORIENTED_EDGE('',*,*,#15834,.F.);
#21308=ORIENTED_EDGE('',*,*,#15509,.F.);
#21309=ORIENTED_EDGE('',*,*,#15839,.T.);
#21310=ORIENTED_EDGE('',*,*,#15837,.F.);
#21311=ORIENTED_EDGE('',*,*,#15840,.T.);
#21312=ORIENTED_EDGE('',*,*,#15500,.T.);
#21313=ORIENTED_EDGE('',*,*,#15654,.T.);
#21314=ORIENTED_EDGE('',*,*,#15841,.T.);
#21315=ORIENTED_EDGE('',*,*,#15842,.T.);
#21316=ORIENTED_EDGE('',*,*,#15841,.F.);
#21317=ORIENTED_EDGE('',*,*,#15653,.T.);
#21318=ORIENTED_EDGE('',*,*,#15843,.T.);
#21319=ORIENTED_EDGE('',*,*,#15652,.T.);
#21320=ORIENTED_EDGE('',*,*,#15504,.T.);
#21321=ORIENTED_EDGE('',*,*,#15844,.T.);
#21322=ORIENTED_EDGE('',*,*,#15843,.F.);
#21323=ORIENTED_EDGE('',*,*,#15840,.F.);
#21324=ORIENTED_EDGE('',*,*,#15845,.T.);
#21325=ORIENTED_EDGE('',*,*,#15846,.T.);
#21326=ORIENTED_EDGE('',*,*,#15501,.F.);
#21327=ORIENTED_EDGE('',*,*,#15842,.F.);
#21328=ORIENTED_EDGE('',*,*,#15847,.T.);
#21329=ORIENTED_EDGE('',*,*,#15848,.T.);
#21330=ORIENTED_EDGE('',*,*,#15845,.F.);
#21331=ORIENTED_EDGE('',*,*,#15844,.F.);
#21332=ORIENTED_EDGE('',*,*,#15503,.F.);
#21333=ORIENTED_EDGE('',*,*,#15849,.T.);
#21334=ORIENTED_EDGE('',*,*,#15847,.F.);
#21335=ORIENTED_EDGE('',*,*,#15850,.T.);
#21336=ORIENTED_EDGE('',*,*,#15494,.T.);
#21337=ORIENTED_EDGE('',*,*,#15657,.T.);
#21338=ORIENTED_EDGE('',*,*,#15851,.T.);
#21339=ORIENTED_EDGE('',*,*,#15852,.T.);
#21340=ORIENTED_EDGE('',*,*,#15851,.F.);
#21341=ORIENTED_EDGE('',*,*,#15656,.T.);
#21342=ORIENTED_EDGE('',*,*,#15853,.T.);
#21343=ORIENTED_EDGE('',*,*,#15655,.T.);
#21344=ORIENTED_EDGE('',*,*,#15498,.T.);
#21345=ORIENTED_EDGE('',*,*,#15854,.T.);
#21346=ORIENTED_EDGE('',*,*,#15853,.F.);
#21347=ORIENTED_EDGE('',*,*,#15850,.F.);
#21348=ORIENTED_EDGE('',*,*,#15855,.T.);
#21349=ORIENTED_EDGE('',*,*,#15856,.T.);
#21350=ORIENTED_EDGE('',*,*,#15495,.F.);
#21351=ORIENTED_EDGE('',*,*,#15852,.F.);
#21352=ORIENTED_EDGE('',*,*,#15857,.T.);
#21353=ORIENTED_EDGE('',*,*,#15858,.T.);
#21354=ORIENTED_EDGE('',*,*,#15855,.F.);
#21355=ORIENTED_EDGE('',*,*,#15854,.F.);
#21356=ORIENTED_EDGE('',*,*,#15497,.F.);
#21357=ORIENTED_EDGE('',*,*,#15859,.T.);
#21358=ORIENTED_EDGE('',*,*,#15857,.F.);
#21359=ORIENTED_EDGE('',*,*,#15860,.T.);
#21360=ORIENTED_EDGE('',*,*,#15488,.T.);
#21361=ORIENTED_EDGE('',*,*,#15660,.T.);
#21362=ORIENTED_EDGE('',*,*,#15861,.T.);
#21363=ORIENTED_EDGE('',*,*,#15862,.T.);
#21364=ORIENTED_EDGE('',*,*,#15861,.F.);
#21365=ORIENTED_EDGE('',*,*,#15659,.T.);
#21366=ORIENTED_EDGE('',*,*,#15863,.T.);
#21367=ORIENTED_EDGE('',*,*,#15658,.T.);
#21368=ORIENTED_EDGE('',*,*,#15492,.T.);
#21369=ORIENTED_EDGE('',*,*,#15864,.T.);
#21370=ORIENTED_EDGE('',*,*,#15863,.F.);
#21371=ORIENTED_EDGE('',*,*,#15860,.F.);
#21372=ORIENTED_EDGE('',*,*,#15865,.T.);
#21373=ORIENTED_EDGE('',*,*,#15866,.T.);
#21374=ORIENTED_EDGE('',*,*,#15489,.F.);
#21375=ORIENTED_EDGE('',*,*,#15862,.F.);
#21376=ORIENTED_EDGE('',*,*,#15867,.T.);
#21377=ORIENTED_EDGE('',*,*,#15868,.T.);
#21378=ORIENTED_EDGE('',*,*,#15865,.F.);
#21379=ORIENTED_EDGE('',*,*,#15864,.F.);
#21380=ORIENTED_EDGE('',*,*,#15491,.F.);
#21381=ORIENTED_EDGE('',*,*,#15869,.T.);
#21382=ORIENTED_EDGE('',*,*,#15867,.F.);
#21383=ORIENTED_EDGE('',*,*,#15870,.T.);
#21384=ORIENTED_EDGE('',*,*,#15482,.T.);
#21385=ORIENTED_EDGE('',*,*,#15663,.T.);
#21386=ORIENTED_EDGE('',*,*,#15871,.T.);
#21387=ORIENTED_EDGE('',*,*,#15872,.T.);
#21388=ORIENTED_EDGE('',*,*,#15871,.F.);
#21389=ORIENTED_EDGE('',*,*,#15662,.T.);
#21390=ORIENTED_EDGE('',*,*,#15873,.T.);
#21391=ORIENTED_EDGE('',*,*,#15661,.T.);
#21392=ORIENTED_EDGE('',*,*,#15486,.T.);
#21393=ORIENTED_EDGE('',*,*,#15874,.T.);
#21394=ORIENTED_EDGE('',*,*,#15873,.F.);
#21395=ORIENTED_EDGE('',*,*,#15870,.F.);
#21396=ORIENTED_EDGE('',*,*,#15875,.T.);
#21397=ORIENTED_EDGE('',*,*,#15876,.T.);
#21398=ORIENTED_EDGE('',*,*,#15483,.F.);
#21399=ORIENTED_EDGE('',*,*,#15872,.F.);
#21400=ORIENTED_EDGE('',*,*,#15877,.T.);
#21401=ORIENTED_EDGE('',*,*,#15878,.T.);
#21402=ORIENTED_EDGE('',*,*,#15875,.F.);
#21403=ORIENTED_EDGE('',*,*,#15874,.F.);
#21404=ORIENTED_EDGE('',*,*,#15485,.F.);
#21405=ORIENTED_EDGE('',*,*,#15879,.T.);
#21406=ORIENTED_EDGE('',*,*,#15877,.F.);
#21407=ORIENTED_EDGE('',*,*,#15880,.T.);
#21408=ORIENTED_EDGE('',*,*,#15476,.T.);
#21409=ORIENTED_EDGE('',*,*,#15666,.T.);
#21410=ORIENTED_EDGE('',*,*,#15881,.T.);
#21411=ORIENTED_EDGE('',*,*,#15882,.T.);
#21412=ORIENTED_EDGE('',*,*,#15881,.F.);
#21413=ORIENTED_EDGE('',*,*,#15665,.T.);
#21414=ORIENTED_EDGE('',*,*,#15883,.T.);
#21415=ORIENTED_EDGE('',*,*,#15664,.T.);
#21416=ORIENTED_EDGE('',*,*,#15480,.T.);
#21417=ORIENTED_EDGE('',*,*,#15884,.T.);
#21418=ORIENTED_EDGE('',*,*,#15883,.F.);
#21419=ORIENTED_EDGE('',*,*,#15880,.F.);
#21420=ORIENTED_EDGE('',*,*,#15885,.T.);
#21421=ORIENTED_EDGE('',*,*,#15886,.T.);
#21422=ORIENTED_EDGE('',*,*,#15477,.F.);
#21423=ORIENTED_EDGE('',*,*,#15882,.F.);
#21424=ORIENTED_EDGE('',*,*,#15887,.T.);
#21425=ORIENTED_EDGE('',*,*,#15888,.T.);
#21426=ORIENTED_EDGE('',*,*,#15885,.F.);
#21427=ORIENTED_EDGE('',*,*,#15884,.F.);
#21428=ORIENTED_EDGE('',*,*,#15479,.F.);
#21429=ORIENTED_EDGE('',*,*,#15889,.T.);
#21430=ORIENTED_EDGE('',*,*,#15887,.F.);
#21431=ORIENTED_EDGE('',*,*,#15890,.T.);
#21432=ORIENTED_EDGE('',*,*,#15470,.T.);
#21433=ORIENTED_EDGE('',*,*,#15669,.T.);
#21434=ORIENTED_EDGE('',*,*,#15891,.T.);
#21435=ORIENTED_EDGE('',*,*,#15892,.T.);
#21436=ORIENTED_EDGE('',*,*,#15891,.F.);
#21437=ORIENTED_EDGE('',*,*,#15668,.T.);
#21438=ORIENTED_EDGE('',*,*,#15893,.T.);
#21439=ORIENTED_EDGE('',*,*,#15667,.T.);
#21440=ORIENTED_EDGE('',*,*,#15474,.T.);
#21441=ORIENTED_EDGE('',*,*,#15894,.T.);
#21442=ORIENTED_EDGE('',*,*,#15893,.F.);
#21443=ORIENTED_EDGE('',*,*,#15890,.F.);
#21444=ORIENTED_EDGE('',*,*,#15895,.T.);
#21445=ORIENTED_EDGE('',*,*,#15896,.T.);
#21446=ORIENTED_EDGE('',*,*,#15471,.F.);
#21447=ORIENTED_EDGE('',*,*,#15892,.F.);
#21448=ORIENTED_EDGE('',*,*,#15897,.T.);
#21449=ORIENTED_EDGE('',*,*,#15898,.T.);
#21450=ORIENTED_EDGE('',*,*,#15895,.F.);
#21451=ORIENTED_EDGE('',*,*,#15894,.F.);
#21452=ORIENTED_EDGE('',*,*,#15473,.F.);
#21453=ORIENTED_EDGE('',*,*,#15899,.T.);
#21454=ORIENTED_EDGE('',*,*,#15897,.F.);
#21455=ORIENTED_EDGE('',*,*,#15900,.T.);
#21456=ORIENTED_EDGE('',*,*,#15464,.T.);
#21457=ORIENTED_EDGE('',*,*,#15672,.T.);
#21458=ORIENTED_EDGE('',*,*,#15901,.T.);
#21459=ORIENTED_EDGE('',*,*,#15902,.T.);
#21460=ORIENTED_EDGE('',*,*,#15901,.F.);
#21461=ORIENTED_EDGE('',*,*,#15671,.T.);
#21462=ORIENTED_EDGE('',*,*,#15903,.T.);
#21463=ORIENTED_EDGE('',*,*,#15670,.T.);
#21464=ORIENTED_EDGE('',*,*,#15468,.T.);
#21465=ORIENTED_EDGE('',*,*,#15904,.T.);
#21466=ORIENTED_EDGE('',*,*,#15903,.F.);
#21467=ORIENTED_EDGE('',*,*,#15900,.F.);
#21468=ORIENTED_EDGE('',*,*,#15905,.T.);
#21469=ORIENTED_EDGE('',*,*,#15906,.T.);
#21470=ORIENTED_EDGE('',*,*,#15465,.F.);
#21471=ORIENTED_EDGE('',*,*,#15902,.F.);
#21472=ORIENTED_EDGE('',*,*,#15907,.T.);
#21473=ORIENTED_EDGE('',*,*,#15908,.T.);
#21474=ORIENTED_EDGE('',*,*,#15905,.F.);
#21475=ORIENTED_EDGE('',*,*,#15904,.F.);
#21476=ORIENTED_EDGE('',*,*,#15467,.F.);
#21477=ORIENTED_EDGE('',*,*,#15909,.T.);
#21478=ORIENTED_EDGE('',*,*,#15907,.F.);
#21479=ORIENTED_EDGE('',*,*,#15910,.T.);
#21480=ORIENTED_EDGE('',*,*,#15458,.T.);
#21481=ORIENTED_EDGE('',*,*,#15675,.T.);
#21482=ORIENTED_EDGE('',*,*,#15911,.T.);
#21483=ORIENTED_EDGE('',*,*,#15912,.T.);
#21484=ORIENTED_EDGE('',*,*,#15911,.F.);
#21485=ORIENTED_EDGE('',*,*,#15674,.T.);
#21486=ORIENTED_EDGE('',*,*,#15913,.T.);
#21487=ORIENTED_EDGE('',*,*,#15673,.T.);
#21488=ORIENTED_EDGE('',*,*,#15462,.T.);
#21489=ORIENTED_EDGE('',*,*,#15914,.T.);
#21490=ORIENTED_EDGE('',*,*,#15913,.F.);
#21491=ORIENTED_EDGE('',*,*,#15910,.F.);
#21492=ORIENTED_EDGE('',*,*,#15915,.T.);
#21493=ORIENTED_EDGE('',*,*,#15916,.T.);
#21494=ORIENTED_EDGE('',*,*,#15459,.F.);
#21495=ORIENTED_EDGE('',*,*,#15912,.F.);
#21496=ORIENTED_EDGE('',*,*,#15917,.T.);
#21497=ORIENTED_EDGE('',*,*,#15918,.T.);
#21498=ORIENTED_EDGE('',*,*,#15915,.F.);
#21499=ORIENTED_EDGE('',*,*,#15914,.F.);
#21500=ORIENTED_EDGE('',*,*,#15461,.F.);
#21501=ORIENTED_EDGE('',*,*,#15919,.T.);
#21502=ORIENTED_EDGE('',*,*,#15917,.F.);
#21503=ORIENTED_EDGE('',*,*,#15920,.T.);
#21504=ORIENTED_EDGE('',*,*,#15452,.T.);
#21505=ORIENTED_EDGE('',*,*,#15678,.T.);
#21506=ORIENTED_EDGE('',*,*,#15921,.T.);
#21507=ORIENTED_EDGE('',*,*,#15922,.T.);
#21508=ORIENTED_EDGE('',*,*,#15921,.F.);
#21509=ORIENTED_EDGE('',*,*,#15677,.T.);
#21510=ORIENTED_EDGE('',*,*,#15923,.T.);
#21511=ORIENTED_EDGE('',*,*,#15676,.T.);
#21512=ORIENTED_EDGE('',*,*,#15456,.T.);
#21513=ORIENTED_EDGE('',*,*,#15924,.T.);
#21514=ORIENTED_EDGE('',*,*,#15923,.F.);
#21515=ORIENTED_EDGE('',*,*,#15920,.F.);
#21516=ORIENTED_EDGE('',*,*,#15925,.T.);
#21517=ORIENTED_EDGE('',*,*,#15926,.T.);
#21518=ORIENTED_EDGE('',*,*,#15453,.F.);
#21519=ORIENTED_EDGE('',*,*,#15922,.F.);
#21520=ORIENTED_EDGE('',*,*,#15927,.T.);
#21521=ORIENTED_EDGE('',*,*,#15928,.T.);
#21522=ORIENTED_EDGE('',*,*,#15925,.F.);
#21523=ORIENTED_EDGE('',*,*,#15924,.F.);
#21524=ORIENTED_EDGE('',*,*,#15455,.F.);
#21525=ORIENTED_EDGE('',*,*,#15929,.T.);
#21526=ORIENTED_EDGE('',*,*,#15927,.F.);
#21527=ORIENTED_EDGE('',*,*,#15930,.T.);
#21528=ORIENTED_EDGE('',*,*,#15931,.T.);
#21529=ORIENTED_EDGE('',*,*,#15932,.T.);
#21530=ORIENTED_EDGE('',*,*,#15933,.T.);
#21531=ORIENTED_EDGE('',*,*,#15934,.T.);
#21532=ORIENTED_EDGE('',*,*,#15355,.T.);
#21533=ORIENTED_EDGE('',*,*,#15935,.T.);
#21534=ORIENTED_EDGE('',*,*,#15933,.F.);
#21535=ORIENTED_EDGE('',*,*,#15936,.F.);
#21536=ORIENTED_EDGE('',*,*,#15930,.F.);
#21537=ORIENTED_EDGE('',*,*,#15935,.F.);
#21538=ORIENTED_EDGE('',*,*,#15354,.F.);
#21539=ORIENTED_EDGE('',*,*,#15937,.F.);
#21540=ORIENTED_EDGE('',*,*,#15938,.F.);
#21541=ORIENTED_EDGE('',*,*,#15939,.F.);
#21542=ORIENTED_EDGE('',*,*,#15348,.F.);
#21543=ORIENTED_EDGE('',*,*,#15940,.F.);
#21544=ORIENTED_EDGE('',*,*,#15941,.F.);
#21545=ORIENTED_EDGE('',*,*,#15942,.F.);
#21546=ORIENTED_EDGE('',*,*,#15342,.F.);
#21547=ORIENTED_EDGE('',*,*,#15943,.F.);
#21548=ORIENTED_EDGE('',*,*,#15944,.F.);
#21549=ORIENTED_EDGE('',*,*,#15945,.F.);
#21550=ORIENTED_EDGE('',*,*,#15336,.F.);
#21551=ORIENTED_EDGE('',*,*,#15946,.F.);
#21552=ORIENTED_EDGE('',*,*,#15947,.F.);
#21553=ORIENTED_EDGE('',*,*,#15948,.F.);
#21554=ORIENTED_EDGE('',*,*,#15330,.F.);
#21555=ORIENTED_EDGE('',*,*,#15949,.F.);
#21556=ORIENTED_EDGE('',*,*,#15950,.F.);
#21557=ORIENTED_EDGE('',*,*,#15951,.F.);
#21558=ORIENTED_EDGE('',*,*,#15324,.F.);
#21559=ORIENTED_EDGE('',*,*,#15952,.F.);
#21560=ORIENTED_EDGE('',*,*,#15953,.F.);
#21561=ORIENTED_EDGE('',*,*,#15954,.F.);
#21562=ORIENTED_EDGE('',*,*,#15318,.F.);
#21563=ORIENTED_EDGE('',*,*,#15955,.F.);
#21564=ORIENTED_EDGE('',*,*,#15956,.F.);
#21565=ORIENTED_EDGE('',*,*,#15957,.F.);
#21566=ORIENTED_EDGE('',*,*,#15312,.F.);
#21567=ORIENTED_EDGE('',*,*,#15958,.F.);
#21568=ORIENTED_EDGE('',*,*,#15959,.F.);
#21569=ORIENTED_EDGE('',*,*,#15960,.F.);
#21570=ORIENTED_EDGE('',*,*,#15306,.F.);
#21571=ORIENTED_EDGE('',*,*,#15961,.F.);
#21572=ORIENTED_EDGE('',*,*,#15962,.F.);
#21573=ORIENTED_EDGE('',*,*,#15963,.F.);
#21574=ORIENTED_EDGE('',*,*,#15300,.F.);
#21575=ORIENTED_EDGE('',*,*,#15964,.F.);
#21576=ORIENTED_EDGE('',*,*,#15965,.F.);
#21577=ORIENTED_EDGE('',*,*,#15966,.F.);
#21578=ORIENTED_EDGE('',*,*,#15294,.F.);
#21579=ORIENTED_EDGE('',*,*,#15967,.F.);
#21580=ORIENTED_EDGE('',*,*,#15968,.F.);
#21581=ORIENTED_EDGE('',*,*,#15969,.F.);
#21582=ORIENTED_EDGE('',*,*,#15288,.F.);
#21583=ORIENTED_EDGE('',*,*,#15970,.F.);
#21584=ORIENTED_EDGE('',*,*,#15971,.F.);
#21585=ORIENTED_EDGE('',*,*,#15972,.F.);
#21586=ORIENTED_EDGE('',*,*,#15282,.F.);
#21587=ORIENTED_EDGE('',*,*,#15973,.F.);
#21588=ORIENTED_EDGE('',*,*,#15974,.F.);
#21589=ORIENTED_EDGE('',*,*,#15975,.F.);
#21590=ORIENTED_EDGE('',*,*,#15276,.F.);
#21591=ORIENTED_EDGE('',*,*,#15976,.F.);
#21592=ORIENTED_EDGE('',*,*,#15977,.F.);
#21593=ORIENTED_EDGE('',*,*,#15978,.F.);
#21594=ORIENTED_EDGE('',*,*,#15270,.F.);
#21595=ORIENTED_EDGE('',*,*,#15979,.F.);
#21596=ORIENTED_EDGE('',*,*,#15980,.F.);
#21597=ORIENTED_EDGE('',*,*,#15981,.F.);
#21598=ORIENTED_EDGE('',*,*,#15264,.F.);
#21599=ORIENTED_EDGE('',*,*,#15982,.F.);
#21600=ORIENTED_EDGE('',*,*,#15983,.F.);
#21601=ORIENTED_EDGE('',*,*,#15984,.F.);
#21602=ORIENTED_EDGE('',*,*,#15258,.F.);
#21603=ORIENTED_EDGE('',*,*,#15985,.F.);
#21604=ORIENTED_EDGE('',*,*,#15986,.F.);
#21605=ORIENTED_EDGE('',*,*,#15987,.F.);
#21606=ORIENTED_EDGE('',*,*,#15252,.F.);
#21607=ORIENTED_EDGE('',*,*,#15988,.F.);
#21608=ORIENTED_EDGE('',*,*,#15989,.F.);
#21609=ORIENTED_EDGE('',*,*,#15990,.F.);
#21610=ORIENTED_EDGE('',*,*,#15246,.F.);
#21611=ORIENTED_EDGE('',*,*,#15991,.F.);
#21612=ORIENTED_EDGE('',*,*,#15992,.F.);
#21613=ORIENTED_EDGE('',*,*,#15993,.F.);
#21614=ORIENTED_EDGE('',*,*,#15240,.F.);
#21615=ORIENTED_EDGE('',*,*,#15994,.F.);
#21616=ORIENTED_EDGE('',*,*,#15995,.F.);
#21617=ORIENTED_EDGE('',*,*,#15996,.F.);
#21618=ORIENTED_EDGE('',*,*,#15234,.F.);
#21619=ORIENTED_EDGE('',*,*,#15997,.F.);
#21620=ORIENTED_EDGE('',*,*,#15998,.F.);
#21621=ORIENTED_EDGE('',*,*,#15999,.F.);
#21622=ORIENTED_EDGE('',*,*,#15228,.F.);
#21623=ORIENTED_EDGE('',*,*,#16000,.F.);
#21624=ORIENTED_EDGE('',*,*,#16001,.F.);
#21625=ORIENTED_EDGE('',*,*,#16002,.F.);
#21626=ORIENTED_EDGE('',*,*,#15222,.F.);
#21627=ORIENTED_EDGE('',*,*,#15402,.F.);
#21628=ORIENTED_EDGE('',*,*,#16003,.F.);
#21629=ORIENTED_EDGE('',*,*,#16004,.F.);
#21630=ORIENTED_EDGE('',*,*,#16005,.F.);
#21631=ORIENTED_EDGE('',*,*,#15396,.F.);
#21632=ORIENTED_EDGE('',*,*,#16006,.F.);
#21633=ORIENTED_EDGE('',*,*,#16007,.F.);
#21634=ORIENTED_EDGE('',*,*,#16008,.F.);
#21635=ORIENTED_EDGE('',*,*,#15390,.F.);
#21636=ORIENTED_EDGE('',*,*,#16009,.F.);
#21637=ORIENTED_EDGE('',*,*,#16010,.F.);
#21638=ORIENTED_EDGE('',*,*,#16011,.F.);
#21639=ORIENTED_EDGE('',*,*,#15384,.F.);
#21640=ORIENTED_EDGE('',*,*,#16012,.F.);
#21641=ORIENTED_EDGE('',*,*,#16013,.F.);
#21642=ORIENTED_EDGE('',*,*,#16014,.F.);
#21643=ORIENTED_EDGE('',*,*,#15378,.F.);
#21644=ORIENTED_EDGE('',*,*,#16015,.F.);
#21645=ORIENTED_EDGE('',*,*,#16016,.F.);
#21646=ORIENTED_EDGE('',*,*,#16017,.F.);
#21647=ORIENTED_EDGE('',*,*,#15372,.F.);
#21648=ORIENTED_EDGE('',*,*,#16018,.F.);
#21649=ORIENTED_EDGE('',*,*,#16019,.F.);
#21650=ORIENTED_EDGE('',*,*,#16020,.F.);
#21651=ORIENTED_EDGE('',*,*,#15366,.F.);
#21652=ORIENTED_EDGE('',*,*,#16021,.F.);
#21653=ORIENTED_EDGE('',*,*,#16022,.F.);
#21654=ORIENTED_EDGE('',*,*,#16023,.F.);
#21655=ORIENTED_EDGE('',*,*,#15360,.F.);
#21656=ORIENTED_EDGE('',*,*,#16024,.F.);
#21657=ORIENTED_EDGE('',*,*,#16025,.F.);
#21658=ORIENTED_EDGE('',*,*,#16026,.F.);
#21659=ORIENTED_EDGE('',*,*,#16027,.T.);
#21660=ORIENTED_EDGE('',*,*,#16028,.F.);
#21661=ORIENTED_EDGE('',*,*,#16029,.F.);
#21662=ORIENTED_EDGE('',*,*,#16030,.F.);
#21663=ORIENTED_EDGE('',*,*,#16031,.T.);
#21664=ORIENTED_EDGE('',*,*,#15359,.T.);
#21665=ORIENTED_EDGE('',*,*,#16032,.T.);
#21666=ORIENTED_EDGE('',*,*,#15931,.F.);
#21667=ORIENTED_EDGE('',*,*,#15936,.T.);
#21668=ORIENTED_EDGE('',*,*,#16022,.T.);
#21669=ORIENTED_EDGE('',*,*,#16033,.T.);
#21670=ORIENTED_EDGE('',*,*,#16034,.T.);
#21671=ORIENTED_EDGE('',*,*,#16035,.T.);
#21672=ORIENTED_EDGE('',*,*,#16021,.T.);
#21673=ORIENTED_EDGE('',*,*,#15365,.T.);
#21674=ORIENTED_EDGE('',*,*,#16036,.T.);
#21675=ORIENTED_EDGE('',*,*,#16033,.F.);
#21676=ORIENTED_EDGE('',*,*,#16037,.T.);
#21677=ORIENTED_EDGE('',*,*,#15361,.T.);
#21678=ORIENTED_EDGE('',*,*,#16023,.T.);
#21679=ORIENTED_EDGE('',*,*,#16035,.F.);
#21680=ORIENTED_EDGE('',*,*,#16019,.T.);
#21681=ORIENTED_EDGE('',*,*,#16038,.T.);
#21682=ORIENTED_EDGE('',*,*,#16039,.T.);
#21683=ORIENTED_EDGE('',*,*,#16040,.T.);
#21684=ORIENTED_EDGE('',*,*,#16018,.T.);
#21685=ORIENTED_EDGE('',*,*,#15371,.T.);
#21686=ORIENTED_EDGE('',*,*,#16041,.T.);
#21687=ORIENTED_EDGE('',*,*,#16038,.F.);
#21688=ORIENTED_EDGE('',*,*,#16042,.T.);
#21689=ORIENTED_EDGE('',*,*,#15367,.T.);
#21690=ORIENTED_EDGE('',*,*,#16020,.T.);
#21691=ORIENTED_EDGE('',*,*,#16040,.F.);
#21692=ORIENTED_EDGE('',*,*,#16042,.F.);
#21693=ORIENTED_EDGE('',*,*,#16043,.T.);
#21694=ORIENTED_EDGE('',*,*,#16044,.T.);
#21695=ORIENTED_EDGE('',*,*,#15368,.F.);
#21696=ORIENTED_EDGE('',*,*,#16039,.F.);
#21697=ORIENTED_EDGE('',*,*,#16045,.T.);
#21698=ORIENTED_EDGE('',*,*,#16046,.T.);
#21699=ORIENTED_EDGE('',*,*,#16043,.F.);
#21700=ORIENTED_EDGE('',*,*,#16016,.T.);
#21701=ORIENTED_EDGE('',*,*,#16047,.T.);
#21702=ORIENTED_EDGE('',*,*,#16048,.T.);
#21703=ORIENTED_EDGE('',*,*,#16049,.T.);
#21704=ORIENTED_EDGE('',*,*,#16015,.T.);
#21705=ORIENTED_EDGE('',*,*,#15377,.T.);
#21706=ORIENTED_EDGE('',*,*,#16050,.T.);
#21707=ORIENTED_EDGE('',*,*,#16047,.F.);
#21708=ORIENTED_EDGE('',*,*,#16051,.T.);
#21709=ORIENTED_EDGE('',*,*,#15373,.T.);
#21710=ORIENTED_EDGE('',*,*,#16017,.T.);
#21711=ORIENTED_EDGE('',*,*,#16049,.F.);
#21712=ORIENTED_EDGE('',*,*,#16013,.T.);
#21713=ORIENTED_EDGE('',*,*,#16052,.T.);
#21714=ORIENTED_EDGE('',*,*,#16053,.T.);
#21715=ORIENTED_EDGE('',*,*,#16054,.T.);
#21716=ORIENTED_EDGE('',*,*,#16012,.T.);
#21717=ORIENTED_EDGE('',*,*,#15383,.T.);
#21718=ORIENTED_EDGE('',*,*,#16055,.T.);
#21719=ORIENTED_EDGE('',*,*,#16052,.F.);
#21720=ORIENTED_EDGE('',*,*,#16056,.T.);
#21721=ORIENTED_EDGE('',*,*,#15379,.T.);
#21722=ORIENTED_EDGE('',*,*,#16014,.T.);
#21723=ORIENTED_EDGE('',*,*,#16054,.F.);
#21724=ORIENTED_EDGE('',*,*,#16056,.F.);
#21725=ORIENTED_EDGE('',*,*,#16057,.T.);
#21726=ORIENTED_EDGE('',*,*,#16058,.T.);
#21727=ORIENTED_EDGE('',*,*,#15380,.F.);
#21728=ORIENTED_EDGE('',*,*,#16053,.F.);
#21729=ORIENTED_EDGE('',*,*,#16059,.T.);
#21730=ORIENTED_EDGE('',*,*,#16060,.T.);
#21731=ORIENTED_EDGE('',*,*,#16057,.F.);
#21732=ORIENTED_EDGE('',*,*,#16010,.T.);
#21733=ORIENTED_EDGE('',*,*,#16061,.T.);
#21734=ORIENTED_EDGE('',*,*,#16062,.T.);
#21735=ORIENTED_EDGE('',*,*,#16063,.T.);
#21736=ORIENTED_EDGE('',*,*,#16009,.T.);
#21737=ORIENTED_EDGE('',*,*,#15389,.T.);
#21738=ORIENTED_EDGE('',*,*,#16064,.T.);
#21739=ORIENTED_EDGE('',*,*,#16061,.F.);
#21740=ORIENTED_EDGE('',*,*,#16065,.T.);
#21741=ORIENTED_EDGE('',*,*,#15385,.T.);
#21742=ORIENTED_EDGE('',*,*,#16011,.T.);
#21743=ORIENTED_EDGE('',*,*,#16063,.F.);
#21744=ORIENTED_EDGE('',*,*,#16007,.T.);
#21745=ORIENTED_EDGE('',*,*,#16066,.T.);
#21746=ORIENTED_EDGE('',*,*,#16067,.T.);
#21747=ORIENTED_EDGE('',*,*,#16068,.T.);
#21748=ORIENTED_EDGE('',*,*,#16006,.T.);
#21749=ORIENTED_EDGE('',*,*,#15395,.T.);
#21750=ORIENTED_EDGE('',*,*,#16069,.T.);
#21751=ORIENTED_EDGE('',*,*,#16066,.F.);
#21752=ORIENTED_EDGE('',*,*,#16070,.T.);
#21753=ORIENTED_EDGE('',*,*,#15391,.T.);
#21754=ORIENTED_EDGE('',*,*,#16008,.T.);
#21755=ORIENTED_EDGE('',*,*,#16068,.F.);
#21756=ORIENTED_EDGE('',*,*,#16070,.F.);
#21757=ORIENTED_EDGE('',*,*,#16071,.T.);
#21758=ORIENTED_EDGE('',*,*,#16072,.T.);
#21759=ORIENTED_EDGE('',*,*,#15392,.F.);
#21760=ORIENTED_EDGE('',*,*,#16067,.F.);
#21761=ORIENTED_EDGE('',*,*,#16073,.T.);
#21762=ORIENTED_EDGE('',*,*,#16074,.T.);
#21763=ORIENTED_EDGE('',*,*,#16071,.F.);
#21764=ORIENTED_EDGE('',*,*,#15397,.T.);
#21765=ORIENTED_EDGE('',*,*,#16005,.T.);
#21766=ORIENTED_EDGE('',*,*,#16075,.T.);
#21767=ORIENTED_EDGE('',*,*,#16076,.T.);
#21768=ORIENTED_EDGE('',*,*,#16077,.T.);
#21769=ORIENTED_EDGE('',*,*,#16075,.F.);
#21770=ORIENTED_EDGE('',*,*,#16004,.T.);
#21771=ORIENTED_EDGE('',*,*,#16078,.T.);
#21772=ORIENTED_EDGE('',*,*,#16003,.T.);
#21773=ORIENTED_EDGE('',*,*,#15401,.T.);
#21774=ORIENTED_EDGE('',*,*,#16079,.T.);
#21775=ORIENTED_EDGE('',*,*,#16078,.F.);
#21776=ORIENTED_EDGE('',*,*,#16001,.T.);
#21777=ORIENTED_EDGE('',*,*,#16080,.T.);
#21778=ORIENTED_EDGE('',*,*,#16081,.T.);
#21779=ORIENTED_EDGE('',*,*,#16082,.T.);
#21780=ORIENTED_EDGE('',*,*,#16000,.T.);
#21781=ORIENTED_EDGE('',*,*,#15227,.T.);
#21782=ORIENTED_EDGE('',*,*,#16083,.T.);
#21783=ORIENTED_EDGE('',*,*,#16080,.F.);
#21784=ORIENTED_EDGE('',*,*,#16084,.T.);
#21785=ORIENTED_EDGE('',*,*,#15223,.T.);
#21786=ORIENTED_EDGE('',*,*,#16002,.T.);
#21787=ORIENTED_EDGE('',*,*,#16082,.F.);
#21788=ORIENTED_EDGE('',*,*,#15998,.T.);
#21789=ORIENTED_EDGE('',*,*,#16085,.T.);
#21790=ORIENTED_EDGE('',*,*,#16086,.T.);
#21791=ORIENTED_EDGE('',*,*,#16087,.T.);
#21792=ORIENTED_EDGE('',*,*,#15997,.T.);
#21793=ORIENTED_EDGE('',*,*,#15233,.T.);
#21794=ORIENTED_EDGE('',*,*,#16088,.T.);
#21795=ORIENTED_EDGE('',*,*,#16085,.F.);
#21796=ORIENTED_EDGE('',*,*,#16089,.T.);
#21797=ORIENTED_EDGE('',*,*,#15229,.T.);
#21798=ORIENTED_EDGE('',*,*,#15999,.T.);
#21799=ORIENTED_EDGE('',*,*,#16087,.F.);
#21800=ORIENTED_EDGE('',*,*,#16089,.F.);
#21801=ORIENTED_EDGE('',*,*,#16090,.T.);
#21802=ORIENTED_EDGE('',*,*,#16091,.T.);
#21803=ORIENTED_EDGE('',*,*,#15230,.F.);
#21804=ORIENTED_EDGE('',*,*,#16086,.F.);
#21805=ORIENTED_EDGE('',*,*,#16092,.T.);
#21806=ORIENTED_EDGE('',*,*,#16093,.T.);
#21807=ORIENTED_EDGE('',*,*,#16090,.F.);
#21808=ORIENTED_EDGE('',*,*,#15995,.T.);
#21809=ORIENTED_EDGE('',*,*,#16094,.T.);
#21810=ORIENTED_EDGE('',*,*,#16095,.T.);
#21811=ORIENTED_EDGE('',*,*,#16096,.T.);
#21812=ORIENTED_EDGE('',*,*,#15994,.T.);
#21813=ORIENTED_EDGE('',*,*,#15239,.T.);
#21814=ORIENTED_EDGE('',*,*,#16097,.T.);
#21815=ORIENTED_EDGE('',*,*,#16094,.F.);
#21816=ORIENTED_EDGE('',*,*,#16098,.T.);
#21817=ORIENTED_EDGE('',*,*,#15235,.T.);
#21818=ORIENTED_EDGE('',*,*,#15996,.T.);
#21819=ORIENTED_EDGE('',*,*,#16096,.F.);
#21820=ORIENTED_EDGE('',*,*,#15992,.T.);
#21821=ORIENTED_EDGE('',*,*,#16099,.T.);
#21822=ORIENTED_EDGE('',*,*,#16100,.T.);
#21823=ORIENTED_EDGE('',*,*,#16101,.T.);
#21824=ORIENTED_EDGE('',*,*,#15991,.T.);
#21825=ORIENTED_EDGE('',*,*,#15245,.T.);
#21826=ORIENTED_EDGE('',*,*,#16102,.T.);
#21827=ORIENTED_EDGE('',*,*,#16099,.F.);
#21828=ORIENTED_EDGE('',*,*,#16103,.T.);
#21829=ORIENTED_EDGE('',*,*,#15241,.T.);
#21830=ORIENTED_EDGE('',*,*,#15993,.T.);
#21831=ORIENTED_EDGE('',*,*,#16101,.F.);
#21832=ORIENTED_EDGE('',*,*,#16103,.F.);
#21833=ORIENTED_EDGE('',*,*,#16104,.T.);
#21834=ORIENTED_EDGE('',*,*,#16105,.T.);
#21835=ORIENTED_EDGE('',*,*,#15242,.F.);
#21836=ORIENTED_EDGE('',*,*,#16100,.F.);
#21837=ORIENTED_EDGE('',*,*,#16106,.T.);
#21838=ORIENTED_EDGE('',*,*,#16107,.T.);
#21839=ORIENTED_EDGE('',*,*,#16104,.F.);
#21840=ORIENTED_EDGE('',*,*,#15989,.T.);
#21841=ORIENTED_EDGE('',*,*,#16108,.T.);
#21842=ORIENTED_EDGE('',*,*,#16109,.T.);
#21843=ORIENTED_EDGE('',*,*,#16110,.T.);
#21844=ORIENTED_EDGE('',*,*,#15988,.T.);
#21845=ORIENTED_EDGE('',*,*,#15251,.T.);
#21846=ORIENTED_EDGE('',*,*,#16111,.T.);
#21847=ORIENTED_EDGE('',*,*,#16108,.F.);
#21848=ORIENTED_EDGE('',*,*,#16112,.T.);
#21849=ORIENTED_EDGE('',*,*,#15247,.T.);
#21850=ORIENTED_EDGE('',*,*,#15990,.T.);
#21851=ORIENTED_EDGE('',*,*,#16110,.F.);
#21852=ORIENTED_EDGE('',*,*,#15986,.T.);
#21853=ORIENTED_EDGE('',*,*,#16113,.T.);
#21854=ORIENTED_EDGE('',*,*,#16114,.T.);
#21855=ORIENTED_EDGE('',*,*,#16115,.T.);
#21856=ORIENTED_EDGE('',*,*,#15985,.T.);
#21857=ORIENTED_EDGE('',*,*,#15257,.T.);
#21858=ORIENTED_EDGE('',*,*,#16116,.T.);
#21859=ORIENTED_EDGE('',*,*,#16113,.F.);
#21860=ORIENTED_EDGE('',*,*,#16117,.T.);
#21861=ORIENTED_EDGE('',*,*,#15253,.T.);
#21862=ORIENTED_EDGE('',*,*,#15987,.T.);
#21863=ORIENTED_EDGE('',*,*,#16115,.F.);
#21864=ORIENTED_EDGE('',*,*,#16117,.F.);
#21865=ORIENTED_EDGE('',*,*,#16118,.T.);
#21866=ORIENTED_EDGE('',*,*,#16119,.T.);
#21867=ORIENTED_EDGE('',*,*,#15254,.F.);
#21868=ORIENTED_EDGE('',*,*,#16114,.F.);
#21869=ORIENTED_EDGE('',*,*,#16120,.T.);
#21870=ORIENTED_EDGE('',*,*,#16121,.T.);
#21871=ORIENTED_EDGE('',*,*,#16118,.F.);
#21872=ORIENTED_EDGE('',*,*,#15983,.T.);
#21873=ORIENTED_EDGE('',*,*,#16122,.T.);
#21874=ORIENTED_EDGE('',*,*,#16123,.T.);
#21875=ORIENTED_EDGE('',*,*,#16124,.T.);
#21876=ORIENTED_EDGE('',*,*,#15982,.T.);
#21877=ORIENTED_EDGE('',*,*,#15263,.T.);
#21878=ORIENTED_EDGE('',*,*,#16125,.T.);
#21879=ORIENTED_EDGE('',*,*,#16122,.F.);
#21880=ORIENTED_EDGE('',*,*,#16126,.T.);
#21881=ORIENTED_EDGE('',*,*,#15259,.T.);
#21882=ORIENTED_EDGE('',*,*,#15984,.T.);
#21883=ORIENTED_EDGE('',*,*,#16124,.F.);
#21884=ORIENTED_EDGE('',*,*,#15980,.T.);
#21885=ORIENTED_EDGE('',*,*,#16127,.T.);
#21886=ORIENTED_EDGE('',*,*,#16128,.T.);
#21887=ORIENTED_EDGE('',*,*,#16129,.T.);
#21888=ORIENTED_EDGE('',*,*,#15979,.T.);
#21889=ORIENTED_EDGE('',*,*,#15269,.T.);
#21890=ORIENTED_EDGE('',*,*,#16130,.T.);
#21891=ORIENTED_EDGE('',*,*,#16127,.F.);
#21892=ORIENTED_EDGE('',*,*,#16131,.T.);
#21893=ORIENTED_EDGE('',*,*,#15265,.T.);
#21894=ORIENTED_EDGE('',*,*,#15981,.T.);
#21895=ORIENTED_EDGE('',*,*,#16129,.F.);
#21896=ORIENTED_EDGE('',*,*,#16131,.F.);
#21897=ORIENTED_EDGE('',*,*,#16132,.T.);
#21898=ORIENTED_EDGE('',*,*,#16133,.T.);
#21899=ORIENTED_EDGE('',*,*,#15266,.F.);
#21900=ORIENTED_EDGE('',*,*,#16128,.F.);
#21901=ORIENTED_EDGE('',*,*,#16134,.T.);
#21902=ORIENTED_EDGE('',*,*,#16135,.T.);
#21903=ORIENTED_EDGE('',*,*,#16132,.F.);
#21904=ORIENTED_EDGE('',*,*,#15977,.T.);
#21905=ORIENTED_EDGE('',*,*,#16136,.T.);
#21906=ORIENTED_EDGE('',*,*,#16137,.T.);
#21907=ORIENTED_EDGE('',*,*,#16138,.T.);
#21908=ORIENTED_EDGE('',*,*,#15976,.T.);
#21909=ORIENTED_EDGE('',*,*,#15275,.T.);
#21910=ORIENTED_EDGE('',*,*,#16139,.T.);
#21911=ORIENTED_EDGE('',*,*,#16136,.F.);
#21912=ORIENTED_EDGE('',*,*,#16140,.T.);
#21913=ORIENTED_EDGE('',*,*,#15271,.T.);
#21914=ORIENTED_EDGE('',*,*,#15978,.T.);
#21915=ORIENTED_EDGE('',*,*,#16138,.F.);
#21916=ORIENTED_EDGE('',*,*,#15974,.T.);
#21917=ORIENTED_EDGE('',*,*,#16141,.T.);
#21918=ORIENTED_EDGE('',*,*,#16142,.T.);
#21919=ORIENTED_EDGE('',*,*,#16143,.T.);
#21920=ORIENTED_EDGE('',*,*,#15973,.T.);
#21921=ORIENTED_EDGE('',*,*,#15281,.T.);
#21922=ORIENTED_EDGE('',*,*,#16144,.T.);
#21923=ORIENTED_EDGE('',*,*,#16141,.F.);
#21924=ORIENTED_EDGE('',*,*,#16145,.T.);
#21925=ORIENTED_EDGE('',*,*,#15277,.T.);
#21926=ORIENTED_EDGE('',*,*,#15975,.T.);
#21927=ORIENTED_EDGE('',*,*,#16143,.F.);
#21928=ORIENTED_EDGE('',*,*,#16145,.F.);
#21929=ORIENTED_EDGE('',*,*,#16146,.T.);
#21930=ORIENTED_EDGE('',*,*,#16147,.T.);
#21931=ORIENTED_EDGE('',*,*,#15278,.F.);
#21932=ORIENTED_EDGE('',*,*,#16142,.F.);
#21933=ORIENTED_EDGE('',*,*,#16148,.T.);
#21934=ORIENTED_EDGE('',*,*,#16149,.T.);
#21935=ORIENTED_EDGE('',*,*,#16146,.F.);
#21936=ORIENTED_EDGE('',*,*,#15971,.T.);
#21937=ORIENTED_EDGE('',*,*,#16150,.T.);
#21938=ORIENTED_EDGE('',*,*,#16151,.T.);
#21939=ORIENTED_EDGE('',*,*,#16152,.T.);
#21940=ORIENTED_EDGE('',*,*,#15970,.T.);
#21941=ORIENTED_EDGE('',*,*,#15287,.T.);
#21942=ORIENTED_EDGE('',*,*,#16153,.T.);
#21943=ORIENTED_EDGE('',*,*,#16150,.F.);
#21944=ORIENTED_EDGE('',*,*,#16154,.T.);
#21945=ORIENTED_EDGE('',*,*,#15283,.T.);
#21946=ORIENTED_EDGE('',*,*,#15972,.T.);
#21947=ORIENTED_EDGE('',*,*,#16152,.F.);
#21948=ORIENTED_EDGE('',*,*,#15968,.T.);
#21949=ORIENTED_EDGE('',*,*,#16155,.T.);
#21950=ORIENTED_EDGE('',*,*,#16156,.T.);
#21951=ORIENTED_EDGE('',*,*,#16157,.T.);
#21952=ORIENTED_EDGE('',*,*,#15967,.T.);
#21953=ORIENTED_EDGE('',*,*,#15293,.T.);
#21954=ORIENTED_EDGE('',*,*,#16158,.T.);
#21955=ORIENTED_EDGE('',*,*,#16155,.F.);
#21956=ORIENTED_EDGE('',*,*,#16159,.T.);
#21957=ORIENTED_EDGE('',*,*,#15289,.T.);
#21958=ORIENTED_EDGE('',*,*,#15969,.T.);
#21959=ORIENTED_EDGE('',*,*,#16157,.F.);
#21960=ORIENTED_EDGE('',*,*,#16159,.F.);
#21961=ORIENTED_EDGE('',*,*,#16160,.T.);
#21962=ORIENTED_EDGE('',*,*,#16161,.T.);
#21963=ORIENTED_EDGE('',*,*,#15290,.F.);
#21964=ORIENTED_EDGE('',*,*,#16156,.F.);
#21965=ORIENTED_EDGE('',*,*,#16162,.T.);
#21966=ORIENTED_EDGE('',*,*,#16163,.T.);
#21967=ORIENTED_EDGE('',*,*,#16160,.F.);
#21968=ORIENTED_EDGE('',*,*,#15965,.T.);
#21969=ORIENTED_EDGE('',*,*,#16164,.T.);
#21970=ORIENTED_EDGE('',*,*,#16165,.T.);
#21971=ORIENTED_EDGE('',*,*,#16166,.T.);
#21972=ORIENTED_EDGE('',*,*,#16167,.T.);
#21973=ORIENTED_EDGE('',*,*,#15295,.T.);
#21974=ORIENTED_EDGE('',*,*,#15966,.T.);
#21975=ORIENTED_EDGE('',*,*,#16166,.F.);
#21976=ORIENTED_EDGE('',*,*,#15299,.T.);
#21977=ORIENTED_EDGE('',*,*,#16168,.T.);
#21978=ORIENTED_EDGE('',*,*,#16164,.F.);
#21979=ORIENTED_EDGE('',*,*,#15964,.T.);
#21980=ORIENTED_EDGE('',*,*,#15962,.T.);
#21981=ORIENTED_EDGE('',*,*,#16169,.T.);
#21982=ORIENTED_EDGE('',*,*,#16170,.T.);
#21983=ORIENTED_EDGE('',*,*,#16171,.T.);
#21984=ORIENTED_EDGE('',*,*,#15961,.T.);
#21985=ORIENTED_EDGE('',*,*,#15305,.T.);
#21986=ORIENTED_EDGE('',*,*,#16172,.T.);
#21987=ORIENTED_EDGE('',*,*,#16169,.F.);
#21988=ORIENTED_EDGE('',*,*,#16173,.T.);
#21989=ORIENTED_EDGE('',*,*,#15301,.T.);
#21990=ORIENTED_EDGE('',*,*,#15963,.T.);
#21991=ORIENTED_EDGE('',*,*,#16171,.F.);
#21992=ORIENTED_EDGE('',*,*,#15959,.T.);
#21993=ORIENTED_EDGE('',*,*,#16174,.T.);
#21994=ORIENTED_EDGE('',*,*,#16175,.T.);
#21995=ORIENTED_EDGE('',*,*,#16176,.T.);
#21996=ORIENTED_EDGE('',*,*,#15958,.T.);
#21997=ORIENTED_EDGE('',*,*,#15311,.T.);
#21998=ORIENTED_EDGE('',*,*,#16177,.T.);
#21999=ORIENTED_EDGE('',*,*,#16174,.F.);
#22000=ORIENTED_EDGE('',*,*,#16178,.T.);
#22001=ORIENTED_EDGE('',*,*,#15307,.T.);
#22002=ORIENTED_EDGE('',*,*,#15960,.T.);
#22003=ORIENTED_EDGE('',*,*,#16176,.F.);
#22004=ORIENTED_EDGE('',*,*,#16178,.F.);
#22005=ORIENTED_EDGE('',*,*,#16179,.T.);
#22006=ORIENTED_EDGE('',*,*,#16180,.T.);
#22007=ORIENTED_EDGE('',*,*,#15308,.F.);
#22008=ORIENTED_EDGE('',*,*,#16175,.F.);
#22009=ORIENTED_EDGE('',*,*,#16181,.T.);
#22010=ORIENTED_EDGE('',*,*,#16182,.T.);
#22011=ORIENTED_EDGE('',*,*,#16179,.F.);
#22012=ORIENTED_EDGE('',*,*,#15956,.T.);
#22013=ORIENTED_EDGE('',*,*,#16183,.T.);
#22014=ORIENTED_EDGE('',*,*,#16184,.T.);
#22015=ORIENTED_EDGE('',*,*,#16185,.T.);
#22016=ORIENTED_EDGE('',*,*,#15955,.T.);
#22017=ORIENTED_EDGE('',*,*,#15317,.T.);
#22018=ORIENTED_EDGE('',*,*,#16186,.T.);
#22019=ORIENTED_EDGE('',*,*,#16183,.F.);
#22020=ORIENTED_EDGE('',*,*,#16187,.T.);
#22021=ORIENTED_EDGE('',*,*,#15313,.T.);
#22022=ORIENTED_EDGE('',*,*,#15957,.T.);
#22023=ORIENTED_EDGE('',*,*,#16185,.F.);
#22024=ORIENTED_EDGE('',*,*,#15953,.T.);
#22025=ORIENTED_EDGE('',*,*,#16188,.T.);
#22026=ORIENTED_EDGE('',*,*,#16189,.T.);
#22027=ORIENTED_EDGE('',*,*,#16190,.T.);
#22028=ORIENTED_EDGE('',*,*,#15952,.T.);
#22029=ORIENTED_EDGE('',*,*,#15323,.T.);
#22030=ORIENTED_EDGE('',*,*,#16191,.T.);
#22031=ORIENTED_EDGE('',*,*,#16188,.F.);
#22032=ORIENTED_EDGE('',*,*,#16192,.T.);
#22033=ORIENTED_EDGE('',*,*,#15319,.T.);
#22034=ORIENTED_EDGE('',*,*,#15954,.T.);
#22035=ORIENTED_EDGE('',*,*,#16190,.F.);
#22036=ORIENTED_EDGE('',*,*,#16192,.F.);
#22037=ORIENTED_EDGE('',*,*,#16193,.T.);
#22038=ORIENTED_EDGE('',*,*,#16194,.T.);
#22039=ORIENTED_EDGE('',*,*,#15320,.F.);
#22040=ORIENTED_EDGE('',*,*,#16189,.F.);
#22041=ORIENTED_EDGE('',*,*,#16195,.T.);
#22042=ORIENTED_EDGE('',*,*,#16196,.T.);
#22043=ORIENTED_EDGE('',*,*,#16193,.F.);
#22044=ORIENTED_EDGE('',*,*,#15950,.T.);
#22045=ORIENTED_EDGE('',*,*,#16197,.T.);
#22046=ORIENTED_EDGE('',*,*,#16198,.T.);
#22047=ORIENTED_EDGE('',*,*,#16199,.T.);
#22048=ORIENTED_EDGE('',*,*,#15949,.T.);
#22049=ORIENTED_EDGE('',*,*,#15329,.T.);
#22050=ORIENTED_EDGE('',*,*,#16200,.T.);
#22051=ORIENTED_EDGE('',*,*,#16197,.F.);
#22052=ORIENTED_EDGE('',*,*,#16201,.T.);
#22053=ORIENTED_EDGE('',*,*,#15325,.T.);
#22054=ORIENTED_EDGE('',*,*,#15951,.T.);
#22055=ORIENTED_EDGE('',*,*,#16199,.F.);
#22056=ORIENTED_EDGE('',*,*,#15947,.T.);
#22057=ORIENTED_EDGE('',*,*,#16202,.T.);
#22058=ORIENTED_EDGE('',*,*,#16203,.T.);
#22059=ORIENTED_EDGE('',*,*,#16204,.T.);
#22060=ORIENTED_EDGE('',*,*,#15946,.T.);
#22061=ORIENTED_EDGE('',*,*,#15335,.T.);
#22062=ORIENTED_EDGE('',*,*,#16205,.T.);
#22063=ORIENTED_EDGE('',*,*,#16202,.F.);
#22064=ORIENTED_EDGE('',*,*,#16206,.T.);
#22065=ORIENTED_EDGE('',*,*,#15331,.T.);
#22066=ORIENTED_EDGE('',*,*,#15948,.T.);
#22067=ORIENTED_EDGE('',*,*,#16204,.F.);
#22068=ORIENTED_EDGE('',*,*,#16206,.F.);
#22069=ORIENTED_EDGE('',*,*,#16207,.T.);
#22070=ORIENTED_EDGE('',*,*,#16208,.T.);
#22071=ORIENTED_EDGE('',*,*,#15332,.F.);
#22072=ORIENTED_EDGE('',*,*,#16203,.F.);
#22073=ORIENTED_EDGE('',*,*,#16209,.T.);
#22074=ORIENTED_EDGE('',*,*,#16210,.T.);
#22075=ORIENTED_EDGE('',*,*,#16207,.F.);
#22076=ORIENTED_EDGE('',*,*,#15337,.T.);
#22077=ORIENTED_EDGE('',*,*,#15945,.T.);
#22078=ORIENTED_EDGE('',*,*,#16211,.T.);
#22079=ORIENTED_EDGE('',*,*,#16212,.T.);
#22080=ORIENTED_EDGE('',*,*,#16213,.T.);
#22081=ORIENTED_EDGE('',*,*,#16211,.F.);
#22082=ORIENTED_EDGE('',*,*,#15944,.T.);
#22083=ORIENTED_EDGE('',*,*,#16214,.T.);
#22084=ORIENTED_EDGE('',*,*,#15943,.T.);
#22085=ORIENTED_EDGE('',*,*,#15341,.T.);
#22086=ORIENTED_EDGE('',*,*,#16215,.T.);
#22087=ORIENTED_EDGE('',*,*,#16214,.F.);
#22088=ORIENTED_EDGE('',*,*,#15941,.T.);
#22089=ORIENTED_EDGE('',*,*,#16216,.T.);
#22090=ORIENTED_EDGE('',*,*,#16217,.T.);
#22091=ORIENTED_EDGE('',*,*,#16218,.T.);
#22092=ORIENTED_EDGE('',*,*,#15940,.T.);
#22093=ORIENTED_EDGE('',*,*,#15347,.T.);
#22094=ORIENTED_EDGE('',*,*,#16219,.T.);
#22095=ORIENTED_EDGE('',*,*,#16216,.F.);
#22096=ORIENTED_EDGE('',*,*,#16220,.T.);
#22097=ORIENTED_EDGE('',*,*,#15343,.T.);
#22098=ORIENTED_EDGE('',*,*,#15942,.T.);
#22099=ORIENTED_EDGE('',*,*,#16218,.F.);
#22100=ORIENTED_EDGE('',*,*,#15938,.T.);
#22101=ORIENTED_EDGE('',*,*,#16221,.T.);
#22102=ORIENTED_EDGE('',*,*,#16222,.T.);
#22103=ORIENTED_EDGE('',*,*,#16223,.T.);
#22104=ORIENTED_EDGE('',*,*,#15937,.T.);
#22105=ORIENTED_EDGE('',*,*,#15353,.T.);
#22106=ORIENTED_EDGE('',*,*,#16224,.T.);
#22107=ORIENTED_EDGE('',*,*,#16221,.F.);
#22108=ORIENTED_EDGE('',*,*,#16225,.T.);
#22109=ORIENTED_EDGE('',*,*,#15349,.T.);
#22110=ORIENTED_EDGE('',*,*,#15939,.T.);
#22111=ORIENTED_EDGE('',*,*,#16223,.F.);
#22112=ORIENTED_EDGE('',*,*,#16225,.F.);
#22113=ORIENTED_EDGE('',*,*,#16226,.T.);
#22114=ORIENTED_EDGE('',*,*,#16227,.T.);
#22115=ORIENTED_EDGE('',*,*,#15350,.F.);
#22116=ORIENTED_EDGE('',*,*,#16222,.F.);
#22117=ORIENTED_EDGE('',*,*,#16228,.T.);
#22118=ORIENTED_EDGE('',*,*,#16229,.T.);
#22119=ORIENTED_EDGE('',*,*,#16226,.F.);
#22120=ORIENTED_EDGE('',*,*,#15704,.T.);
#22121=ORIENTED_EDGE('',*,*,#16230,.T.);
#22122=ORIENTED_EDGE('',*,*,#16231,.T.);
#22123=ORIENTED_EDGE('',*,*,#16232,.T.);
#22124=ORIENTED_EDGE('',*,*,#15703,.T.);
#22125=ORIENTED_EDGE('',*,*,#16233,.T.);
#22126=ORIENTED_EDGE('',*,*,#16234,.T.);
#22127=ORIENTED_EDGE('',*,*,#16230,.F.);
#22128=ORIENTED_EDGE('',*,*,#16235,.T.);
#22129=ORIENTED_EDGE('',*,*,#16236,.T.);
#22130=ORIENTED_EDGE('',*,*,#15697,.T.);
#22131=ORIENTED_EDGE('',*,*,#16232,.F.);
#22132=ORIENTED_EDGE('',*,*,#16235,.F.);
#22133=ORIENTED_EDGE('',*,*,#16237,.F.);
#22134=ORIENTED_EDGE('',*,*,#16238,.F.);
#22135=ORIENTED_EDGE('',*,*,#16239,.F.);
#22136=ORIENTED_EDGE('',*,*,#16231,.F.);
#22137=ORIENTED_EDGE('',*,*,#16240,.F.);
#22138=ORIENTED_EDGE('',*,*,#16241,.F.);
#22139=ORIENTED_EDGE('',*,*,#16237,.T.);
#22140=ORIENTED_EDGE('',*,*,#16234,.F.);
#22141=ORIENTED_EDGE('',*,*,#16242,.F.);
#22142=ORIENTED_EDGE('',*,*,#16243,.F.);
#22143=ORIENTED_EDGE('',*,*,#16240,.T.);
#22144=ORIENTED_EDGE('',*,*,#16233,.F.);
#22145=ORIENTED_EDGE('',*,*,#15702,.T.);
#22146=ORIENTED_EDGE('',*,*,#16244,.F.);
#22147=ORIENTED_EDGE('',*,*,#16245,.T.);
#22148=ORIENTED_EDGE('',*,*,#16246,.F.);
#22149=ORIENTED_EDGE('',*,*,#16027,.F.);
#22150=ORIENTED_EDGE('',*,*,#16247,.F.);
#22151=ORIENTED_EDGE('',*,*,#16242,.T.);
#22152=ORIENTED_EDGE('',*,*,#16241,.T.);
#22153=ORIENTED_EDGE('',*,*,#16248,.T.);
#22154=ORIENTED_EDGE('',*,*,#16025,.T.);
#22155=ORIENTED_EDGE('',*,*,#16249,.T.);
#22156=ORIENTED_EDGE('',*,*,#16243,.T.);
#22157=ORIENTED_EDGE('',*,*,#16247,.T.);
#22158=ORIENTED_EDGE('',*,*,#16026,.T.);
#22159=ORIENTED_EDGE('',*,*,#16248,.F.);
#22160=ORIENTED_EDGE('',*,*,#16024,.T.);
#22161=ORIENTED_EDGE('',*,*,#16250,.T.);
#22162=ORIENTED_EDGE('',*,*,#16238,.T.);
#22163=ORIENTED_EDGE('',*,*,#16249,.F.);
#22164=ORIENTED_EDGE('',*,*,#16251,.T.);
#22165=ORIENTED_EDGE('',*,*,#16252,.T.);
#22166=ORIENTED_EDGE('',*,*,#16030,.T.);
#22167=ORIENTED_EDGE('',*,*,#16253,.T.);
#22168=ORIENTED_EDGE('',*,*,#16029,.T.);
#22169=ORIENTED_EDGE('',*,*,#16254,.T.);
#22170=ORIENTED_EDGE('',*,*,#16255,.T.);
#22171=ORIENTED_EDGE('',*,*,#16253,.F.);
#22172=ORIENTED_EDGE('',*,*,#16028,.T.);
#22173=ORIENTED_EDGE('',*,*,#16246,.T.);
#22174=ORIENTED_EDGE('',*,*,#16256,.T.);
#22175=ORIENTED_EDGE('',*,*,#16254,.F.);
#22176=ORIENTED_EDGE('',*,*,#16251,.F.);
#22177=ORIENTED_EDGE('',*,*,#16257,.T.);
#22178=ORIENTED_EDGE('',*,*,#16258,.F.);
#22179=ORIENTED_EDGE('',*,*,#16259,.F.);
#22180=ORIENTED_EDGE('',*,*,#16255,.F.);
#22181=ORIENTED_EDGE('',*,*,#16260,.T.);
#22182=ORIENTED_EDGE('',*,*,#16261,.F.);
#22183=ORIENTED_EDGE('',*,*,#16257,.F.);
#22184=ORIENTED_EDGE('',*,*,#16256,.F.);
#22185=ORIENTED_EDGE('',*,*,#16245,.F.);
#22186=ORIENTED_EDGE('',*,*,#16262,.F.);
#22187=ORIENTED_EDGE('',*,*,#16260,.F.);
#22188=ORIENTED_EDGE('',*,*,#15699,.T.);
#22189=ORIENTED_EDGE('',*,*,#16263,.T.);
#22190=ORIENTED_EDGE('',*,*,#16258,.T.);
#22191=ORIENTED_EDGE('',*,*,#16264,.T.);
#22192=ORIENTED_EDGE('',*,*,#16261,.T.);
#22193=ORIENTED_EDGE('',*,*,#16265,.T.);
#22194=ORIENTED_EDGE('',*,*,#15700,.T.);
#22195=ORIENTED_EDGE('',*,*,#16264,.F.);
#22196=ORIENTED_EDGE('',*,*,#16262,.T.);
#22197=ORIENTED_EDGE('',*,*,#16244,.T.);
#22198=ORIENTED_EDGE('',*,*,#15701,.T.);
#22199=ORIENTED_EDGE('',*,*,#16265,.F.);
#22200=ORIENTED_EDGE('',*,*,#15454,.F.);
#22201=ORIENTED_EDGE('',*,*,#15926,.F.);
#22202=ORIENTED_EDGE('',*,*,#15928,.F.);
#22203=ORIENTED_EDGE('',*,*,#15929,.F.);
#22204=ORIENTED_EDGE('',*,*,#16224,.F.);
#22205=ORIENTED_EDGE('',*,*,#15352,.F.);
#22206=ORIENTED_EDGE('',*,*,#16266,.T.);
#22207=ORIENTED_EDGE('',*,*,#16228,.F.);
#22208=ORIENTED_EDGE('',*,*,#15351,.F.);
#22209=ORIENTED_EDGE('',*,*,#16227,.F.);
#22210=ORIENTED_EDGE('',*,*,#16229,.F.);
#22211=ORIENTED_EDGE('',*,*,#16266,.F.);
#22212=ORIENTED_EDGE('',*,*,#15460,.F.);
#22213=ORIENTED_EDGE('',*,*,#15916,.F.);
#22214=ORIENTED_EDGE('',*,*,#15918,.F.);
#22215=ORIENTED_EDGE('',*,*,#15919,.F.);
#22216=ORIENTED_EDGE('',*,*,#16217,.F.);
#22217=ORIENTED_EDGE('',*,*,#16267,.T.);
#22218=ORIENTED_EDGE('',*,*,#16268,.T.);
#22219=ORIENTED_EDGE('',*,*,#16269,.F.);
#22220=ORIENTED_EDGE('',*,*,#16219,.F.);
#22221=ORIENTED_EDGE('',*,*,#15346,.F.);
#22222=ORIENTED_EDGE('',*,*,#16270,.T.);
#22223=ORIENTED_EDGE('',*,*,#16267,.F.);
#22224=ORIENTED_EDGE('',*,*,#16220,.F.);
#22225=ORIENTED_EDGE('',*,*,#16269,.T.);
#22226=ORIENTED_EDGE('',*,*,#16271,.T.);
#22227=ORIENTED_EDGE('',*,*,#15344,.F.);
#22228=ORIENTED_EDGE('',*,*,#15345,.F.);
#22229=ORIENTED_EDGE('',*,*,#16271,.F.);
#22230=ORIENTED_EDGE('',*,*,#16268,.F.);
#22231=ORIENTED_EDGE('',*,*,#16270,.F.);
#22232=ORIENTED_EDGE('',*,*,#15466,.F.);
#22233=ORIENTED_EDGE('',*,*,#15906,.F.);
#22234=ORIENTED_EDGE('',*,*,#15908,.F.);
#22235=ORIENTED_EDGE('',*,*,#15909,.F.);
#22236=ORIENTED_EDGE('',*,*,#16213,.F.);
#22237=ORIENTED_EDGE('',*,*,#16272,.T.);
#22238=ORIENTED_EDGE('',*,*,#16273,.T.);
#22239=ORIENTED_EDGE('',*,*,#16274,.F.);
#22240=ORIENTED_EDGE('',*,*,#16215,.F.);
#22241=ORIENTED_EDGE('',*,*,#15340,.F.);
#22242=ORIENTED_EDGE('',*,*,#16275,.T.);
#22243=ORIENTED_EDGE('',*,*,#16272,.F.);
#22244=ORIENTED_EDGE('',*,*,#16212,.F.);
#22245=ORIENTED_EDGE('',*,*,#16274,.T.);
#22246=ORIENTED_EDGE('',*,*,#16276,.T.);
#22247=ORIENTED_EDGE('',*,*,#15338,.F.);
#22248=ORIENTED_EDGE('',*,*,#15339,.F.);
#22249=ORIENTED_EDGE('',*,*,#16276,.F.);
#22250=ORIENTED_EDGE('',*,*,#16273,.F.);
#22251=ORIENTED_EDGE('',*,*,#16275,.F.);
#22252=ORIENTED_EDGE('',*,*,#15472,.F.);
#22253=ORIENTED_EDGE('',*,*,#15896,.F.);
#22254=ORIENTED_EDGE('',*,*,#15898,.F.);
#22255=ORIENTED_EDGE('',*,*,#15899,.F.);
#22256=ORIENTED_EDGE('',*,*,#16205,.F.);
#22257=ORIENTED_EDGE('',*,*,#15334,.F.);
#22258=ORIENTED_EDGE('',*,*,#16277,.T.);
#22259=ORIENTED_EDGE('',*,*,#16209,.F.);
#22260=ORIENTED_EDGE('',*,*,#15333,.F.);
#22261=ORIENTED_EDGE('',*,*,#16208,.F.);
#22262=ORIENTED_EDGE('',*,*,#16210,.F.);
#22263=ORIENTED_EDGE('',*,*,#16277,.F.);
#22264=ORIENTED_EDGE('',*,*,#15478,.F.);
#22265=ORIENTED_EDGE('',*,*,#15886,.F.);
#22266=ORIENTED_EDGE('',*,*,#15888,.F.);
#22267=ORIENTED_EDGE('',*,*,#15889,.F.);
#22268=ORIENTED_EDGE('',*,*,#16198,.F.);
#22269=ORIENTED_EDGE('',*,*,#16278,.T.);
#22270=ORIENTED_EDGE('',*,*,#16279,.T.);
#22271=ORIENTED_EDGE('',*,*,#16280,.F.);
#22272=ORIENTED_EDGE('',*,*,#16200,.F.);
#22273=ORIENTED_EDGE('',*,*,#15328,.F.);
#22274=ORIENTED_EDGE('',*,*,#16281,.T.);
#22275=ORIENTED_EDGE('',*,*,#16278,.F.);
#22276=ORIENTED_EDGE('',*,*,#16201,.F.);
#22277=ORIENTED_EDGE('',*,*,#16280,.T.);
#22278=ORIENTED_EDGE('',*,*,#16282,.T.);
#22279=ORIENTED_EDGE('',*,*,#15326,.F.);
#22280=ORIENTED_EDGE('',*,*,#15327,.F.);
#22281=ORIENTED_EDGE('',*,*,#16282,.F.);
#22282=ORIENTED_EDGE('',*,*,#16279,.F.);
#22283=ORIENTED_EDGE('',*,*,#16281,.F.);
#22284=ORIENTED_EDGE('',*,*,#15484,.F.);
#22285=ORIENTED_EDGE('',*,*,#15876,.F.);
#22286=ORIENTED_EDGE('',*,*,#15878,.F.);
#22287=ORIENTED_EDGE('',*,*,#15879,.F.);
#22288=ORIENTED_EDGE('',*,*,#16191,.F.);
#22289=ORIENTED_EDGE('',*,*,#15322,.F.);
#22290=ORIENTED_EDGE('',*,*,#16283,.T.);
#22291=ORIENTED_EDGE('',*,*,#16195,.F.);
#22292=ORIENTED_EDGE('',*,*,#15321,.F.);
#22293=ORIENTED_EDGE('',*,*,#16194,.F.);
#22294=ORIENTED_EDGE('',*,*,#16196,.F.);
#22295=ORIENTED_EDGE('',*,*,#16283,.F.);
#22296=ORIENTED_EDGE('',*,*,#15490,.F.);
#22297=ORIENTED_EDGE('',*,*,#15866,.F.);
#22298=ORIENTED_EDGE('',*,*,#15868,.F.);
#22299=ORIENTED_EDGE('',*,*,#15869,.F.);
#22300=ORIENTED_EDGE('',*,*,#16184,.F.);
#22301=ORIENTED_EDGE('',*,*,#16284,.T.);
#22302=ORIENTED_EDGE('',*,*,#16285,.T.);
#22303=ORIENTED_EDGE('',*,*,#16286,.F.);
#22304=ORIENTED_EDGE('',*,*,#16186,.F.);
#22305=ORIENTED_EDGE('',*,*,#15316,.F.);
#22306=ORIENTED_EDGE('',*,*,#16287,.T.);
#22307=ORIENTED_EDGE('',*,*,#16284,.F.);
#22308=ORIENTED_EDGE('',*,*,#16187,.F.);
#22309=ORIENTED_EDGE('',*,*,#16286,.T.);
#22310=ORIENTED_EDGE('',*,*,#16288,.T.);
#22311=ORIENTED_EDGE('',*,*,#15314,.F.);
#22312=ORIENTED_EDGE('',*,*,#15315,.F.);
#22313=ORIENTED_EDGE('',*,*,#16288,.F.);
#22314=ORIENTED_EDGE('',*,*,#16285,.F.);
#22315=ORIENTED_EDGE('',*,*,#16287,.F.);
#22316=ORIENTED_EDGE('',*,*,#15496,.F.);
#22317=ORIENTED_EDGE('',*,*,#15856,.F.);
#22318=ORIENTED_EDGE('',*,*,#15858,.F.);
#22319=ORIENTED_EDGE('',*,*,#15859,.F.);
#22320=ORIENTED_EDGE('',*,*,#16177,.F.);
#22321=ORIENTED_EDGE('',*,*,#15310,.F.);
#22322=ORIENTED_EDGE('',*,*,#16289,.T.);
#22323=ORIENTED_EDGE('',*,*,#16181,.F.);
#22324=ORIENTED_EDGE('',*,*,#15309,.F.);
#22325=ORIENTED_EDGE('',*,*,#16180,.F.);
#22326=ORIENTED_EDGE('',*,*,#16182,.F.);
#22327=ORIENTED_EDGE('',*,*,#16289,.F.);
#22328=ORIENTED_EDGE('',*,*,#15502,.F.);
#22329=ORIENTED_EDGE('',*,*,#15846,.F.);
#22330=ORIENTED_EDGE('',*,*,#15848,.F.);
#22331=ORIENTED_EDGE('',*,*,#15849,.F.);
#22332=ORIENTED_EDGE('',*,*,#16170,.F.);
#22333=ORIENTED_EDGE('',*,*,#16290,.T.);
#22334=ORIENTED_EDGE('',*,*,#16291,.T.);
#22335=ORIENTED_EDGE('',*,*,#16292,.F.);
#22336=ORIENTED_EDGE('',*,*,#16172,.F.);
#22337=ORIENTED_EDGE('',*,*,#15304,.F.);
#22338=ORIENTED_EDGE('',*,*,#16293,.T.);
#22339=ORIENTED_EDGE('',*,*,#16290,.F.);
#22340=ORIENTED_EDGE('',*,*,#16173,.F.);
#22341=ORIENTED_EDGE('',*,*,#16292,.T.);
#22342=ORIENTED_EDGE('',*,*,#16294,.T.);
#22343=ORIENTED_EDGE('',*,*,#15302,.F.);
#22344=ORIENTED_EDGE('',*,*,#15303,.F.);
#22345=ORIENTED_EDGE('',*,*,#16294,.F.);
#22346=ORIENTED_EDGE('',*,*,#16291,.F.);
#22347=ORIENTED_EDGE('',*,*,#16293,.F.);
#22348=ORIENTED_EDGE('',*,*,#15508,.F.);
#22349=ORIENTED_EDGE('',*,*,#15836,.F.);
#22350=ORIENTED_EDGE('',*,*,#15838,.F.);
#22351=ORIENTED_EDGE('',*,*,#15839,.F.);
#22352=ORIENTED_EDGE('',*,*,#16165,.F.);
#22353=ORIENTED_EDGE('',*,*,#16295,.T.);
#22354=ORIENTED_EDGE('',*,*,#16296,.T.);
#22355=ORIENTED_EDGE('',*,*,#16297,.F.);
#22356=ORIENTED_EDGE('',*,*,#16168,.F.);
#22357=ORIENTED_EDGE('',*,*,#15298,.F.);
#22358=ORIENTED_EDGE('',*,*,#16298,.T.);
#22359=ORIENTED_EDGE('',*,*,#16295,.F.);
#22360=ORIENTED_EDGE('',*,*,#16167,.F.);
#22361=ORIENTED_EDGE('',*,*,#16297,.T.);
#22362=ORIENTED_EDGE('',*,*,#16299,.T.);
#22363=ORIENTED_EDGE('',*,*,#15296,.F.);
#22364=ORIENTED_EDGE('',*,*,#15297,.F.);
#22365=ORIENTED_EDGE('',*,*,#16299,.F.);
#22366=ORIENTED_EDGE('',*,*,#16296,.F.);
#22367=ORIENTED_EDGE('',*,*,#16298,.F.);
#22368=ORIENTED_EDGE('',*,*,#15514,.F.);
#22369=ORIENTED_EDGE('',*,*,#15826,.F.);
#22370=ORIENTED_EDGE('',*,*,#15828,.F.);
#22371=ORIENTED_EDGE('',*,*,#15829,.F.);
#22372=ORIENTED_EDGE('',*,*,#16158,.F.);
#22373=ORIENTED_EDGE('',*,*,#15292,.F.);
#22374=ORIENTED_EDGE('',*,*,#16300,.T.);
#22375=ORIENTED_EDGE('',*,*,#16162,.F.);
#22376=ORIENTED_EDGE('',*,*,#15291,.F.);
#22377=ORIENTED_EDGE('',*,*,#16161,.F.);
#22378=ORIENTED_EDGE('',*,*,#16163,.F.);
#22379=ORIENTED_EDGE('',*,*,#16300,.F.);
#22380=ORIENTED_EDGE('',*,*,#15520,.F.);
#22381=ORIENTED_EDGE('',*,*,#15816,.F.);
#22382=ORIENTED_EDGE('',*,*,#15818,.F.);
#22383=ORIENTED_EDGE('',*,*,#15819,.F.);
#22384=ORIENTED_EDGE('',*,*,#16151,.F.);
#22385=ORIENTED_EDGE('',*,*,#16301,.T.);
#22386=ORIENTED_EDGE('',*,*,#16302,.T.);
#22387=ORIENTED_EDGE('',*,*,#16303,.F.);
#22388=ORIENTED_EDGE('',*,*,#16153,.F.);
#22389=ORIENTED_EDGE('',*,*,#15286,.F.);
#22390=ORIENTED_EDGE('',*,*,#16304,.T.);
#22391=ORIENTED_EDGE('',*,*,#16301,.F.);
#22392=ORIENTED_EDGE('',*,*,#16154,.F.);
#22393=ORIENTED_EDGE('',*,*,#16303,.T.);
#22394=ORIENTED_EDGE('',*,*,#16305,.T.);
#22395=ORIENTED_EDGE('',*,*,#15284,.F.);
#22396=ORIENTED_EDGE('',*,*,#15285,.F.);
#22397=ORIENTED_EDGE('',*,*,#16305,.F.);
#22398=ORIENTED_EDGE('',*,*,#16302,.F.);
#22399=ORIENTED_EDGE('',*,*,#16304,.F.);
#22400=ORIENTED_EDGE('',*,*,#15526,.F.);
#22401=ORIENTED_EDGE('',*,*,#15808,.F.);
#22402=ORIENTED_EDGE('',*,*,#15809,.F.);
#22403=ORIENTED_EDGE('',*,*,#15802,.F.);
#22404=ORIENTED_EDGE('',*,*,#16144,.F.);
#22405=ORIENTED_EDGE('',*,*,#15280,.F.);
#22406=ORIENTED_EDGE('',*,*,#16306,.T.);
#22407=ORIENTED_EDGE('',*,*,#16148,.F.);
#22408=ORIENTED_EDGE('',*,*,#15279,.F.);
#22409=ORIENTED_EDGE('',*,*,#16147,.F.);
#22410=ORIENTED_EDGE('',*,*,#16149,.F.);
#22411=ORIENTED_EDGE('',*,*,#16306,.F.);
#22412=ORIENTED_EDGE('',*,*,#15532,.F.);
#22413=ORIENTED_EDGE('',*,*,#15796,.F.);
#22414=ORIENTED_EDGE('',*,*,#15798,.F.);
#22415=ORIENTED_EDGE('',*,*,#15799,.F.);
#22416=ORIENTED_EDGE('',*,*,#16137,.F.);
#22417=ORIENTED_EDGE('',*,*,#16307,.T.);
#22418=ORIENTED_EDGE('',*,*,#16308,.T.);
#22419=ORIENTED_EDGE('',*,*,#16309,.F.);
#22420=ORIENTED_EDGE('',*,*,#16139,.F.);
#22421=ORIENTED_EDGE('',*,*,#15274,.F.);
#22422=ORIENTED_EDGE('',*,*,#16310,.T.);
#22423=ORIENTED_EDGE('',*,*,#16307,.F.);
#22424=ORIENTED_EDGE('',*,*,#16140,.F.);
#22425=ORIENTED_EDGE('',*,*,#16309,.T.);
#22426=ORIENTED_EDGE('',*,*,#16311,.T.);
#22427=ORIENTED_EDGE('',*,*,#15272,.F.);
#22428=ORIENTED_EDGE('',*,*,#15273,.F.);
#22429=ORIENTED_EDGE('',*,*,#16311,.F.);
#22430=ORIENTED_EDGE('',*,*,#16308,.F.);
#22431=ORIENTED_EDGE('',*,*,#16310,.F.);
#22432=ORIENTED_EDGE('',*,*,#15538,.F.);
#22433=ORIENTED_EDGE('',*,*,#15786,.F.);
#22434=ORIENTED_EDGE('',*,*,#15788,.F.);
#22435=ORIENTED_EDGE('',*,*,#15789,.F.);
#22436=ORIENTED_EDGE('',*,*,#16130,.F.);
#22437=ORIENTED_EDGE('',*,*,#15268,.F.);
#22438=ORIENTED_EDGE('',*,*,#16312,.T.);
#22439=ORIENTED_EDGE('',*,*,#16134,.F.);
#22440=ORIENTED_EDGE('',*,*,#15267,.F.);
#22441=ORIENTED_EDGE('',*,*,#16133,.F.);
#22442=ORIENTED_EDGE('',*,*,#16135,.F.);
#22443=ORIENTED_EDGE('',*,*,#16312,.F.);
#22444=ORIENTED_EDGE('',*,*,#15544,.F.);
#22445=ORIENTED_EDGE('',*,*,#15776,.F.);
#22446=ORIENTED_EDGE('',*,*,#15778,.F.);
#22447=ORIENTED_EDGE('',*,*,#15779,.F.);
#22448=ORIENTED_EDGE('',*,*,#16123,.F.);
#22449=ORIENTED_EDGE('',*,*,#16313,.T.);
#22450=ORIENTED_EDGE('',*,*,#16314,.T.);
#22451=ORIENTED_EDGE('',*,*,#16315,.F.);
#22452=ORIENTED_EDGE('',*,*,#16125,.F.);
#22453=ORIENTED_EDGE('',*,*,#15262,.F.);
#22454=ORIENTED_EDGE('',*,*,#16316,.T.);
#22455=ORIENTED_EDGE('',*,*,#16313,.F.);
#22456=ORIENTED_EDGE('',*,*,#16126,.F.);
#22457=ORIENTED_EDGE('',*,*,#16315,.T.);
#22458=ORIENTED_EDGE('',*,*,#16317,.T.);
#22459=ORIENTED_EDGE('',*,*,#15260,.F.);
#22460=ORIENTED_EDGE('',*,*,#15261,.F.);
#22461=ORIENTED_EDGE('',*,*,#16317,.F.);
#22462=ORIENTED_EDGE('',*,*,#16314,.F.);
#22463=ORIENTED_EDGE('',*,*,#16316,.F.);
#22464=ORIENTED_EDGE('',*,*,#15550,.F.);
#22465=ORIENTED_EDGE('',*,*,#15766,.F.);
#22466=ORIENTED_EDGE('',*,*,#15768,.F.);
#22467=ORIENTED_EDGE('',*,*,#15769,.F.);
#22468=ORIENTED_EDGE('',*,*,#16116,.F.);
#22469=ORIENTED_EDGE('',*,*,#15256,.F.);
#22470=ORIENTED_EDGE('',*,*,#16318,.T.);
#22471=ORIENTED_EDGE('',*,*,#16120,.F.);
#22472=ORIENTED_EDGE('',*,*,#15255,.F.);
#22473=ORIENTED_EDGE('',*,*,#16119,.F.);
#22474=ORIENTED_EDGE('',*,*,#16121,.F.);
#22475=ORIENTED_EDGE('',*,*,#16318,.F.);
#22476=ORIENTED_EDGE('',*,*,#15556,.F.);
#22477=ORIENTED_EDGE('',*,*,#15756,.F.);
#22478=ORIENTED_EDGE('',*,*,#15758,.F.);
#22479=ORIENTED_EDGE('',*,*,#15759,.F.);
#22480=ORIENTED_EDGE('',*,*,#16109,.F.);
#22481=ORIENTED_EDGE('',*,*,#16319,.T.);
#22482=ORIENTED_EDGE('',*,*,#16320,.T.);
#22483=ORIENTED_EDGE('',*,*,#16321,.F.);
#22484=ORIENTED_EDGE('',*,*,#16111,.F.);
#22485=ORIENTED_EDGE('',*,*,#15250,.F.);
#22486=ORIENTED_EDGE('',*,*,#16322,.T.);
#22487=ORIENTED_EDGE('',*,*,#16319,.F.);
#22488=ORIENTED_EDGE('',*,*,#16112,.F.);
#22489=ORIENTED_EDGE('',*,*,#16321,.T.);
#22490=ORIENTED_EDGE('',*,*,#16323,.T.);
#22491=ORIENTED_EDGE('',*,*,#15248,.F.);
#22492=ORIENTED_EDGE('',*,*,#15249,.F.);
#22493=ORIENTED_EDGE('',*,*,#16323,.F.);
#22494=ORIENTED_EDGE('',*,*,#16320,.F.);
#22495=ORIENTED_EDGE('',*,*,#16322,.F.);
#22496=ORIENTED_EDGE('',*,*,#15562,.F.);
#22497=ORIENTED_EDGE('',*,*,#15746,.F.);
#22498=ORIENTED_EDGE('',*,*,#15748,.F.);
#22499=ORIENTED_EDGE('',*,*,#15749,.F.);
#22500=ORIENTED_EDGE('',*,*,#16102,.F.);
#22501=ORIENTED_EDGE('',*,*,#15244,.F.);
#22502=ORIENTED_EDGE('',*,*,#16324,.T.);
#22503=ORIENTED_EDGE('',*,*,#16106,.F.);
#22504=ORIENTED_EDGE('',*,*,#15243,.F.);
#22505=ORIENTED_EDGE('',*,*,#16105,.F.);
#22506=ORIENTED_EDGE('',*,*,#16107,.F.);
#22507=ORIENTED_EDGE('',*,*,#16324,.F.);
#22508=ORIENTED_EDGE('',*,*,#15739,.F.);
#22509=ORIENTED_EDGE('',*,*,#15738,.T.);
#22510=ORIENTED_EDGE('',*,*,#16325,.T.);
#22511=ORIENTED_EDGE('',*,*,#15567,.F.);
#22512=ORIENTED_EDGE('',*,*,#15568,.F.);
#22513=ORIENTED_EDGE('',*,*,#16325,.F.);
#22514=ORIENTED_EDGE('',*,*,#15737,.F.);
#22515=ORIENTED_EDGE('',*,*,#15206,.F.);
#22516=ORIENTED_EDGE('',*,*,#16095,.F.);
#22517=ORIENTED_EDGE('',*,*,#16326,.T.);
#22518=ORIENTED_EDGE('',*,*,#16327,.T.);
#22519=ORIENTED_EDGE('',*,*,#16328,.F.);
#22520=ORIENTED_EDGE('',*,*,#16097,.F.);
#22521=ORIENTED_EDGE('',*,*,#15238,.F.);
#22522=ORIENTED_EDGE('',*,*,#16329,.T.);
#22523=ORIENTED_EDGE('',*,*,#16326,.F.);
#22524=ORIENTED_EDGE('',*,*,#16098,.F.);
#22525=ORIENTED_EDGE('',*,*,#16328,.T.);
#22526=ORIENTED_EDGE('',*,*,#16330,.T.);
#22527=ORIENTED_EDGE('',*,*,#15236,.F.);
#22528=ORIENTED_EDGE('',*,*,#15237,.F.);
#22529=ORIENTED_EDGE('',*,*,#16330,.F.);
#22530=ORIENTED_EDGE('',*,*,#16327,.F.);
#22531=ORIENTED_EDGE('',*,*,#16329,.F.);
#22532=ORIENTED_EDGE('',*,*,#15211,.F.);
#22533=ORIENTED_EDGE('',*,*,#15578,.F.);
#22534=ORIENTED_EDGE('',*,*,#15580,.F.);
#22535=ORIENTED_EDGE('',*,*,#15581,.F.);
#22536=ORIENTED_EDGE('',*,*,#16088,.F.);
#22537=ORIENTED_EDGE('',*,*,#15232,.F.);
#22538=ORIENTED_EDGE('',*,*,#16331,.T.);
#22539=ORIENTED_EDGE('',*,*,#16092,.F.);
#22540=ORIENTED_EDGE('',*,*,#15231,.F.);
#22541=ORIENTED_EDGE('',*,*,#16091,.F.);
#22542=ORIENTED_EDGE('',*,*,#16093,.F.);
#22543=ORIENTED_EDGE('',*,*,#16331,.F.);
#22544=ORIENTED_EDGE('',*,*,#15217,.F.);
#22545=ORIENTED_EDGE('',*,*,#15591,.F.);
#22546=ORIENTED_EDGE('',*,*,#15593,.F.);
#22547=ORIENTED_EDGE('',*,*,#15594,.F.);
#22548=ORIENTED_EDGE('',*,*,#16081,.F.);
#22549=ORIENTED_EDGE('',*,*,#16332,.T.);
#22550=ORIENTED_EDGE('',*,*,#16333,.T.);
#22551=ORIENTED_EDGE('',*,*,#16334,.F.);
#22552=ORIENTED_EDGE('',*,*,#16083,.F.);
#22553=ORIENTED_EDGE('',*,*,#15226,.F.);
#22554=ORIENTED_EDGE('',*,*,#16335,.T.);
#22555=ORIENTED_EDGE('',*,*,#16332,.F.);
#22556=ORIENTED_EDGE('',*,*,#16084,.F.);
#22557=ORIENTED_EDGE('',*,*,#16334,.T.);
#22558=ORIENTED_EDGE('',*,*,#16336,.T.);
#22559=ORIENTED_EDGE('',*,*,#15224,.F.);
#22560=ORIENTED_EDGE('',*,*,#15225,.F.);
#22561=ORIENTED_EDGE('',*,*,#16336,.F.);
#22562=ORIENTED_EDGE('',*,*,#16333,.F.);
#22563=ORIENTED_EDGE('',*,*,#16335,.F.);
#22564=ORIENTED_EDGE('',*,*,#15406,.F.);
#22565=ORIENTED_EDGE('',*,*,#15604,.F.);
#22566=ORIENTED_EDGE('',*,*,#15606,.F.);
#22567=ORIENTED_EDGE('',*,*,#15607,.F.);
#22568=ORIENTED_EDGE('',*,*,#16077,.F.);
#22569=ORIENTED_EDGE('',*,*,#16337,.T.);
#22570=ORIENTED_EDGE('',*,*,#16338,.T.);
#22571=ORIENTED_EDGE('',*,*,#16339,.F.);
#22572=ORIENTED_EDGE('',*,*,#16079,.F.);
#22573=ORIENTED_EDGE('',*,*,#15400,.F.);
#22574=ORIENTED_EDGE('',*,*,#16340,.T.);
#22575=ORIENTED_EDGE('',*,*,#16337,.F.);
#22576=ORIENTED_EDGE('',*,*,#16076,.F.);
#22577=ORIENTED_EDGE('',*,*,#16339,.T.);
#22578=ORIENTED_EDGE('',*,*,#16341,.T.);
#22579=ORIENTED_EDGE('',*,*,#15398,.F.);
#22580=ORIENTED_EDGE('',*,*,#15399,.F.);
#22581=ORIENTED_EDGE('',*,*,#16341,.F.);
#22582=ORIENTED_EDGE('',*,*,#16338,.F.);
#22583=ORIENTED_EDGE('',*,*,#16340,.F.);
#22584=ORIENTED_EDGE('',*,*,#15412,.F.);
#22585=ORIENTED_EDGE('',*,*,#15615,.F.);
#22586=ORIENTED_EDGE('',*,*,#15617,.F.);
#22587=ORIENTED_EDGE('',*,*,#16342,.F.);
#22588=ORIENTED_EDGE('',*,*,#15618,.F.);
#22589=ORIENTED_EDGE('',*,*,#15413,.F.);
#22590=ORIENTED_EDGE('',*,*,#16342,.T.);
#22591=ORIENTED_EDGE('',*,*,#15616,.F.);
#22592=ORIENTED_EDGE('',*,*,#16069,.F.);
#22593=ORIENTED_EDGE('',*,*,#15394,.F.);
#22594=ORIENTED_EDGE('',*,*,#16343,.T.);
#22595=ORIENTED_EDGE('',*,*,#16073,.F.);
#22596=ORIENTED_EDGE('',*,*,#15393,.F.);
#22597=ORIENTED_EDGE('',*,*,#16072,.F.);
#22598=ORIENTED_EDGE('',*,*,#16074,.F.);
#22599=ORIENTED_EDGE('',*,*,#16343,.F.);
#22600=ORIENTED_EDGE('',*,*,#15705,.F.);
#22601=ORIENTED_EDGE('',*,*,#16344,.T.);
#22602=ORIENTED_EDGE('',*,*,#16345,.T.);
#22603=ORIENTED_EDGE('',*,*,#15417,.F.);
#22604=ORIENTED_EDGE('',*,*,#15418,.F.);
#22605=ORIENTED_EDGE('',*,*,#16345,.F.);
#22606=ORIENTED_EDGE('',*,*,#16346,.F.);
#22607=ORIENTED_EDGE('',*,*,#16347,.F.);
#22608=ORIENTED_EDGE('',*,*,#15708,.F.);
#22609=ORIENTED_EDGE('',*,*,#16348,.T.);
#22610=ORIENTED_EDGE('',*,*,#16346,.T.);
#22611=ORIENTED_EDGE('',*,*,#16344,.F.);
#22612=ORIENTED_EDGE('',*,*,#15709,.F.);
#22613=ORIENTED_EDGE('',*,*,#15419,.F.);
#22614=ORIENTED_EDGE('',*,*,#16347,.T.);
#22615=ORIENTED_EDGE('',*,*,#16348,.F.);
#22616=ORIENTED_EDGE('',*,*,#16062,.F.);
#22617=ORIENTED_EDGE('',*,*,#16349,.T.);
#22618=ORIENTED_EDGE('',*,*,#16350,.T.);
#22619=ORIENTED_EDGE('',*,*,#16351,.F.);
#22620=ORIENTED_EDGE('',*,*,#16064,.F.);
#22621=ORIENTED_EDGE('',*,*,#15388,.F.);
#22622=ORIENTED_EDGE('',*,*,#16352,.T.);
#22623=ORIENTED_EDGE('',*,*,#16349,.F.);
#22624=ORIENTED_EDGE('',*,*,#16065,.F.);
#22625=ORIENTED_EDGE('',*,*,#16351,.T.);
#22626=ORIENTED_EDGE('',*,*,#16353,.T.);
#22627=ORIENTED_EDGE('',*,*,#15386,.F.);
#22628=ORIENTED_EDGE('',*,*,#15387,.F.);
#22629=ORIENTED_EDGE('',*,*,#16353,.F.);
#22630=ORIENTED_EDGE('',*,*,#16350,.F.);
#22631=ORIENTED_EDGE('',*,*,#16352,.F.);
#22632=ORIENTED_EDGE('',*,*,#15710,.F.);
#22633=ORIENTED_EDGE('',*,*,#16354,.T.);
#22634=ORIENTED_EDGE('',*,*,#16355,.T.);
#22635=ORIENTED_EDGE('',*,*,#15423,.F.);
#22636=ORIENTED_EDGE('',*,*,#15424,.F.);
#22637=ORIENTED_EDGE('',*,*,#16355,.F.);
#22638=ORIENTED_EDGE('',*,*,#16356,.F.);
#22639=ORIENTED_EDGE('',*,*,#16357,.F.);
#22640=ORIENTED_EDGE('',*,*,#15713,.F.);
#22641=ORIENTED_EDGE('',*,*,#16358,.T.);
#22642=ORIENTED_EDGE('',*,*,#16356,.T.);
#22643=ORIENTED_EDGE('',*,*,#16354,.F.);
#22644=ORIENTED_EDGE('',*,*,#15714,.F.);
#22645=ORIENTED_EDGE('',*,*,#15425,.F.);
#22646=ORIENTED_EDGE('',*,*,#16357,.T.);
#22647=ORIENTED_EDGE('',*,*,#16358,.F.);
#22648=ORIENTED_EDGE('',*,*,#16055,.F.);
#22649=ORIENTED_EDGE('',*,*,#15382,.F.);
#22650=ORIENTED_EDGE('',*,*,#16359,.T.);
#22651=ORIENTED_EDGE('',*,*,#16059,.F.);
#22652=ORIENTED_EDGE('',*,*,#15381,.F.);
#22653=ORIENTED_EDGE('',*,*,#16058,.F.);
#22654=ORIENTED_EDGE('',*,*,#16060,.F.);
#22655=ORIENTED_EDGE('',*,*,#16359,.F.);
#22656=ORIENTED_EDGE('',*,*,#15715,.F.);
#22657=ORIENTED_EDGE('',*,*,#16360,.T.);
#22658=ORIENTED_EDGE('',*,*,#16361,.T.);
#22659=ORIENTED_EDGE('',*,*,#15429,.F.);
#22660=ORIENTED_EDGE('',*,*,#15430,.F.);
#22661=ORIENTED_EDGE('',*,*,#16361,.F.);
#22662=ORIENTED_EDGE('',*,*,#16362,.F.);
#22663=ORIENTED_EDGE('',*,*,#16363,.F.);
#22664=ORIENTED_EDGE('',*,*,#15718,.F.);
#22665=ORIENTED_EDGE('',*,*,#16364,.T.);
#22666=ORIENTED_EDGE('',*,*,#16362,.T.);
#22667=ORIENTED_EDGE('',*,*,#16360,.F.);
#22668=ORIENTED_EDGE('',*,*,#15719,.F.);
#22669=ORIENTED_EDGE('',*,*,#15431,.F.);
#22670=ORIENTED_EDGE('',*,*,#16363,.T.);
#22671=ORIENTED_EDGE('',*,*,#16364,.F.);
#22672=ORIENTED_EDGE('',*,*,#16048,.F.);
#22673=ORIENTED_EDGE('',*,*,#16365,.T.);
#22674=ORIENTED_EDGE('',*,*,#16366,.T.);
#22675=ORIENTED_EDGE('',*,*,#16367,.F.);
#22676=ORIENTED_EDGE('',*,*,#16050,.F.);
#22677=ORIENTED_EDGE('',*,*,#15376,.F.);
#22678=ORIENTED_EDGE('',*,*,#16368,.T.);
#22679=ORIENTED_EDGE('',*,*,#16365,.F.);
#22680=ORIENTED_EDGE('',*,*,#16051,.F.);
#22681=ORIENTED_EDGE('',*,*,#16367,.T.);
#22682=ORIENTED_EDGE('',*,*,#16369,.T.);
#22683=ORIENTED_EDGE('',*,*,#15374,.F.);
#22684=ORIENTED_EDGE('',*,*,#15375,.F.);
#22685=ORIENTED_EDGE('',*,*,#16369,.F.);
#22686=ORIENTED_EDGE('',*,*,#16366,.F.);
#22687=ORIENTED_EDGE('',*,*,#16368,.F.);
#22688=ORIENTED_EDGE('',*,*,#15720,.F.);
#22689=ORIENTED_EDGE('',*,*,#16370,.T.);
#22690=ORIENTED_EDGE('',*,*,#16371,.T.);
#22691=ORIENTED_EDGE('',*,*,#15435,.F.);
#22692=ORIENTED_EDGE('',*,*,#15436,.F.);
#22693=ORIENTED_EDGE('',*,*,#16371,.F.);
#22694=ORIENTED_EDGE('',*,*,#16372,.F.);
#22695=ORIENTED_EDGE('',*,*,#16373,.F.);
#22696=ORIENTED_EDGE('',*,*,#15723,.F.);
#22697=ORIENTED_EDGE('',*,*,#16374,.T.);
#22698=ORIENTED_EDGE('',*,*,#16372,.T.);
#22699=ORIENTED_EDGE('',*,*,#16370,.F.);
#22700=ORIENTED_EDGE('',*,*,#15724,.F.);
#22701=ORIENTED_EDGE('',*,*,#15437,.F.);
#22702=ORIENTED_EDGE('',*,*,#16373,.T.);
#22703=ORIENTED_EDGE('',*,*,#16374,.F.);
#22704=ORIENTED_EDGE('',*,*,#16041,.F.);
#22705=ORIENTED_EDGE('',*,*,#15370,.F.);
#22706=ORIENTED_EDGE('',*,*,#16375,.T.);
#22707=ORIENTED_EDGE('',*,*,#16045,.F.);
#22708=ORIENTED_EDGE('',*,*,#15369,.F.);
#22709=ORIENTED_EDGE('',*,*,#16044,.F.);
#22710=ORIENTED_EDGE('',*,*,#16046,.F.);
#22711=ORIENTED_EDGE('',*,*,#16375,.F.);
#22712=ORIENTED_EDGE('',*,*,#15725,.F.);
#22713=ORIENTED_EDGE('',*,*,#16376,.T.);
#22714=ORIENTED_EDGE('',*,*,#16377,.T.);
#22715=ORIENTED_EDGE('',*,*,#15441,.F.);
#22716=ORIENTED_EDGE('',*,*,#15442,.F.);
#22717=ORIENTED_EDGE('',*,*,#16377,.F.);
#22718=ORIENTED_EDGE('',*,*,#16378,.F.);
#22719=ORIENTED_EDGE('',*,*,#16379,.F.);
#22720=ORIENTED_EDGE('',*,*,#15728,.F.);
#22721=ORIENTED_EDGE('',*,*,#16380,.T.);
#22722=ORIENTED_EDGE('',*,*,#16378,.T.);
#22723=ORIENTED_EDGE('',*,*,#16376,.F.);
#22724=ORIENTED_EDGE('',*,*,#15729,.F.);
#22725=ORIENTED_EDGE('',*,*,#15443,.F.);
#22726=ORIENTED_EDGE('',*,*,#16379,.T.);
#22727=ORIENTED_EDGE('',*,*,#16380,.F.);
#22728=ORIENTED_EDGE('',*,*,#16034,.F.);
#22729=ORIENTED_EDGE('',*,*,#16381,.T.);
#22730=ORIENTED_EDGE('',*,*,#16382,.T.);
#22731=ORIENTED_EDGE('',*,*,#16383,.F.);
#22732=ORIENTED_EDGE('',*,*,#16036,.F.);
#22733=ORIENTED_EDGE('',*,*,#15364,.F.);
#22734=ORIENTED_EDGE('',*,*,#16384,.T.);
#22735=ORIENTED_EDGE('',*,*,#16381,.F.);
#22736=ORIENTED_EDGE('',*,*,#16037,.F.);
#22737=ORIENTED_EDGE('',*,*,#16383,.T.);
#22738=ORIENTED_EDGE('',*,*,#16385,.T.);
#22739=ORIENTED_EDGE('',*,*,#15362,.F.);
#22740=ORIENTED_EDGE('',*,*,#15363,.F.);
#22741=ORIENTED_EDGE('',*,*,#16385,.F.);
#22742=ORIENTED_EDGE('',*,*,#16382,.F.);
#22743=ORIENTED_EDGE('',*,*,#16384,.F.);
#22744=ORIENTED_EDGE('',*,*,#15730,.F.);
#22745=ORIENTED_EDGE('',*,*,#16386,.T.);
#22746=ORIENTED_EDGE('',*,*,#16387,.T.);
#22747=ORIENTED_EDGE('',*,*,#15447,.F.);
#22748=ORIENTED_EDGE('',*,*,#15448,.F.);
#22749=ORIENTED_EDGE('',*,*,#16387,.F.);
#22750=ORIENTED_EDGE('',*,*,#16388,.F.);
#22751=ORIENTED_EDGE('',*,*,#16389,.F.);
#22752=ORIENTED_EDGE('',*,*,#15733,.F.);
#22753=ORIENTED_EDGE('',*,*,#16390,.T.);
#22754=ORIENTED_EDGE('',*,*,#16388,.T.);
#22755=ORIENTED_EDGE('',*,*,#16386,.F.);
#22756=ORIENTED_EDGE('',*,*,#15734,.F.);
#22757=ORIENTED_EDGE('',*,*,#15449,.F.);
#22758=ORIENTED_EDGE('',*,*,#16389,.T.);
#22759=ORIENTED_EDGE('',*,*,#16390,.F.);
#22760=ORIENTED_EDGE('',*,*,#15357,.F.);
#22761=ORIENTED_EDGE('',*,*,#16391,.F.);
#22762=ORIENTED_EDGE('',*,*,#16392,.F.);
#22763=ORIENTED_EDGE('',*,*,#16393,.F.);
#22764=ORIENTED_EDGE('',*,*,#16032,.F.);
#22765=ORIENTED_EDGE('',*,*,#15358,.F.);
#22766=ORIENTED_EDGE('',*,*,#16393,.T.);
#22767=ORIENTED_EDGE('',*,*,#16394,.F.);
#22768=ORIENTED_EDGE('',*,*,#15932,.F.);
#22769=ORIENTED_EDGE('',*,*,#16394,.T.);
#22770=ORIENTED_EDGE('',*,*,#16392,.T.);
#22771=ORIENTED_EDGE('',*,*,#16395,.F.);
#22772=ORIENTED_EDGE('',*,*,#15934,.F.);
#22773=ORIENTED_EDGE('',*,*,#16395,.T.);
#22774=ORIENTED_EDGE('',*,*,#16391,.T.);
#22775=ORIENTED_EDGE('',*,*,#15356,.F.);
#22776=ORIENTED_EDGE('',*,*,#16236,.F.);
#22777=ORIENTED_EDGE('',*,*,#16239,.T.);
#22778=ORIENTED_EDGE('',*,*,#16250,.F.);
#22779=ORIENTED_EDGE('',*,*,#16031,.F.);
#22780=ORIENTED_EDGE('',*,*,#16252,.F.);
#22781=ORIENTED_EDGE('',*,*,#16259,.T.);
#22782=ORIENTED_EDGE('',*,*,#16263,.F.);
#22783=ORIENTED_EDGE('',*,*,#15698,.T.);
#22784=ORIENTED_EDGE('',*,*,#16396,.F.);
#22785=ORIENTED_EDGE('',*,*,#16397,.T.);
#22786=ORIENTED_EDGE('',*,*,#16398,.T.);
#22787=ORIENTED_EDGE('',*,*,#16399,.F.);
#22788=ORIENTED_EDGE('',*,*,#16400,.F.);
#22789=ORIENTED_EDGE('',*,*,#16399,.T.);
#22790=ORIENTED_EDGE('',*,*,#16401,.T.);
#22791=ORIENTED_EDGE('',*,*,#16402,.F.);
#22792=ORIENTED_EDGE('',*,*,#16403,.F.);
#22793=ORIENTED_EDGE('',*,*,#16404,.T.);
#22794=ORIENTED_EDGE('',*,*,#16405,.T.);
#22795=ORIENTED_EDGE('',*,*,#16397,.F.);
#22796=ORIENTED_EDGE('',*,*,#16406,.F.);
#22797=ORIENTED_EDGE('',*,*,#16402,.T.);
#22798=ORIENTED_EDGE('',*,*,#16407,.T.);
#22799=ORIENTED_EDGE('',*,*,#16404,.F.);
#22800=ORIENTED_EDGE('',*,*,#16398,.F.);
#22801=ORIENTED_EDGE('',*,*,#16405,.F.);
#22802=ORIENTED_EDGE('',*,*,#16407,.F.);
#22803=ORIENTED_EDGE('',*,*,#16401,.F.);
#22804=ORIENTED_EDGE('',*,*,#16408,.F.);
#22805=ORIENTED_EDGE('',*,*,#16409,.F.);
#22806=ORIENTED_EDGE('',*,*,#16410,.T.);
#22807=ORIENTED_EDGE('',*,*,#16411,.F.);
#22808=ORIENTED_EDGE('',*,*,#16412,.F.);
#22809=ORIENTED_EDGE('',*,*,#16410,.F.);
#22810=ORIENTED_EDGE('',*,*,#16413,.F.);
#22811=ORIENTED_EDGE('',*,*,#16414,.F.);
#22812=ORIENTED_EDGE('',*,*,#16415,.F.);
#22813=ORIENTED_EDGE('',*,*,#16416,.T.);
#22814=ORIENTED_EDGE('',*,*,#16414,.T.);
#22815=ORIENTED_EDGE('',*,*,#16416,.F.);
#22816=ORIENTED_EDGE('',*,*,#16417,.F.);
#22817=ORIENTED_EDGE('',*,*,#16418,.T.);
#22818=ORIENTED_EDGE('',*,*,#16413,.T.);
#22819=ORIENTED_EDGE('',*,*,#16419,.T.);
#22820=ORIENTED_EDGE('',*,*,#16415,.T.);
#22821=ORIENTED_EDGE('',*,*,#16419,.F.);
#22822=ORIENTED_EDGE('',*,*,#16409,.T.);
#22823=ORIENTED_EDGE('',*,*,#16408,.T.);
#22824=ORIENTED_EDGE('',*,*,#16418,.F.);
#22825=ORIENTED_EDGE('',*,*,#16411,.T.);
#22826=ORIENTED_EDGE('',*,*,#16412,.T.);
#22827=ORIENTED_EDGE('',*,*,#16420,.F.);
#22828=ORIENTED_EDGE('',*,*,#16421,.T.);
#22829=ORIENTED_EDGE('',*,*,#16417,.T.);
#22830=ORIENTED_EDGE('',*,*,#16421,.F.);
#22831=ORIENTED_EDGE('',*,*,#16422,.F.);
#22832=ORIENTED_EDGE('',*,*,#16423,.T.);
#22833=ORIENTED_EDGE('',*,*,#16420,.T.);
#22834=ORIENTED_EDGE('',*,*,#16423,.F.);
#22835=ORIENTED_EDGE('',*,*,#16424,.F.);
#22836=ORIENTED_EDGE('',*,*,#16422,.T.);
#22837=ORIENTED_EDGE('',*,*,#16425,.F.);
#22838=ORIENTED_EDGE('',*,*,#16426,.T.);
#22839=ORIENTED_EDGE('',*,*,#16424,.T.);
#22840=ORIENTED_EDGE('',*,*,#16426,.F.);
#22841=ORIENTED_EDGE('',*,*,#16425,.T.);
#22842=ORIENTED_EDGE('',*,*,#16427,.F.);
#22843=ORIENTED_EDGE('',*,*,#16428,.F.);
#22844=ORIENTED_EDGE('',*,*,#16429,.T.);
#22845=ORIENTED_EDGE('',*,*,#16427,.T.);
#22846=ORIENTED_EDGE('',*,*,#16429,.F.);
#22847=ORIENTED_EDGE('',*,*,#16428,.T.);
#22848=ORIENTED_EDGE('',*,*,#16430,.F.);
#22849=ORIENTED_EDGE('',*,*,#16431,.F.);
#22850=ORIENTED_EDGE('',*,*,#16432,.T.);
#22851=ORIENTED_EDGE('',*,*,#16430,.T.);
#22852=ORIENTED_EDGE('',*,*,#16432,.F.);
#22853=ORIENTED_EDGE('',*,*,#16433,.F.);
#22854=ORIENTED_EDGE('',*,*,#16431,.T.);
#22855=ORIENTED_EDGE('',*,*,#16434,.F.);
#22856=ORIENTED_EDGE('',*,*,#16435,.T.);
#22857=ORIENTED_EDGE('',*,*,#16433,.T.);
#22858=ORIENTED_EDGE('',*,*,#16435,.F.);
#22859=ORIENTED_EDGE('',*,*,#16434,.T.);
#22860=ORIENTED_EDGE('',*,*,#16436,.F.);
#22861=ORIENTED_EDGE('',*,*,#16437,.F.);
#22862=ORIENTED_EDGE('',*,*,#16438,.T.);
#22863=ORIENTED_EDGE('',*,*,#16436,.T.);
#22864=ORIENTED_EDGE('',*,*,#16438,.F.);
#22865=ORIENTED_EDGE('',*,*,#16406,.T.);
#22866=ORIENTED_EDGE('',*,*,#16403,.T.);
#22867=ORIENTED_EDGE('',*,*,#16396,.T.);
#22868=ORIENTED_EDGE('',*,*,#16400,.T.);
#22869=ORIENTED_EDGE('',*,*,#16439,.F.);
#22870=ORIENTED_EDGE('',*,*,#16440,.T.);
#22871=ORIENTED_EDGE('',*,*,#16437,.T.);
#22872=ORIENTED_EDGE('',*,*,#16440,.F.);
#22873=ORIENTED_EDGE('',*,*,#16439,.T.);
#22874=ORIENTED_EDGE('',*,*,#16441,.F.);
#22875=ORIENTED_EDGE('',*,*,#16442,.T.);
#22876=ORIENTED_EDGE('',*,*,#16443,.T.);
#22877=ORIENTED_EDGE('',*,*,#16442,.F.);
#22878=ORIENTED_EDGE('',*,*,#16444,.F.);
#22879=ORIENTED_EDGE('',*,*,#16441,.T.);
#22880=ORIENTED_EDGE('',*,*,#16444,.T.);
#22881=ORIENTED_EDGE('',*,*,#16445,.T.);
#22882=ORIENTED_EDGE('',*,*,#16446,.F.);
#22883=ORIENTED_EDGE('',*,*,#16445,.F.);
#22884=ORIENTED_EDGE('',*,*,#16447,.F.);
#22885=ORIENTED_EDGE('',*,*,#16446,.T.);
#22886=ORIENTED_EDGE('',*,*,#16448,.F.);
#22887=ORIENTED_EDGE('',*,*,#16449,.T.);
#22888=ORIENTED_EDGE('',*,*,#16447,.T.);
#22889=ORIENTED_EDGE('',*,*,#16449,.F.);
#22890=ORIENTED_EDGE('',*,*,#16450,.F.);
#22891=ORIENTED_EDGE('',*,*,#16451,.T.);
#22892=ORIENTED_EDGE('',*,*,#16448,.T.);
#22893=ORIENTED_EDGE('',*,*,#16451,.F.);
#22894=ORIENTED_EDGE('',*,*,#16452,.F.);
#22895=ORIENTED_EDGE('',*,*,#16453,.T.);
#22896=ORIENTED_EDGE('',*,*,#16450,.T.);
#22897=ORIENTED_EDGE('',*,*,#16453,.F.);
#22898=ORIENTED_EDGE('',*,*,#16452,.T.);
#22899=ORIENTED_EDGE('',*,*,#16454,.F.);
#22900=ORIENTED_EDGE('',*,*,#16454,.T.);
#22901=ORIENTED_EDGE('',*,*,#16455,.T.);
#22902=ORIENTED_EDGE('',*,*,#16456,.F.);
#22903=ORIENTED_EDGE('',*,*,#16455,.F.);
#22904=ORIENTED_EDGE('',*,*,#16456,.T.);
#22905=ORIENTED_EDGE('',*,*,#16457,.F.);
#22906=ORIENTED_EDGE('',*,*,#16458,.F.);
#22907=ORIENTED_EDGE('',*,*,#16459,.T.);
#22908=ORIENTED_EDGE('',*,*,#16457,.T.);
#22909=ORIENTED_EDGE('',*,*,#16459,.F.);
#22910=ORIENTED_EDGE('',*,*,#16458,.T.);
#22911=ORIENTED_EDGE('',*,*,#16460,.F.);
#22912=ORIENTED_EDGE('',*,*,#16460,.T.);
#22913=ORIENTED_EDGE('',*,*,#16461,.T.);
#22914=ORIENTED_EDGE('',*,*,#16462,.F.);
#22915=ORIENTED_EDGE('',*,*,#16461,.F.);
#22916=ORIENTED_EDGE('',*,*,#16462,.T.);
#22917=ORIENTED_EDGE('',*,*,#16463,.T.);
#22918=ORIENTED_EDGE('',*,*,#16464,.F.);
#22919=ORIENTED_EDGE('',*,*,#16463,.F.);
#22920=ORIENTED_EDGE('',*,*,#16464,.T.);
#22921=ORIENTED_EDGE('',*,*,#16465,.T.);
#22922=ORIENTED_EDGE('',*,*,#16466,.F.);
#22923=ORIENTED_EDGE('',*,*,#16465,.F.);
#22924=ORIENTED_EDGE('',*,*,#16443,.F.);
#22925=ORIENTED_EDGE('',*,*,#16466,.T.);
#22926=ORIENTED_EDGE('',*,*,#16467,.T.);
#22927=ORIENTED_EDGE('',*,*,#16468,.T.);
#22928=ORIENTED_EDGE('',*,*,#16469,.T.);
#22929=ORIENTED_EDGE('',*,*,#16470,.T.);
#22930=ORIENTED_EDGE('',*,*,#16468,.F.);
#22931=ORIENTED_EDGE('',*,*,#16469,.F.);
#22932=ORIENTED_EDGE('',*,*,#16470,.F.);
#22933=ORIENTED_EDGE('',*,*,#16471,.T.);
#22934=ORIENTED_EDGE('',*,*,#16472,.T.);
#22935=ORIENTED_EDGE('',*,*,#16471,.F.);
#22936=ORIENTED_EDGE('',*,*,#16467,.F.);
#22937=ORIENTED_EDGE('',*,*,#16473,.F.);
#22938=ORIENTED_EDGE('',*,*,#16474,.T.);
#22939=ORIENTED_EDGE('',*,*,#16475,.T.);
#22940=ORIENTED_EDGE('',*,*,#16476,.F.);
#22941=ORIENTED_EDGE('',*,*,#16475,.F.);
#22942=ORIENTED_EDGE('',*,*,#16477,.F.);
#22943=ORIENTED_EDGE('',*,*,#16476,.T.);
#22944=ORIENTED_EDGE('',*,*,#16472,.F.);
#22945=ORIENTED_EDGE('',*,*,#16478,.T.);
#22946=ORIENTED_EDGE('',*,*,#16477,.T.);
#22947=ORIENTED_EDGE('',*,*,#16478,.F.);
#22948=ORIENTED_EDGE('',*,*,#16479,.F.);
#22949=ORIENTED_EDGE('',*,*,#16480,.T.);
#22950=ORIENTED_EDGE('',*,*,#16473,.T.);
#22951=ORIENTED_EDGE('',*,*,#16480,.F.);
#22952=ORIENTED_EDGE('',*,*,#16479,.T.);
#22953=ORIENTED_EDGE('',*,*,#16481,.F.);
#22954=ORIENTED_EDGE('',*,*,#16481,.T.);
#22955=ORIENTED_EDGE('',*,*,#16482,.T.);
#22956=ORIENTED_EDGE('',*,*,#16483,.F.);
#22957=ORIENTED_EDGE('',*,*,#16482,.F.);
#22958=ORIENTED_EDGE('',*,*,#16483,.T.);
#22959=ORIENTED_EDGE('',*,*,#16474,.F.);
#22960=ORIENTED_EDGE('',*,*,#16484,.T.);
#22961=ORIENTED_EDGE('',*,*,#16485,.T.);
#22962=ORIENTED_EDGE('',*,*,#16486,.F.);
#22963=ORIENTED_EDGE('',*,*,#16485,.F.);
#22964=ORIENTED_EDGE('',*,*,#16487,.F.);
#22965=ORIENTED_EDGE('',*,*,#16486,.T.);
#22966=ORIENTED_EDGE('',*,*,#16488,.F.);
#22967=ORIENTED_EDGE('',*,*,#16489,.T.);
#22968=ORIENTED_EDGE('',*,*,#16487,.T.);
#22969=ORIENTED_EDGE('',*,*,#16489,.F.);
#22970=ORIENTED_EDGE('',*,*,#16490,.F.);
#22971=ORIENTED_EDGE('',*,*,#16491,.T.);
#22972=ORIENTED_EDGE('',*,*,#16488,.T.);
#22973=ORIENTED_EDGE('',*,*,#16491,.F.);
#22974=ORIENTED_EDGE('',*,*,#16490,.T.);
#22975=ORIENTED_EDGE('',*,*,#16484,.F.);
#22976=ORIENTED_EDGE('',*,*,#16492,.F.);
#22977=ORIENTED_EDGE('',*,*,#16493,.F.);
#22978=ORIENTED_EDGE('',*,*,#16494,.T.);
#22979=ORIENTED_EDGE('',*,*,#16492,.T.);
#22980=ORIENTED_EDGE('',*,*,#16494,.F.);
#22981=ORIENTED_EDGE('',*,*,#16495,.F.);
#22982=ORIENTED_EDGE('',*,*,#16496,.T.);
#22983=ORIENTED_EDGE('',*,*,#16493,.T.);
#22984=ORIENTED_EDGE('',*,*,#16496,.F.);
#22985=ORIENTED_EDGE('',*,*,#16497,.F.);
#22986=ORIENTED_EDGE('',*,*,#16498,.T.);
#22987=ORIENTED_EDGE('',*,*,#16495,.T.);
#22988=ORIENTED_EDGE('',*,*,#16498,.F.);
#22989=ORIENTED_EDGE('',*,*,#16497,.T.);
#22990=ORIENTED_EDGE('',*,*,#16499,.T.);
#22991=ORIENTED_EDGE('',*,*,#16500,.T.);
#22992=ORIENTED_EDGE('',*,*,#16501,.F.);
#22993=ORIENTED_EDGE('',*,*,#16500,.F.);
#22994=ORIENTED_EDGE('',*,*,#16502,.F.);
#22995=ORIENTED_EDGE('',*,*,#16501,.T.);
#22996=ORIENTED_EDGE('',*,*,#16503,.F.);
#22997=ORIENTED_EDGE('',*,*,#16504,.T.);
#22998=ORIENTED_EDGE('',*,*,#16502,.T.);
#22999=ORIENTED_EDGE('',*,*,#16504,.F.);
#23000=ORIENTED_EDGE('',*,*,#16503,.T.);
#23001=ORIENTED_EDGE('',*,*,#16499,.F.);
#23002=ORIENTED_EDGE('',*,*,#16505,.F.);
#23003=ORIENTED_EDGE('',*,*,#16506,.T.);
#23004=ORIENTED_EDGE('',*,*,#16505,.T.);
#23005=ORIENTED_EDGE('',*,*,#16506,.F.);
#23006=ORIENTED_EDGE('',*,*,#16507,.T.);
#23007=ORIENTED_EDGE('',*,*,#16508,.T.);
#23008=ORIENTED_EDGE('',*,*,#16509,.T.);
#23009=ORIENTED_EDGE('',*,*,#16510,.T.);
#23010=ORIENTED_EDGE('',*,*,#16511,.T.);
#23011=ORIENTED_EDGE('',*,*,#16512,.T.);
#23012=ORIENTED_EDGE('',*,*,#16513,.T.);
#23013=ORIENTED_EDGE('',*,*,#16510,.F.);
#23014=ORIENTED_EDGE('',*,*,#16514,.T.);
#23015=ORIENTED_EDGE('',*,*,#16515,.T.);
#23016=ORIENTED_EDGE('',*,*,#16516,.T.);
#23017=ORIENTED_EDGE('',*,*,#16512,.F.);
#23018=ORIENTED_EDGE('',*,*,#16514,.F.);
#23019=ORIENTED_EDGE('',*,*,#16511,.F.);
#23020=ORIENTED_EDGE('',*,*,#16509,.F.);
#23021=ORIENTED_EDGE('',*,*,#16517,.T.);
#23022=ORIENTED_EDGE('',*,*,#16518,.T.);
#23023=ORIENTED_EDGE('',*,*,#16519,.T.);
#23024=ORIENTED_EDGE('',*,*,#16520,.T.);
#23025=ORIENTED_EDGE('',*,*,#16521,.T.);
#23026=ORIENTED_EDGE('',*,*,#16522,.T.);
#23027=ORIENTED_EDGE('',*,*,#16523,.T.);
#23028=ORIENTED_EDGE('',*,*,#16524,.T.);
#23029=ORIENTED_EDGE('',*,*,#16525,.T.);
#23030=ORIENTED_EDGE('',*,*,#16526,.T.);
#23031=ORIENTED_EDGE('',*,*,#16525,.F.);
#23032=ORIENTED_EDGE('',*,*,#16527,.T.);
#23033=ORIENTED_EDGE('',*,*,#16521,.F.);
#23034=ORIENTED_EDGE('',*,*,#16518,.F.);
#23035=ORIENTED_EDGE('',*,*,#16527,.F.);
#23036=ORIENTED_EDGE('',*,*,#16524,.F.);
#23037=ORIENTED_EDGE('',*,*,#16528,.T.);
#23038=ORIENTED_EDGE('',*,*,#16516,.F.);
#23039=ORIENTED_EDGE('',*,*,#16529,.F.);
#23040=ORIENTED_EDGE('',*,*,#16522,.F.);
#23041=ORIENTED_EDGE('',*,*,#16530,.T.);
#23042=ORIENTED_EDGE('',*,*,#16513,.F.);
#23043=ORIENTED_EDGE('',*,*,#16530,.F.);
#23044=ORIENTED_EDGE('',*,*,#16526,.F.);
#23045=ORIENTED_EDGE('',*,*,#16531,.T.);
#23046=ORIENTED_EDGE('',*,*,#16515,.F.);
#23047=ORIENTED_EDGE('',*,*,#16517,.F.);
#23048=ORIENTED_EDGE('',*,*,#16508,.F.);
#23049=ORIENTED_EDGE('',*,*,#16532,.F.);
#23050=ORIENTED_EDGE('',*,*,#16519,.F.);
#23051=ORIENTED_EDGE('',*,*,#16528,.F.);
#23052=ORIENTED_EDGE('',*,*,#16523,.F.);
#23053=ORIENTED_EDGE('',*,*,#16529,.T.);
#23054=ORIENTED_EDGE('',*,*,#16507,.F.);
#23055=ORIENTED_EDGE('',*,*,#16531,.F.);
#23056=ORIENTED_EDGE('',*,*,#16520,.F.);
#23057=ORIENTED_EDGE('',*,*,#16532,.T.);
#23058=ORIENTED_EDGE('',*,*,#16533,.F.);
#23059=ORIENTED_EDGE('',*,*,#16534,.F.);
#23060=ORIENTED_EDGE('',*,*,#16535,.F.);
#23061=ORIENTED_EDGE('',*,*,#16536,.F.);
#23062=ORIENTED_EDGE('',*,*,#16537,.F.);
#23063=ORIENTED_EDGE('',*,*,#16538,.F.);
#23064=ORIENTED_EDGE('',*,*,#16539,.T.);
#23065=ORIENTED_EDGE('',*,*,#16540,.T.);
#23066=ORIENTED_EDGE('',*,*,#16537,.T.);
#23067=ORIENTED_EDGE('',*,*,#16541,.T.);
#23068=ORIENTED_EDGE('',*,*,#16542,.F.);
#23069=ORIENTED_EDGE('',*,*,#16543,.F.);
#23070=ORIENTED_EDGE('',*,*,#16544,.F.);
#23071=ORIENTED_EDGE('',*,*,#16545,.F.);
#23072=ORIENTED_EDGE('',*,*,#16546,.F.);
#23073=ORIENTED_EDGE('',*,*,#16547,.F.);
#23074=ORIENTED_EDGE('',*,*,#16538,.T.);
#23075=ORIENTED_EDGE('',*,*,#16548,.T.);
#23076=ORIENTED_EDGE('',*,*,#16546,.T.);
#23077=ORIENTED_EDGE('',*,*,#16549,.T.);
#23078=ORIENTED_EDGE('',*,*,#16550,.T.);
#23079=ORIENTED_EDGE('',*,*,#16551,.T.);
#23080=ORIENTED_EDGE('',*,*,#16547,.T.);
#23081=ORIENTED_EDGE('',*,*,#16552,.T.);
#23082=ORIENTED_EDGE('',*,*,#16543,.T.);
#23083=ORIENTED_EDGE('',*,*,#16553,.T.);
#23084=ORIENTED_EDGE('',*,*,#16545,.T.);
#23085=ORIENTED_EDGE('',*,*,#16554,.T.);
#23086=ORIENTED_EDGE('',*,*,#16555,.T.);
#23087=ORIENTED_EDGE('',*,*,#16556,.T.);
#23088=ORIENTED_EDGE('',*,*,#16544,.T.);
#23089=ORIENTED_EDGE('',*,*,#16557,.T.);
#23090=ORIENTED_EDGE('',*,*,#16542,.T.);
#23091=ORIENTED_EDGE('',*,*,#16558,.T.);
#23092=ORIENTED_EDGE('',*,*,#16535,.T.);
#23093=ORIENTED_EDGE('',*,*,#16559,.T.);
#23094=ORIENTED_EDGE('',*,*,#16534,.T.);
#23095=ORIENTED_EDGE('',*,*,#16560,.T.);
#23096=ORIENTED_EDGE('',*,*,#16536,.T.);
#23097=ORIENTED_EDGE('',*,*,#16561,.T.);
#23098=ORIENTED_EDGE('',*,*,#16562,.T.);
#23099=ORIENTED_EDGE('',*,*,#16563,.T.);
#23100=ORIENTED_EDGE('',*,*,#16533,.T.);
#23101=ORIENTED_EDGE('',*,*,#16564,.T.);
#23102=ORIENTED_EDGE('',*,*,#16552,.F.);
#23103=ORIENTED_EDGE('',*,*,#16548,.F.);
#23104=ORIENTED_EDGE('',*,*,#16540,.F.);
#23105=ORIENTED_EDGE('',*,*,#16565,.F.);
#23106=ORIENTED_EDGE('',*,*,#16541,.F.);
#23107=ORIENTED_EDGE('',*,*,#16560,.F.);
#23108=ORIENTED_EDGE('',*,*,#16563,.F.);
#23109=ORIENTED_EDGE('',*,*,#16566,.F.);
#23110=ORIENTED_EDGE('',*,*,#16549,.F.);
#23111=ORIENTED_EDGE('',*,*,#16553,.F.);
#23112=ORIENTED_EDGE('',*,*,#16559,.F.);
#23113=ORIENTED_EDGE('',*,*,#16561,.F.);
#23114=ORIENTED_EDGE('',*,*,#16550,.F.);
#23115=ORIENTED_EDGE('',*,*,#16565,.T.);
#23116=ORIENTED_EDGE('',*,*,#16539,.F.);
#23117=ORIENTED_EDGE('',*,*,#16566,.T.);
#23118=ORIENTED_EDGE('',*,*,#16562,.F.);
#23119=ORIENTED_EDGE('',*,*,#16567,.F.);
#23120=ORIENTED_EDGE('',*,*,#16555,.F.);
#23121=ORIENTED_EDGE('',*,*,#16568,.F.);
#23122=ORIENTED_EDGE('',*,*,#16551,.F.);
#23123=ORIENTED_EDGE('',*,*,#16568,.T.);
#23124=ORIENTED_EDGE('',*,*,#16557,.F.);
#23125=ORIENTED_EDGE('',*,*,#16554,.F.);
#23126=ORIENTED_EDGE('',*,*,#16556,.F.);
#23127=ORIENTED_EDGE('',*,*,#16567,.T.);
#23128=ORIENTED_EDGE('',*,*,#16564,.F.);
#23129=ORIENTED_EDGE('',*,*,#16558,.F.);
#23130=ORIENTED_EDGE('',*,*,#16569,.T.);
#23131=ORIENTED_EDGE('',*,*,#16570,.T.);
#23132=ORIENTED_EDGE('',*,*,#16571,.T.);
#23133=ORIENTED_EDGE('',*,*,#16570,.F.);
#23134=ORIENTED_EDGE('',*,*,#16572,.F.);
#23135=ORIENTED_EDGE('',*,*,#16573,.F.);
#23136=ORIENTED_EDGE('',*,*,#16574,.F.);
#23137=ORIENTED_EDGE('',*,*,#16575,.F.);
#23138=ORIENTED_EDGE('',*,*,#16576,.F.);
#23139=ORIENTED_EDGE('',*,*,#16577,.T.);
#23140=ORIENTED_EDGE('',*,*,#16571,.F.);
#23141=ORIENTED_EDGE('',*,*,#16577,.F.);
#23142=ORIENTED_EDGE('',*,*,#16578,.F.);
#23143=ORIENTED_EDGE('',*,*,#16579,.F.);
#23144=ORIENTED_EDGE('',*,*,#16569,.F.);
#23145=ORIENTED_EDGE('',*,*,#16580,.F.);
#23146=ORIENTED_EDGE('',*,*,#16581,.F.);
#23147=ORIENTED_EDGE('',*,*,#16582,.F.);
#23148=ORIENTED_EDGE('',*,*,#16583,.F.);
#23149=ORIENTED_EDGE('',*,*,#16584,.F.);
#23150=ORIENTED_EDGE('',*,*,#16585,.F.);
#23151=ORIENTED_EDGE('',*,*,#16586,.F.);
#23152=ORIENTED_EDGE('',*,*,#16587,.F.);
#23153=ORIENTED_EDGE('',*,*,#16588,.F.);
#23154=ORIENTED_EDGE('',*,*,#16589,.F.);
#23155=ORIENTED_EDGE('',*,*,#16590,.F.);
#23156=ORIENTED_EDGE('',*,*,#16591,.F.);
#23157=ORIENTED_EDGE('',*,*,#16592,.F.);
#23158=ORIENTED_EDGE('',*,*,#16593,.F.);
#23159=ORIENTED_EDGE('',*,*,#16594,.F.);
#23160=ORIENTED_EDGE('',*,*,#16595,.F.);
#23161=ORIENTED_EDGE('',*,*,#16596,.F.);
#23162=ORIENTED_EDGE('',*,*,#16597,.F.);
#23163=ORIENTED_EDGE('',*,*,#16593,.T.);
#23164=ORIENTED_EDGE('',*,*,#16598,.T.);
#23165=ORIENTED_EDGE('',*,*,#16596,.T.);
#23166=ORIENTED_EDGE('',*,*,#16572,.T.);
#23167=ORIENTED_EDGE('',*,*,#16599,.T.);
#23168=ORIENTED_EDGE('',*,*,#16600,.T.);
#23169=ORIENTED_EDGE('',*,*,#16597,.T.);
#23170=ORIENTED_EDGE('',*,*,#16601,.T.);
#23171=ORIENTED_EDGE('',*,*,#16595,.T.);
#23172=ORIENTED_EDGE('',*,*,#16602,.T.);
#23173=ORIENTED_EDGE('',*,*,#16590,.T.);
#23174=ORIENTED_EDGE('',*,*,#16573,.T.);
#23175=ORIENTED_EDGE('',*,*,#16587,.T.);
#23176=ORIENTED_EDGE('',*,*,#16603,.T.);
#23177=ORIENTED_EDGE('',*,*,#16594,.T.);
#23178=ORIENTED_EDGE('',*,*,#16579,.T.);
#23179=ORIENTED_EDGE('',*,*,#16604,.T.);
#23180=ORIENTED_EDGE('',*,*,#16605,.T.);
#23181=ORIENTED_EDGE('',*,*,#16592,.T.);
#23182=ORIENTED_EDGE('',*,*,#16606,.T.);
#23183=ORIENTED_EDGE('',*,*,#16607,.T.);
#23184=ORIENTED_EDGE('',*,*,#16608,.T.);
#23185=ORIENTED_EDGE('',*,*,#16591,.T.);
#23186=ORIENTED_EDGE('',*,*,#16609,.T.);
#23187=ORIENTED_EDGE('',*,*,#16589,.T.);
#23188=ORIENTED_EDGE('',*,*,#16610,.T.);
#23189=ORIENTED_EDGE('',*,*,#16584,.T.);
#23190=ORIENTED_EDGE('',*,*,#16574,.T.);
#23191=ORIENTED_EDGE('',*,*,#16581,.T.);
#23192=ORIENTED_EDGE('',*,*,#16611,.T.);
#23193=ORIENTED_EDGE('',*,*,#16588,.T.);
#23194=ORIENTED_EDGE('',*,*,#16578,.T.);
#23195=ORIENTED_EDGE('',*,*,#16576,.T.);
#23196=ORIENTED_EDGE('',*,*,#16612,.T.);
#23197=ORIENTED_EDGE('',*,*,#16613,.T.);
#23198=ORIENTED_EDGE('',*,*,#16586,.T.);
#23199=ORIENTED_EDGE('',*,*,#16614,.T.);
#23200=ORIENTED_EDGE('',*,*,#16615,.T.);
#23201=ORIENTED_EDGE('',*,*,#16616,.T.);
#23202=ORIENTED_EDGE('',*,*,#16585,.T.);
#23203=ORIENTED_EDGE('',*,*,#16617,.T.);
#23204=ORIENTED_EDGE('',*,*,#16583,.T.);
#23205=ORIENTED_EDGE('',*,*,#16618,.T.);
#23206=ORIENTED_EDGE('',*,*,#16582,.T.);
#23207=ORIENTED_EDGE('',*,*,#16575,.T.);
#23208=ORIENTED_EDGE('',*,*,#16619,.T.);
#23209=ORIENTED_EDGE('',*,*,#16620,.T.);
#23210=ORIENTED_EDGE('',*,*,#16580,.T.);
#23211=ORIENTED_EDGE('',*,*,#16621,.T.);
#23212=ORIENTED_EDGE('',*,*,#16604,.F.);
#23213=ORIENTED_EDGE('',*,*,#16622,.F.);
#23214=ORIENTED_EDGE('',*,*,#16623,.T.);
#23215=ORIENTED_EDGE('',*,*,#16624,.F.);
#23216=ORIENTED_EDGE('',*,*,#16606,.F.);
#23217=ORIENTED_EDGE('',*,*,#16603,.F.);
#23218=ORIENTED_EDGE('',*,*,#16613,.F.);
#23219=ORIENTED_EDGE('',*,*,#16625,.T.);
#23220=ORIENTED_EDGE('',*,*,#16626,.F.);
#23221=ORIENTED_EDGE('',*,*,#16622,.T.);
#23222=ORIENTED_EDGE('',*,*,#16612,.F.);
#23223=ORIENTED_EDGE('',*,*,#16627,.F.);
#23224=ORIENTED_EDGE('',*,*,#16628,.T.);
#23225=ORIENTED_EDGE('',*,*,#16625,.F.);
#23226=ORIENTED_EDGE('',*,*,#16614,.F.);
#23227=ORIENTED_EDGE('',*,*,#16611,.F.);
#23228=ORIENTED_EDGE('',*,*,#16620,.F.);
#23229=ORIENTED_EDGE('',*,*,#16629,.T.);
#23230=ORIENTED_EDGE('',*,*,#16630,.F.);
#23231=ORIENTED_EDGE('',*,*,#16627,.T.);
#23232=ORIENTED_EDGE('',*,*,#16619,.F.);
#23233=ORIENTED_EDGE('',*,*,#16631,.F.);
#23234=ORIENTED_EDGE('',*,*,#16632,.T.);
#23235=ORIENTED_EDGE('',*,*,#16629,.F.);
#23236=ORIENTED_EDGE('',*,*,#16621,.F.);
#23237=ORIENTED_EDGE('',*,*,#16618,.F.);
#23238=ORIENTED_EDGE('',*,*,#16616,.F.);
#23239=ORIENTED_EDGE('',*,*,#16633,.T.);
#23240=ORIENTED_EDGE('',*,*,#16634,.F.);
#23241=ORIENTED_EDGE('',*,*,#16631,.T.);
#23242=ORIENTED_EDGE('',*,*,#16608,.F.);
#23243=ORIENTED_EDGE('',*,*,#16635,.T.);
#23244=ORIENTED_EDGE('',*,*,#16636,.F.);
#23245=ORIENTED_EDGE('',*,*,#16637,.T.);
#23246=ORIENTED_EDGE('',*,*,#16617,.F.);
#23247=ORIENTED_EDGE('',*,*,#16610,.F.);
#23248=ORIENTED_EDGE('',*,*,#16600,.F.);
#23249=ORIENTED_EDGE('',*,*,#16638,.T.);
#23250=ORIENTED_EDGE('',*,*,#16639,.F.);
#23251=ORIENTED_EDGE('',*,*,#16640,.T.);
#23252=ORIENTED_EDGE('',*,*,#16609,.F.);
#23253=ORIENTED_EDGE('',*,*,#16602,.F.);
#23254=ORIENTED_EDGE('',*,*,#16599,.F.);
#23255=ORIENTED_EDGE('',*,*,#16641,.F.);
#23256=ORIENTED_EDGE('',*,*,#16642,.T.);
#23257=ORIENTED_EDGE('',*,*,#16638,.F.);
#23258=ORIENTED_EDGE('',*,*,#16607,.F.);
#23259=ORIENTED_EDGE('',*,*,#16640,.F.);
#23260=ORIENTED_EDGE('',*,*,#16643,.T.);
#23261=ORIENTED_EDGE('',*,*,#16635,.F.);
#23262=ORIENTED_EDGE('',*,*,#16615,.F.);
#23263=ORIENTED_EDGE('',*,*,#16637,.F.);
#23264=ORIENTED_EDGE('',*,*,#16644,.T.);
#23265=ORIENTED_EDGE('',*,*,#16633,.F.);
#23266=ORIENTED_EDGE('',*,*,#16605,.F.);
#23267=ORIENTED_EDGE('',*,*,#16624,.T.);
#23268=ORIENTED_EDGE('',*,*,#16645,.F.);
#23269=ORIENTED_EDGE('',*,*,#16641,.T.);
#23270=ORIENTED_EDGE('',*,*,#16601,.F.);
#23271=ORIENTED_EDGE('',*,*,#16598,.F.);
#23272=ORIENTED_EDGE('',*,*,#16634,.T.);
#23273=ORIENTED_EDGE('',*,*,#16646,.T.);
#23274=ORIENTED_EDGE('',*,*,#16636,.T.);
#23275=ORIENTED_EDGE('',*,*,#16647,.T.);
#23276=ORIENTED_EDGE('',*,*,#16639,.T.);
#23277=ORIENTED_EDGE('',*,*,#16648,.T.);
#23278=ORIENTED_EDGE('',*,*,#16645,.T.);
#23279=ORIENTED_EDGE('',*,*,#16649,.T.);
#23280=ORIENTED_EDGE('',*,*,#16626,.T.);
#23281=ORIENTED_EDGE('',*,*,#16650,.T.);
#23282=ORIENTED_EDGE('',*,*,#16630,.T.);
#23283=ORIENTED_EDGE('',*,*,#16651,.T.);
#23284=ORIENTED_EDGE('',*,*,#16652,.T.);
#23285=ORIENTED_EDGE('',*,*,#16653,.F.);
#23286=ORIENTED_EDGE('',*,*,#16654,.F.);
#23287=ORIENTED_EDGE('',*,*,#16655,.T.);
#23288=ORIENTED_EDGE('',*,*,#16653,.T.);
#23289=ORIENTED_EDGE('',*,*,#16655,.F.);
#23290=ORIENTED_EDGE('',*,*,#16648,.F.);
#23291=ORIENTED_EDGE('',*,*,#16642,.F.);
#23292=ORIENTED_EDGE('',*,*,#16649,.F.);
#23293=ORIENTED_EDGE('',*,*,#16623,.F.);
#23294=ORIENTED_EDGE('',*,*,#16650,.F.);
#23295=ORIENTED_EDGE('',*,*,#16628,.F.);
#23296=ORIENTED_EDGE('',*,*,#16652,.F.);
#23297=ORIENTED_EDGE('',*,*,#16656,.T.);
#23298=ORIENTED_EDGE('',*,*,#16654,.T.);
#23299=ORIENTED_EDGE('',*,*,#16656,.F.);
#23300=ORIENTED_EDGE('',*,*,#16651,.F.);
#23301=ORIENTED_EDGE('',*,*,#16632,.F.);
#23302=ORIENTED_EDGE('',*,*,#16646,.F.);
#23303=ORIENTED_EDGE('',*,*,#16644,.F.);
#23304=ORIENTED_EDGE('',*,*,#16647,.F.);
#23305=ORIENTED_EDGE('',*,*,#16643,.F.);
#23306=ORIENTED_EDGE('',*,*,#16657,.T.);
#23307=ORIENTED_EDGE('',*,*,#16658,.T.);
#23308=ORIENTED_EDGE('',*,*,#16659,.T.);
#23309=ORIENTED_EDGE('',*,*,#16660,.T.);
#23310=ORIENTED_EDGE('',*,*,#16661,.T.);
#23311=ORIENTED_EDGE('',*,*,#16662,.T.);
#23312=ORIENTED_EDGE('',*,*,#16657,.F.);
#23313=ORIENTED_EDGE('',*,*,#16663,.T.);
#23314=ORIENTED_EDGE('',*,*,#16664,.T.);
#23315=ORIENTED_EDGE('',*,*,#16665,.T.);
#23316=ORIENTED_EDGE('',*,*,#16661,.F.);
#23317=ORIENTED_EDGE('',*,*,#16666,.T.);
#23318=ORIENTED_EDGE('',*,*,#16667,.T.);
#23319=ORIENTED_EDGE('',*,*,#16668,.T.);
#23320=ORIENTED_EDGE('',*,*,#16664,.F.);
#23321=ORIENTED_EDGE('',*,*,#16669,.T.);
#23322=ORIENTED_EDGE('',*,*,#16670,.T.);
#23323=ORIENTED_EDGE('',*,*,#16671,.T.);
#23324=ORIENTED_EDGE('',*,*,#16667,.F.);
#23325=ORIENTED_EDGE('',*,*,#16672,.T.);
#23326=ORIENTED_EDGE('',*,*,#16673,.T.);
#23327=ORIENTED_EDGE('',*,*,#16674,.T.);
#23328=ORIENTED_EDGE('',*,*,#16670,.F.);
#23329=ORIENTED_EDGE('',*,*,#16675,.T.);
#23330=ORIENTED_EDGE('',*,*,#16676,.T.);
#23331=ORIENTED_EDGE('',*,*,#16677,.T.);
#23332=ORIENTED_EDGE('',*,*,#16673,.F.);
#23333=ORIENTED_EDGE('',*,*,#16678,.T.);
#23334=ORIENTED_EDGE('',*,*,#16659,.F.);
#23335=ORIENTED_EDGE('',*,*,#16679,.T.);
#23336=ORIENTED_EDGE('',*,*,#16676,.F.);
#23337=ORIENTED_EDGE('',*,*,#16680,.T.);
#23338=ORIENTED_EDGE('',*,*,#16669,.F.);
#23339=ORIENTED_EDGE('',*,*,#16681,.F.);
#23340=ORIENTED_EDGE('',*,*,#16682,.F.);
#23341=ORIENTED_EDGE('',*,*,#16683,.T.);
#23342=ORIENTED_EDGE('',*,*,#16666,.F.);
#23343=ORIENTED_EDGE('',*,*,#16684,.F.);
#23344=ORIENTED_EDGE('',*,*,#16685,.F.);
#23345=ORIENTED_EDGE('',*,*,#16681,.T.);
#23346=ORIENTED_EDGE('',*,*,#16663,.F.);
#23347=ORIENTED_EDGE('',*,*,#16686,.F.);
#23348=ORIENTED_EDGE('',*,*,#16687,.F.);
#23349=ORIENTED_EDGE('',*,*,#16684,.T.);
#23350=ORIENTED_EDGE('',*,*,#16660,.F.);
#23351=ORIENTED_EDGE('',*,*,#16688,.F.);
#23352=ORIENTED_EDGE('',*,*,#16689,.F.);
#23353=ORIENTED_EDGE('',*,*,#16686,.T.);
#23354=ORIENTED_EDGE('',*,*,#16658,.F.);
#23355=ORIENTED_EDGE('',*,*,#16662,.F.);
#23356=ORIENTED_EDGE('',*,*,#16665,.F.);
#23357=ORIENTED_EDGE('',*,*,#16668,.F.);
#23358=ORIENTED_EDGE('',*,*,#16671,.F.);
#23359=ORIENTED_EDGE('',*,*,#16674,.F.);
#23360=ORIENTED_EDGE('',*,*,#16677,.F.);
#23361=ORIENTED_EDGE('',*,*,#16679,.F.);
#23362=ORIENTED_EDGE('',*,*,#16690,.T.);
#23363=ORIENTED_EDGE('',*,*,#16691,.T.);
#23364=ORIENTED_EDGE('',*,*,#16692,.T.);
#23365=ORIENTED_EDGE('',*,*,#16693,.T.);
#23366=ORIENTED_EDGE('',*,*,#16694,.T.);
#23367=ORIENTED_EDGE('',*,*,#16695,.T.);
#23368=ORIENTED_EDGE('',*,*,#16696,.T.);
#23369=ORIENTED_EDGE('',*,*,#16697,.T.);
#23370=ORIENTED_EDGE('',*,*,#16698,.T.);
#23371=ORIENTED_EDGE('',*,*,#16699,.T.);
#23372=ORIENTED_EDGE('',*,*,#16700,.T.);
#23373=ORIENTED_EDGE('',*,*,#16701,.T.);
#23374=ORIENTED_EDGE('',*,*,#16702,.T.);
#23375=ORIENTED_EDGE('',*,*,#16703,.T.);
#23376=ORIENTED_EDGE('',*,*,#16704,.T.);
#23377=ORIENTED_EDGE('',*,*,#16689,.T.);
#23378=ORIENTED_EDGE('',*,*,#16705,.T.);
#23379=ORIENTED_EDGE('',*,*,#16706,.T.);
#23380=ORIENTED_EDGE('',*,*,#16702,.F.);
#23381=ORIENTED_EDGE('',*,*,#16707,.T.);
#23382=ORIENTED_EDGE('',*,*,#16708,.T.);
#23383=ORIENTED_EDGE('',*,*,#16709,.T.);
#23384=ORIENTED_EDGE('',*,*,#16705,.F.);
#23385=ORIENTED_EDGE('',*,*,#16710,.T.);
#23386=ORIENTED_EDGE('',*,*,#16711,.T.);
#23387=ORIENTED_EDGE('',*,*,#16712,.T.);
#23388=ORIENTED_EDGE('',*,*,#16708,.F.);
#23389=ORIENTED_EDGE('',*,*,#16713,.T.);
#23390=ORIENTED_EDGE('',*,*,#16714,.T.);
#23391=ORIENTED_EDGE('',*,*,#16715,.T.);
#23392=ORIENTED_EDGE('',*,*,#16711,.F.);
#23393=ORIENTED_EDGE('',*,*,#16716,.T.);
#23394=ORIENTED_EDGE('',*,*,#16717,.T.);
#23395=ORIENTED_EDGE('',*,*,#16718,.T.);
#23396=ORIENTED_EDGE('',*,*,#16714,.F.);
#23397=ORIENTED_EDGE('',*,*,#16682,.T.);
#23398=ORIENTED_EDGE('',*,*,#16719,.T.);
#23399=ORIENTED_EDGE('',*,*,#16720,.T.);
#23400=ORIENTED_EDGE('',*,*,#16717,.F.);
#23401=ORIENTED_EDGE('',*,*,#16685,.T.);
#23402=ORIENTED_EDGE('',*,*,#16704,.F.);
#23403=ORIENTED_EDGE('',*,*,#16721,.T.);
#23404=ORIENTED_EDGE('',*,*,#16719,.F.);
#23405=ORIENTED_EDGE('',*,*,#16687,.T.);
#23406=ORIENTED_EDGE('',*,*,#16675,.F.);
#23407=ORIENTED_EDGE('',*,*,#16722,.F.);
#23408=ORIENTED_EDGE('',*,*,#16713,.F.);
#23409=ORIENTED_EDGE('',*,*,#16723,.T.);
#23410=ORIENTED_EDGE('',*,*,#16678,.F.);
#23411=ORIENTED_EDGE('',*,*,#16723,.F.);
#23412=ORIENTED_EDGE('',*,*,#16710,.F.);
#23413=ORIENTED_EDGE('',*,*,#16724,.T.);
#23414=ORIENTED_EDGE('',*,*,#16680,.F.);
#23415=ORIENTED_EDGE('',*,*,#16724,.F.);
#23416=ORIENTED_EDGE('',*,*,#16707,.F.);
#23417=ORIENTED_EDGE('',*,*,#16688,.T.);
#23418=ORIENTED_EDGE('',*,*,#16703,.F.);
#23419=ORIENTED_EDGE('',*,*,#16706,.F.);
#23420=ORIENTED_EDGE('',*,*,#16709,.F.);
#23421=ORIENTED_EDGE('',*,*,#16712,.F.);
#23422=ORIENTED_EDGE('',*,*,#16715,.F.);
#23423=ORIENTED_EDGE('',*,*,#16718,.F.);
#23424=ORIENTED_EDGE('',*,*,#16720,.F.);
#23425=ORIENTED_EDGE('',*,*,#16721,.F.);
#23426=ORIENTED_EDGE('',*,*,#16725,.T.);
#23427=ORIENTED_EDGE('',*,*,#16726,.T.);
#23428=ORIENTED_EDGE('',*,*,#16727,.T.);
#23429=ORIENTED_EDGE('',*,*,#16728,.T.);
#23430=ORIENTED_EDGE('',*,*,#16729,.T.);
#23431=ORIENTED_EDGE('',*,*,#16730,.T.);
#23432=ORIENTED_EDGE('',*,*,#16731,.T.);
#23433=ORIENTED_EDGE('',*,*,#16732,.T.);
#23434=ORIENTED_EDGE('',*,*,#16733,.T.);
#23435=ORIENTED_EDGE('',*,*,#16734,.T.);
#23436=ORIENTED_EDGE('',*,*,#16729,.F.);
#23437=ORIENTED_EDGE('',*,*,#16735,.T.);
#23438=ORIENTED_EDGE('',*,*,#16736,.T.);
#23439=ORIENTED_EDGE('',*,*,#16737,.T.);
#23440=ORIENTED_EDGE('',*,*,#16733,.F.);
#23441=ORIENTED_EDGE('',*,*,#16738,.T.);
#23442=ORIENTED_EDGE('',*,*,#16739,.T.);
#23443=ORIENTED_EDGE('',*,*,#16740,.T.);
#23444=ORIENTED_EDGE('',*,*,#16736,.F.);
#23445=ORIENTED_EDGE('',*,*,#16741,.T.);
#23446=ORIENTED_EDGE('',*,*,#16742,.T.);
#23447=ORIENTED_EDGE('',*,*,#16743,.T.);
#23448=ORIENTED_EDGE('',*,*,#16739,.F.);
#23449=ORIENTED_EDGE('',*,*,#16744,.T.);
#23450=ORIENTED_EDGE('',*,*,#16745,.T.);
#23451=ORIENTED_EDGE('',*,*,#16746,.T.);
#23452=ORIENTED_EDGE('',*,*,#16742,.F.);
#23453=ORIENTED_EDGE('',*,*,#16747,.T.);
#23454=ORIENTED_EDGE('',*,*,#16748,.T.);
#23455=ORIENTED_EDGE('',*,*,#16749,.T.);
#23456=ORIENTED_EDGE('',*,*,#16745,.F.);
#23457=ORIENTED_EDGE('',*,*,#16750,.T.);
#23458=ORIENTED_EDGE('',*,*,#16731,.F.);
#23459=ORIENTED_EDGE('',*,*,#16751,.T.);
#23460=ORIENTED_EDGE('',*,*,#16748,.F.);
#23461=ORIENTED_EDGE('',*,*,#16752,.T.);
#23462=ORIENTED_EDGE('',*,*,#16741,.F.);
#23463=ORIENTED_EDGE('',*,*,#16753,.F.);
#23464=ORIENTED_EDGE('',*,*,#16699,.F.);
#23465=ORIENTED_EDGE('',*,*,#16754,.T.);
#23466=ORIENTED_EDGE('',*,*,#16738,.F.);
#23467=ORIENTED_EDGE('',*,*,#16755,.F.);
#23468=ORIENTED_EDGE('',*,*,#16700,.F.);
#23469=ORIENTED_EDGE('',*,*,#16753,.T.);
#23470=ORIENTED_EDGE('',*,*,#16735,.F.);
#23471=ORIENTED_EDGE('',*,*,#16756,.F.);
#23472=ORIENTED_EDGE('',*,*,#16701,.F.);
#23473=ORIENTED_EDGE('',*,*,#16755,.T.);
#23474=ORIENTED_EDGE('',*,*,#16732,.F.);
#23475=ORIENTED_EDGE('',*,*,#16757,.F.);
#23476=ORIENTED_EDGE('',*,*,#16694,.F.);
#23477=ORIENTED_EDGE('',*,*,#16756,.T.);
#23478=ORIENTED_EDGE('',*,*,#16730,.F.);
#23479=ORIENTED_EDGE('',*,*,#16734,.F.);
#23480=ORIENTED_EDGE('',*,*,#16737,.F.);
#23481=ORIENTED_EDGE('',*,*,#16740,.F.);
#23482=ORIENTED_EDGE('',*,*,#16743,.F.);
#23483=ORIENTED_EDGE('',*,*,#16746,.F.);
#23484=ORIENTED_EDGE('',*,*,#16749,.F.);
#23485=ORIENTED_EDGE('',*,*,#16751,.F.);
#23486=ORIENTED_EDGE('',*,*,#16752,.F.);
#23487=ORIENTED_EDGE('',*,*,#16758,.F.);
#23488=ORIENTED_EDGE('',*,*,#16695,.F.);
#23489=ORIENTED_EDGE('',*,*,#16757,.T.);
#23490=ORIENTED_EDGE('',*,*,#16750,.F.);
#23491=ORIENTED_EDGE('',*,*,#16759,.F.);
#23492=ORIENTED_EDGE('',*,*,#16696,.F.);
#23493=ORIENTED_EDGE('',*,*,#16758,.T.);
#23494=ORIENTED_EDGE('',*,*,#16747,.F.);
#23495=ORIENTED_EDGE('',*,*,#16760,.F.);
#23496=ORIENTED_EDGE('',*,*,#16697,.F.);
#23497=ORIENTED_EDGE('',*,*,#16759,.T.);
#23498=ORIENTED_EDGE('',*,*,#16744,.F.);
#23499=ORIENTED_EDGE('',*,*,#16754,.F.);
#23500=ORIENTED_EDGE('',*,*,#16698,.F.);
#23501=ORIENTED_EDGE('',*,*,#16760,.T.);
#23502=ORIENTED_EDGE('',*,*,#16728,.F.);
#23503=ORIENTED_EDGE('',*,*,#16761,.T.);
#23504=ORIENTED_EDGE('',*,*,#16693,.F.);
#23505=ORIENTED_EDGE('',*,*,#16761,.F.);
#23506=ORIENTED_EDGE('',*,*,#16727,.F.);
#23507=ORIENTED_EDGE('',*,*,#16762,.T.);
#23508=ORIENTED_EDGE('',*,*,#16692,.F.);
#23509=ORIENTED_EDGE('',*,*,#16762,.F.);
#23510=ORIENTED_EDGE('',*,*,#16726,.F.);
#23511=ORIENTED_EDGE('',*,*,#16763,.T.);
#23512=ORIENTED_EDGE('',*,*,#16691,.F.);
#23513=ORIENTED_EDGE('',*,*,#16763,.F.);
#23514=ORIENTED_EDGE('',*,*,#16725,.F.);
#23515=ORIENTED_EDGE('',*,*,#16764,.T.);
#23516=ORIENTED_EDGE('',*,*,#16690,.F.);
#23517=ORIENTED_EDGE('',*,*,#16764,.F.);
#23518=ORIENTED_EDGE('',*,*,#16672,.F.);
#23519=ORIENTED_EDGE('',*,*,#16683,.F.);
#23520=ORIENTED_EDGE('',*,*,#16716,.F.);
#23521=ORIENTED_EDGE('',*,*,#16722,.T.);
#23522=ORIENTED_EDGE('',*,*,#16765,.T.);
#23523=ORIENTED_EDGE('',*,*,#16766,.T.);
#23524=ORIENTED_EDGE('',*,*,#16767,.T.);
#23525=ORIENTED_EDGE('',*,*,#16768,.T.);
#23526=ORIENTED_EDGE('',*,*,#16769,.T.);
#23527=ORIENTED_EDGE('',*,*,#16770,.F.);
#23528=ORIENTED_EDGE('',*,*,#16767,.F.);
#23529=ORIENTED_EDGE('',*,*,#16771,.T.);
#23530=ORIENTED_EDGE('',*,*,#16772,.F.);
#23531=ORIENTED_EDGE('',*,*,#16773,.F.);
#23532=ORIENTED_EDGE('',*,*,#16771,.F.);
#23533=ORIENTED_EDGE('',*,*,#16766,.F.);
#23534=ORIENTED_EDGE('',*,*,#16774,.F.);
#23535=ORIENTED_EDGE('',*,*,#16775,.T.);
#23536=ORIENTED_EDGE('',*,*,#16776,.T.);
#23537=ORIENTED_EDGE('',*,*,#16777,.F.);
#23538=ORIENTED_EDGE('',*,*,#16778,.F.);
#23539=ORIENTED_EDGE('',*,*,#16779,.F.);
#23540=ORIENTED_EDGE('',*,*,#16780,.F.);
#23541=ORIENTED_EDGE('',*,*,#16781,.T.);
#23542=ORIENTED_EDGE('',*,*,#16782,.T.);
#23543=ORIENTED_EDGE('',*,*,#16783,.F.);
#23544=ORIENTED_EDGE('',*,*,#16784,.F.);
#23545=ORIENTED_EDGE('',*,*,#16785,.T.);
#23546=ORIENTED_EDGE('',*,*,#16786,.F.);
#23547=ORIENTED_EDGE('',*,*,#16787,.F.);
#23548=ORIENTED_EDGE('',*,*,#16788,.F.);
#23549=ORIENTED_EDGE('',*,*,#16789,.T.);
#23550=ORIENTED_EDGE('',*,*,#16790,.T.);
#23551=ORIENTED_EDGE('',*,*,#16791,.F.);
#23552=ORIENTED_EDGE('',*,*,#16792,.F.);
#23553=ORIENTED_EDGE('',*,*,#16793,.T.);
#23554=ORIENTED_EDGE('',*,*,#16794,.T.);
#23555=ORIENTED_EDGE('',*,*,#16795,.T.);
#23556=ORIENTED_EDGE('',*,*,#16796,.T.);
#23557=ORIENTED_EDGE('',*,*,#16797,.T.);
#23558=ORIENTED_EDGE('',*,*,#16796,.F.);
#23559=ORIENTED_EDGE('',*,*,#16798,.F.);
#23560=ORIENTED_EDGE('',*,*,#16799,.F.);
#23561=ORIENTED_EDGE('',*,*,#16800,.T.);
#23562=ORIENTED_EDGE('',*,*,#16794,.F.);
#23563=ORIENTED_EDGE('',*,*,#16795,.F.);
#23564=ORIENTED_EDGE('',*,*,#16800,.F.);
#23565=ORIENTED_EDGE('',*,*,#16797,.F.);
#23566=ORIENTED_EDGE('',*,*,#16801,.T.);
#23567=ORIENTED_EDGE('',*,*,#16802,.T.);
#23568=ORIENTED_EDGE('',*,*,#16803,.T.);
#23569=ORIENTED_EDGE('',*,*,#16804,.T.);
#23570=ORIENTED_EDGE('',*,*,#16779,.T.);
#23571=ORIENTED_EDGE('',*,*,#16805,.T.);
#23572=ORIENTED_EDGE('',*,*,#16787,.T.);
#23573=ORIENTED_EDGE('',*,*,#16806,.T.);
#23574=ORIENTED_EDGE('',*,*,#16807,.T.);
#23575=ORIENTED_EDGE('',*,*,#16808,.F.);
#23576=ORIENTED_EDGE('',*,*,#16809,.F.);
#23577=ORIENTED_EDGE('',*,*,#16810,.F.);
#23578=ORIENTED_EDGE('',*,*,#16811,.T.);
#23579=ORIENTED_EDGE('',*,*,#16812,.T.);
#23580=ORIENTED_EDGE('',*,*,#16809,.T.);
#23581=ORIENTED_EDGE('',*,*,#16813,.T.);
#23582=ORIENTED_EDGE('',*,*,#16814,.F.);
#23583=ORIENTED_EDGE('',*,*,#16815,.F.);
#23584=ORIENTED_EDGE('',*,*,#16816,.F.);
#23585=ORIENTED_EDGE('',*,*,#16817,.F.);
#23586=ORIENTED_EDGE('',*,*,#16818,.F.);
#23587=ORIENTED_EDGE('',*,*,#16819,.F.);
#23588=ORIENTED_EDGE('',*,*,#16820,.T.);
#23589=ORIENTED_EDGE('',*,*,#16821,.T.);
#23590=ORIENTED_EDGE('',*,*,#16818,.T.);
#23591=ORIENTED_EDGE('',*,*,#16822,.T.);
#23592=ORIENTED_EDGE('',*,*,#16808,.T.);
#23593=ORIENTED_EDGE('',*,*,#16823,.T.);
#23594=ORIENTED_EDGE('',*,*,#16819,.T.);
#23595=ORIENTED_EDGE('',*,*,#16824,.T.);
#23596=ORIENTED_EDGE('',*,*,#16825,.F.);
#23597=ORIENTED_EDGE('',*,*,#16826,.F.);
#23598=ORIENTED_EDGE('',*,*,#16827,.F.);
#23599=ORIENTED_EDGE('',*,*,#16784,.T.);
#23600=ORIENTED_EDGE('',*,*,#16828,.T.);
#23601=ORIENTED_EDGE('',*,*,#16826,.T.);
#23602=ORIENTED_EDGE('',*,*,#16829,.T.);
#23603=ORIENTED_EDGE('',*,*,#16830,.F.);
#23604=ORIENTED_EDGE('',*,*,#16831,.F.);
#23605=ORIENTED_EDGE('',*,*,#16832,.F.);
#23606=ORIENTED_EDGE('',*,*,#16833,.F.);
#23607=ORIENTED_EDGE('',*,*,#16834,.F.);
#23608=ORIENTED_EDGE('',*,*,#16835,.F.);
#23609=ORIENTED_EDGE('',*,*,#16834,.T.);
#23610=ORIENTED_EDGE('',*,*,#16836,.T.);
#23611=ORIENTED_EDGE('',*,*,#16827,.T.);
#23612=ORIENTED_EDGE('',*,*,#16837,.T.);
#23613=ORIENTED_EDGE('',*,*,#16782,.F.);
#23614=ORIENTED_EDGE('',*,*,#16838,.T.);
#23615=ORIENTED_EDGE('',*,*,#16835,.T.);
#23616=ORIENTED_EDGE('',*,*,#16839,.T.);
#23617=ORIENTED_EDGE('',*,*,#16831,.T.);
#23618=ORIENTED_EDGE('',*,*,#16840,.T.);
#23619=ORIENTED_EDGE('',*,*,#16833,.T.);
#23620=ORIENTED_EDGE('',*,*,#16841,.T.);
#23621=ORIENTED_EDGE('',*,*,#16817,.T.);
#23622=ORIENTED_EDGE('',*,*,#16842,.T.);
#23623=ORIENTED_EDGE('',*,*,#16832,.T.);
#23624=ORIENTED_EDGE('',*,*,#16843,.T.);
#23625=ORIENTED_EDGE('',*,*,#16830,.T.);
#23626=ORIENTED_EDGE('',*,*,#16844,.T.);
#23627=ORIENTED_EDGE('',*,*,#16816,.T.);
#23628=ORIENTED_EDGE('',*,*,#16845,.T.);
#23629=ORIENTED_EDGE('',*,*,#16815,.T.);
#23630=ORIENTED_EDGE('',*,*,#16846,.T.);
#23631=ORIENTED_EDGE('',*,*,#16825,.T.);
#23632=ORIENTED_EDGE('',*,*,#16847,.T.);
#23633=ORIENTED_EDGE('',*,*,#16814,.T.);
#23634=ORIENTED_EDGE('',*,*,#16848,.T.);
#23635=ORIENTED_EDGE('',*,*,#16810,.T.);
#23636=ORIENTED_EDGE('',*,*,#16849,.T.);
#23637=ORIENTED_EDGE('',*,*,#16785,.F.);
#23638=ORIENTED_EDGE('',*,*,#16829,.F.);
#23639=ORIENTED_EDGE('',*,*,#16846,.F.);
#23640=ORIENTED_EDGE('',*,*,#16849,.F.);
#23641=ORIENTED_EDGE('',*,*,#16812,.F.);
#23642=ORIENTED_EDGE('',*,*,#16850,.F.);
#23643=ORIENTED_EDGE('',*,*,#16806,.F.);
#23644=ORIENTED_EDGE('',*,*,#16786,.T.);
#23645=ORIENTED_EDGE('',*,*,#16813,.F.);
#23646=ORIENTED_EDGE('',*,*,#16824,.F.);
#23647=ORIENTED_EDGE('',*,*,#16821,.F.);
#23648=ORIENTED_EDGE('',*,*,#16851,.F.);
#23649=ORIENTED_EDGE('',*,*,#16823,.F.);
#23650=ORIENTED_EDGE('',*,*,#16848,.F.);
#23651=ORIENTED_EDGE('',*,*,#16844,.F.);
#23652=ORIENTED_EDGE('',*,*,#16842,.F.);
#23653=ORIENTED_EDGE('',*,*,#16836,.F.);
#23654=ORIENTED_EDGE('',*,*,#16840,.F.);
#23655=ORIENTED_EDGE('',*,*,#16845,.F.);
#23656=ORIENTED_EDGE('',*,*,#16847,.F.);
#23657=ORIENTED_EDGE('',*,*,#16852,.T.);
#23658=ORIENTED_EDGE('',*,*,#16853,.T.);
#23659=ORIENTED_EDGE('',*,*,#16854,.T.);
#23660=ORIENTED_EDGE('',*,*,#16798,.T.);
#23661=ORIENTED_EDGE('',*,*,#16799,.T.);
#23662=ORIENTED_EDGE('',*,*,#16854,.F.);
#23663=ORIENTED_EDGE('',*,*,#16855,.F.);
#23664=ORIENTED_EDGE('',*,*,#16856,.F.);
#23665=ORIENTED_EDGE('',*,*,#16857,.T.);
#23666=ORIENTED_EDGE('',*,*,#16852,.F.);
#23667=ORIENTED_EDGE('',*,*,#16853,.F.);
#23668=ORIENTED_EDGE('',*,*,#16857,.F.);
#23669=ORIENTED_EDGE('',*,*,#16858,.F.);
#23670=ORIENTED_EDGE('',*,*,#16772,.T.);
#23671=ORIENTED_EDGE('',*,*,#16773,.T.);
#23672=ORIENTED_EDGE('',*,*,#16859,.T.);
#23673=ORIENTED_EDGE('',*,*,#16855,.T.);
#23674=ORIENTED_EDGE('',*,*,#16856,.T.);
#23675=ORIENTED_EDGE('',*,*,#16859,.F.);
#23676=ORIENTED_EDGE('',*,*,#16860,.F.);
#23677=ORIENTED_EDGE('',*,*,#16861,.F.);
#23678=ORIENTED_EDGE('',*,*,#16862,.F.);
#23679=ORIENTED_EDGE('',*,*,#16863,.T.);
#23680=ORIENTED_EDGE('',*,*,#16864,.T.);
#23681=ORIENTED_EDGE('',*,*,#16861,.T.);
#23682=ORIENTED_EDGE('',*,*,#16865,.T.);
#23683=ORIENTED_EDGE('',*,*,#16866,.T.);
#23684=ORIENTED_EDGE('',*,*,#16867,.T.);
#23685=ORIENTED_EDGE('',*,*,#16862,.T.);
#23686=ORIENTED_EDGE('',*,*,#16868,.T.);
#23687=ORIENTED_EDGE('',*,*,#16869,.T.);
#23688=ORIENTED_EDGE('',*,*,#16870,.T.);
#23689=ORIENTED_EDGE('',*,*,#16871,.T.);
#23690=ORIENTED_EDGE('',*,*,#16860,.T.);
#23691=ORIENTED_EDGE('',*,*,#16872,.T.);
#23692=ORIENTED_EDGE('',*,*,#16873,.T.);
#23693=ORIENTED_EDGE('',*,*,#16868,.F.);
#23694=ORIENTED_EDGE('',*,*,#16864,.F.);
#23695=ORIENTED_EDGE('',*,*,#16874,.F.);
#23696=ORIENTED_EDGE('',*,*,#16802,.F.);
#23697=ORIENTED_EDGE('',*,*,#16778,.T.);
#23698=ORIENTED_EDGE('',*,*,#16875,.T.);
#23699=ORIENTED_EDGE('',*,*,#16876,.F.);
#23700=ORIENTED_EDGE('',*,*,#16877,.F.);
#23701=ORIENTED_EDGE('',*,*,#16865,.F.);
#23702=ORIENTED_EDGE('',*,*,#16871,.F.);
#23703=ORIENTED_EDGE('',*,*,#16878,.F.);
#23704=ORIENTED_EDGE('',*,*,#16879,.F.);
#23705=ORIENTED_EDGE('',*,*,#16870,.F.);
#23706=ORIENTED_EDGE('',*,*,#16880,.T.);
#23707=ORIENTED_EDGE('',*,*,#16881,.T.);
#23708=ORIENTED_EDGE('',*,*,#16882,.T.);
#23709=ORIENTED_EDGE('',*,*,#16878,.T.);
#23710=ORIENTED_EDGE('',*,*,#16883,.F.);
#23711=ORIENTED_EDGE('',*,*,#16884,.F.);
#23712=ORIENTED_EDGE('',*,*,#16885,.F.);
#23713=ORIENTED_EDGE('',*,*,#16886,.F.);
#23714=ORIENTED_EDGE('',*,*,#16887,.F.);
#23715=ORIENTED_EDGE('',*,*,#16888,.F.);
#23716=ORIENTED_EDGE('',*,*,#16889,.T.);
#23717=ORIENTED_EDGE('',*,*,#16887,.T.);
#23718=ORIENTED_EDGE('',*,*,#16890,.T.);
#23719=ORIENTED_EDGE('',*,*,#16891,.T.);
#23720=ORIENTED_EDGE('',*,*,#16876,.T.);
#23721=ORIENTED_EDGE('',*,*,#16776,.F.);
#23722=ORIENTED_EDGE('',*,*,#16892,.T.);
#23723=ORIENTED_EDGE('',*,*,#16888,.T.);
#23724=ORIENTED_EDGE('',*,*,#16893,.T.);
#23725=ORIENTED_EDGE('',*,*,#16884,.T.);
#23726=ORIENTED_EDGE('',*,*,#16894,.T.);
#23727=ORIENTED_EDGE('',*,*,#16886,.T.);
#23728=ORIENTED_EDGE('',*,*,#16895,.T.);
#23729=ORIENTED_EDGE('',*,*,#16873,.F.);
#23730=ORIENTED_EDGE('',*,*,#16896,.T.);
#23731=ORIENTED_EDGE('',*,*,#16885,.T.);
#23732=ORIENTED_EDGE('',*,*,#16897,.T.);
#23733=ORIENTED_EDGE('',*,*,#16880,.F.);
#23734=ORIENTED_EDGE('',*,*,#16866,.F.);
#23735=ORIENTED_EDGE('',*,*,#16898,.F.);
#23736=ORIENTED_EDGE('',*,*,#16899,.T.);
#23737=ORIENTED_EDGE('',*,*,#16883,.T.);
#23738=ORIENTED_EDGE('',*,*,#16900,.T.);
#23739=ORIENTED_EDGE('',*,*,#16869,.F.);
#23740=ORIENTED_EDGE('',*,*,#16877,.T.);
#23741=ORIENTED_EDGE('',*,*,#16891,.F.);
#23742=ORIENTED_EDGE('',*,*,#16901,.T.);
#23743=ORIENTED_EDGE('',*,*,#16898,.T.);
#23744=ORIENTED_EDGE('',*,*,#16881,.F.);
#23745=ORIENTED_EDGE('',*,*,#16897,.F.);
#23746=ORIENTED_EDGE('',*,*,#16895,.F.);
#23747=ORIENTED_EDGE('',*,*,#16892,.F.);
#23748=ORIENTED_EDGE('',*,*,#16775,.F.);
#23749=ORIENTED_EDGE('',*,*,#16774,.T.);
#23750=ORIENTED_EDGE('',*,*,#16765,.F.);
#23751=ORIENTED_EDGE('',*,*,#16902,.F.);
#23752=ORIENTED_EDGE('',*,*,#16893,.F.);
#23753=ORIENTED_EDGE('',*,*,#16889,.F.);
#23754=ORIENTED_EDGE('',*,*,#16875,.F.);
#23755=ORIENTED_EDGE('',*,*,#16777,.T.);
#23756=ORIENTED_EDGE('',*,*,#16890,.F.);
#23757=ORIENTED_EDGE('',*,*,#16894,.F.);
#23758=ORIENTED_EDGE('',*,*,#16899,.F.);
#23759=ORIENTED_EDGE('',*,*,#16901,.F.);
#23760=ORIENTED_EDGE('',*,*,#16903,.F.);
#23761=ORIENTED_EDGE('',*,*,#16904,.F.);
#23762=ORIENTED_EDGE('',*,*,#16905,.F.);
#23763=ORIENTED_EDGE('',*,*,#16906,.T.);
#23764=ORIENTED_EDGE('',*,*,#16907,.T.);
#23765=ORIENTED_EDGE('',*,*,#16904,.T.);
#23766=ORIENTED_EDGE('',*,*,#16908,.T.);
#23767=ORIENTED_EDGE('',*,*,#16909,.F.);
#23768=ORIENTED_EDGE('',*,*,#16910,.F.);
#23769=ORIENTED_EDGE('',*,*,#16911,.F.);
#23770=ORIENTED_EDGE('',*,*,#16912,.F.);
#23771=ORIENTED_EDGE('',*,*,#16913,.F.);
#23772=ORIENTED_EDGE('',*,*,#16914,.F.);
#23773=ORIENTED_EDGE('',*,*,#16915,.T.);
#23774=ORIENTED_EDGE('',*,*,#16916,.T.);
#23775=ORIENTED_EDGE('',*,*,#16913,.T.);
#23776=ORIENTED_EDGE('',*,*,#16917,.T.);
#23777=ORIENTED_EDGE('',*,*,#16903,.T.);
#23778=ORIENTED_EDGE('',*,*,#16918,.T.);
#23779=ORIENTED_EDGE('',*,*,#16914,.T.);
#23780=ORIENTED_EDGE('',*,*,#16919,.T.);
#23781=ORIENTED_EDGE('',*,*,#16920,.F.);
#23782=ORIENTED_EDGE('',*,*,#16921,.F.);
#23783=ORIENTED_EDGE('',*,*,#16922,.F.);
#23784=ORIENTED_EDGE('',*,*,#16792,.T.);
#23785=ORIENTED_EDGE('',*,*,#16923,.T.);
#23786=ORIENTED_EDGE('',*,*,#16921,.T.);
#23787=ORIENTED_EDGE('',*,*,#16924,.T.);
#23788=ORIENTED_EDGE('',*,*,#16925,.F.);
#23789=ORIENTED_EDGE('',*,*,#16926,.F.);
#23790=ORIENTED_EDGE('',*,*,#16927,.F.);
#23791=ORIENTED_EDGE('',*,*,#16928,.F.);
#23792=ORIENTED_EDGE('',*,*,#16929,.F.);
#23793=ORIENTED_EDGE('',*,*,#16930,.F.);
#23794=ORIENTED_EDGE('',*,*,#16929,.T.);
#23795=ORIENTED_EDGE('',*,*,#16931,.T.);
#23796=ORIENTED_EDGE('',*,*,#16922,.T.);
#23797=ORIENTED_EDGE('',*,*,#16932,.T.);
#23798=ORIENTED_EDGE('',*,*,#16790,.F.);
#23799=ORIENTED_EDGE('',*,*,#16933,.T.);
#23800=ORIENTED_EDGE('',*,*,#16930,.T.);
#23801=ORIENTED_EDGE('',*,*,#16934,.T.);
#23802=ORIENTED_EDGE('',*,*,#16926,.T.);
#23803=ORIENTED_EDGE('',*,*,#16935,.T.);
#23804=ORIENTED_EDGE('',*,*,#16928,.T.);
#23805=ORIENTED_EDGE('',*,*,#16936,.T.);
#23806=ORIENTED_EDGE('',*,*,#16912,.T.);
#23807=ORIENTED_EDGE('',*,*,#16937,.T.);
#23808=ORIENTED_EDGE('',*,*,#16927,.T.);
#23809=ORIENTED_EDGE('',*,*,#16938,.T.);
#23810=ORIENTED_EDGE('',*,*,#16925,.T.);
#23811=ORIENTED_EDGE('',*,*,#16939,.T.);
#23812=ORIENTED_EDGE('',*,*,#16911,.T.);
#23813=ORIENTED_EDGE('',*,*,#16940,.T.);
#23814=ORIENTED_EDGE('',*,*,#16910,.T.);
#23815=ORIENTED_EDGE('',*,*,#16941,.T.);
#23816=ORIENTED_EDGE('',*,*,#16920,.T.);
#23817=ORIENTED_EDGE('',*,*,#16942,.T.);
#23818=ORIENTED_EDGE('',*,*,#16909,.T.);
#23819=ORIENTED_EDGE('',*,*,#16943,.T.);
#23820=ORIENTED_EDGE('',*,*,#16905,.T.);
#23821=ORIENTED_EDGE('',*,*,#16944,.T.);
#23822=ORIENTED_EDGE('',*,*,#16793,.F.);
#23823=ORIENTED_EDGE('',*,*,#16924,.F.);
#23824=ORIENTED_EDGE('',*,*,#16941,.F.);
#23825=ORIENTED_EDGE('',*,*,#16944,.F.);
#23826=ORIENTED_EDGE('',*,*,#16907,.F.);
#23827=ORIENTED_EDGE('',*,*,#16945,.F.);
#23828=ORIENTED_EDGE('',*,*,#16768,.F.);
#23829=ORIENTED_EDGE('',*,*,#16770,.T.);
#23830=ORIENTED_EDGE('',*,*,#16908,.F.);
#23831=ORIENTED_EDGE('',*,*,#16919,.F.);
#23832=ORIENTED_EDGE('',*,*,#16916,.F.);
#23833=ORIENTED_EDGE('',*,*,#16946,.F.);
#23834=ORIENTED_EDGE('',*,*,#16918,.F.);
#23835=ORIENTED_EDGE('',*,*,#16943,.F.);
#23836=ORIENTED_EDGE('',*,*,#16939,.F.);
#23837=ORIENTED_EDGE('',*,*,#16937,.F.);
#23838=ORIENTED_EDGE('',*,*,#16931,.F.);
#23839=ORIENTED_EDGE('',*,*,#16935,.F.);
#23840=ORIENTED_EDGE('',*,*,#16940,.F.);
#23841=ORIENTED_EDGE('',*,*,#16942,.F.);
#23842=ORIENTED_EDGE('',*,*,#16947,.T.);
#23843=ORIENTED_EDGE('',*,*,#16948,.T.);
#23844=ORIENTED_EDGE('',*,*,#16947,.F.);
#23845=ORIENTED_EDGE('',*,*,#16858,.T.);
#23846=ORIENTED_EDGE('',*,*,#16948,.F.);
#23847=ORIENTED_EDGE('',*,*,#16949,.T.);
#23848=ORIENTED_EDGE('',*,*,#16950,.T.);
#23849=ORIENTED_EDGE('',*,*,#16951,.T.);
#23850=ORIENTED_EDGE('',*,*,#16949,.F.);
#23851=ORIENTED_EDGE('',*,*,#16952,.T.);
#23852=ORIENTED_EDGE('',*,*,#16951,.F.);
#23853=ORIENTED_EDGE('',*,*,#16953,.F.);
#23854=ORIENTED_EDGE('',*,*,#16950,.F.);
#23855=ORIENTED_EDGE('',*,*,#16789,.F.);
#23856=ORIENTED_EDGE('',*,*,#16788,.T.);
#23857=ORIENTED_EDGE('',*,*,#16805,.F.);
#23858=ORIENTED_EDGE('',*,*,#16954,.F.);
#23859=ORIENTED_EDGE('',*,*,#16917,.F.);
#23860=ORIENTED_EDGE('',*,*,#16938,.F.);
#23861=ORIENTED_EDGE('',*,*,#16936,.F.);
#23862=ORIENTED_EDGE('',*,*,#16933,.F.);
#23863=ORIENTED_EDGE('',*,*,#16923,.F.);
#23864=ORIENTED_EDGE('',*,*,#16791,.T.);
#23865=ORIENTED_EDGE('',*,*,#16934,.F.);
#23866=ORIENTED_EDGE('',*,*,#16932,.F.);
#23867=ORIENTED_EDGE('',*,*,#16867,.F.);
#23868=ORIENTED_EDGE('',*,*,#16900,.F.);
#23869=ORIENTED_EDGE('',*,*,#16896,.F.);
#23870=ORIENTED_EDGE('',*,*,#16872,.F.);
#23871=ORIENTED_EDGE('',*,*,#16781,.F.);
#23872=ORIENTED_EDGE('',*,*,#16780,.T.);
#23873=ORIENTED_EDGE('',*,*,#16804,.F.);
#23874=ORIENTED_EDGE('',*,*,#16955,.F.);
#23875=ORIENTED_EDGE('',*,*,#16822,.F.);
#23876=ORIENTED_EDGE('',*,*,#16843,.F.);
#23877=ORIENTED_EDGE('',*,*,#16841,.F.);
#23878=ORIENTED_EDGE('',*,*,#16838,.F.);
#23879=ORIENTED_EDGE('',*,*,#16828,.F.);
#23880=ORIENTED_EDGE('',*,*,#16783,.T.);
#23881=ORIENTED_EDGE('',*,*,#16839,.F.);
#23882=ORIENTED_EDGE('',*,*,#16837,.F.);
#23883=ORIENTED_EDGE('',*,*,#16956,.T.);
#23884=ORIENTED_EDGE('',*,*,#16957,.T.);
#23885=ORIENTED_EDGE('',*,*,#16953,.T.);
#23886=ORIENTED_EDGE('',*,*,#16958,.T.);
#23887=ORIENTED_EDGE('',*,*,#16801,.F.);
#23888=ORIENTED_EDGE('',*,*,#16958,.F.);
#23889=ORIENTED_EDGE('',*,*,#16952,.F.);
#23890=ORIENTED_EDGE('',*,*,#16957,.F.);
#23891=ORIENTED_EDGE('',*,*,#16769,.F.);
#23892=ORIENTED_EDGE('',*,*,#16945,.T.);
#23893=ORIENTED_EDGE('',*,*,#16906,.F.);
#23894=ORIENTED_EDGE('',*,*,#16946,.T.);
#23895=ORIENTED_EDGE('',*,*,#16915,.F.);
#23896=ORIENTED_EDGE('',*,*,#16954,.T.);
#23897=ORIENTED_EDGE('',*,*,#16807,.F.);
#23898=ORIENTED_EDGE('',*,*,#16850,.T.);
#23899=ORIENTED_EDGE('',*,*,#16811,.F.);
#23900=ORIENTED_EDGE('',*,*,#16851,.T.);
#23901=ORIENTED_EDGE('',*,*,#16820,.F.);
#23902=ORIENTED_EDGE('',*,*,#16955,.T.);
#23903=ORIENTED_EDGE('',*,*,#16803,.F.);
#23904=ORIENTED_EDGE('',*,*,#16874,.T.);
#23905=ORIENTED_EDGE('',*,*,#16863,.F.);
#23906=ORIENTED_EDGE('',*,*,#16879,.T.);
#23907=ORIENTED_EDGE('',*,*,#16882,.F.);
#23908=ORIENTED_EDGE('',*,*,#16902,.T.);
#23909=ORIENTED_EDGE('',*,*,#16956,.F.);
#23910=ORIENTED_EDGE('',*,*,#16959,.F.);
#23911=ORIENTED_EDGE('',*,*,#16960,.T.);
#23912=ORIENTED_EDGE('',*,*,#16961,.T.);
#23913=ORIENTED_EDGE('',*,*,#16962,.T.);
#23914=ORIENTED_EDGE('',*,*,#16963,.F.);
#23915=ORIENTED_EDGE('',*,*,#16964,.T.);
#23916=ORIENTED_EDGE('',*,*,#16959,.T.);
#23917=ORIENTED_EDGE('',*,*,#16965,.T.);
#23918=ORIENTED_EDGE('',*,*,#16966,.F.);
#23919=ORIENTED_EDGE('',*,*,#16967,.T.);
#23920=ORIENTED_EDGE('',*,*,#16963,.T.);
#23921=ORIENTED_EDGE('',*,*,#16968,.T.);
#23922=ORIENTED_EDGE('',*,*,#16969,.F.);
#23923=ORIENTED_EDGE('',*,*,#16970,.T.);
#23924=ORIENTED_EDGE('',*,*,#16966,.T.);
#23925=ORIENTED_EDGE('',*,*,#16971,.T.);
#23926=ORIENTED_EDGE('',*,*,#16972,.F.);
#23927=ORIENTED_EDGE('',*,*,#16973,.T.);
#23928=ORIENTED_EDGE('',*,*,#16969,.T.);
#23929=ORIENTED_EDGE('',*,*,#16974,.T.);
#23930=ORIENTED_EDGE('',*,*,#16975,.F.);
#23931=ORIENTED_EDGE('',*,*,#16976,.T.);
#23932=ORIENTED_EDGE('',*,*,#16972,.T.);
#23933=ORIENTED_EDGE('',*,*,#16977,.T.);
#23934=ORIENTED_EDGE('',*,*,#16978,.F.);
#23935=ORIENTED_EDGE('',*,*,#16979,.T.);
#23936=ORIENTED_EDGE('',*,*,#16975,.T.);
#23937=ORIENTED_EDGE('',*,*,#16980,.T.);
#23938=ORIENTED_EDGE('',*,*,#16981,.F.);
#23939=ORIENTED_EDGE('',*,*,#16982,.T.);
#23940=ORIENTED_EDGE('',*,*,#16978,.T.);
#23941=ORIENTED_EDGE('',*,*,#16983,.T.);
#23942=ORIENTED_EDGE('',*,*,#16984,.F.);
#23943=ORIENTED_EDGE('',*,*,#16985,.T.);
#23944=ORIENTED_EDGE('',*,*,#16981,.T.);
#23945=ORIENTED_EDGE('',*,*,#16986,.T.);
#23946=ORIENTED_EDGE('',*,*,#16987,.F.);
#23947=ORIENTED_EDGE('',*,*,#16988,.T.);
#23948=ORIENTED_EDGE('',*,*,#16984,.T.);
#23949=ORIENTED_EDGE('',*,*,#16989,.T.);
#23950=ORIENTED_EDGE('',*,*,#16990,.F.);
#23951=ORIENTED_EDGE('',*,*,#16991,.T.);
#23952=ORIENTED_EDGE('',*,*,#16987,.T.);
#23953=ORIENTED_EDGE('',*,*,#16992,.T.);
#23954=ORIENTED_EDGE('',*,*,#16993,.F.);
#23955=ORIENTED_EDGE('',*,*,#16994,.T.);
#23956=ORIENTED_EDGE('',*,*,#16990,.T.);
#23957=ORIENTED_EDGE('',*,*,#16995,.T.);
#23958=ORIENTED_EDGE('',*,*,#16996,.F.);
#23959=ORIENTED_EDGE('',*,*,#16997,.T.);
#23960=ORIENTED_EDGE('',*,*,#16993,.T.);
#23961=ORIENTED_EDGE('',*,*,#16998,.T.);
#23962=ORIENTED_EDGE('',*,*,#16999,.F.);
#23963=ORIENTED_EDGE('',*,*,#17000,.T.);
#23964=ORIENTED_EDGE('',*,*,#16996,.T.);
#23965=ORIENTED_EDGE('',*,*,#17001,.T.);
#23966=ORIENTED_EDGE('',*,*,#17002,.F.);
#23967=ORIENTED_EDGE('',*,*,#17003,.T.);
#23968=ORIENTED_EDGE('',*,*,#16999,.T.);
#23969=ORIENTED_EDGE('',*,*,#17004,.T.);
#23970=ORIENTED_EDGE('',*,*,#17005,.F.);
#23971=ORIENTED_EDGE('',*,*,#17006,.T.);
#23972=ORIENTED_EDGE('',*,*,#17002,.T.);
#23973=ORIENTED_EDGE('',*,*,#17007,.T.);
#23974=ORIENTED_EDGE('',*,*,#17008,.F.);
#23975=ORIENTED_EDGE('',*,*,#17009,.T.);
#23976=ORIENTED_EDGE('',*,*,#17005,.T.);
#23977=ORIENTED_EDGE('',*,*,#17010,.T.);
#23978=ORIENTED_EDGE('',*,*,#17011,.F.);
#23979=ORIENTED_EDGE('',*,*,#17012,.T.);
#23980=ORIENTED_EDGE('',*,*,#17008,.T.);
#23981=ORIENTED_EDGE('',*,*,#17013,.T.);
#23982=ORIENTED_EDGE('',*,*,#17014,.F.);
#23983=ORIENTED_EDGE('',*,*,#17015,.T.);
#23984=ORIENTED_EDGE('',*,*,#17011,.T.);
#23985=ORIENTED_EDGE('',*,*,#17016,.T.);
#23986=ORIENTED_EDGE('',*,*,#17017,.F.);
#23987=ORIENTED_EDGE('',*,*,#17018,.T.);
#23988=ORIENTED_EDGE('',*,*,#17014,.T.);
#23989=ORIENTED_EDGE('',*,*,#17019,.T.);
#23990=ORIENTED_EDGE('',*,*,#17020,.F.);
#23991=ORIENTED_EDGE('',*,*,#17021,.T.);
#23992=ORIENTED_EDGE('',*,*,#17022,.F.);
#23993=ORIENTED_EDGE('',*,*,#17023,.F.);
#23994=ORIENTED_EDGE('',*,*,#17024,.T.);
#23995=ORIENTED_EDGE('',*,*,#17020,.T.);
#23996=ORIENTED_EDGE('',*,*,#17025,.F.);
#23997=ORIENTED_EDGE('',*,*,#17026,.F.);
#23998=ORIENTED_EDGE('',*,*,#17027,.F.);
#23999=ORIENTED_EDGE('',*,*,#17028,.T.);
#24000=ORIENTED_EDGE('',*,*,#17023,.T.);
#24001=ORIENTED_EDGE('',*,*,#17029,.F.);
#24002=ORIENTED_EDGE('',*,*,#17030,.F.);
#24003=ORIENTED_EDGE('',*,*,#17031,.T.);
#24004=ORIENTED_EDGE('',*,*,#17027,.T.);
#24005=ORIENTED_EDGE('',*,*,#17032,.F.);
#24006=ORIENTED_EDGE('',*,*,#17033,.F.);
#24007=ORIENTED_EDGE('',*,*,#17034,.T.);
#24008=ORIENTED_EDGE('',*,*,#17030,.T.);
#24009=ORIENTED_EDGE('',*,*,#17035,.F.);
#24010=ORIENTED_EDGE('',*,*,#17036,.F.);
#24011=ORIENTED_EDGE('',*,*,#17037,.T.);
#24012=ORIENTED_EDGE('',*,*,#17033,.T.);
#24013=ORIENTED_EDGE('',*,*,#17038,.F.);
#24014=ORIENTED_EDGE('',*,*,#17039,.F.);
#24015=ORIENTED_EDGE('',*,*,#17040,.T.);
#24016=ORIENTED_EDGE('',*,*,#17036,.T.);
#24017=ORIENTED_EDGE('',*,*,#17041,.F.);
#24018=ORIENTED_EDGE('',*,*,#17042,.F.);
#24019=ORIENTED_EDGE('',*,*,#17043,.T.);
#24020=ORIENTED_EDGE('',*,*,#17039,.T.);
#24021=ORIENTED_EDGE('',*,*,#17044,.F.);
#24022=ORIENTED_EDGE('',*,*,#17045,.F.);
#24023=ORIENTED_EDGE('',*,*,#17046,.T.);
#24024=ORIENTED_EDGE('',*,*,#17042,.T.);
#24025=ORIENTED_EDGE('',*,*,#17047,.F.);
#24026=ORIENTED_EDGE('',*,*,#17048,.F.);
#24027=ORIENTED_EDGE('',*,*,#17049,.T.);
#24028=ORIENTED_EDGE('',*,*,#17045,.T.);
#24029=ORIENTED_EDGE('',*,*,#17050,.F.);
#24030=ORIENTED_EDGE('',*,*,#17051,.F.);
#24031=ORIENTED_EDGE('',*,*,#17052,.T.);
#24032=ORIENTED_EDGE('',*,*,#17048,.T.);
#24033=ORIENTED_EDGE('',*,*,#17053,.F.);
#24034=ORIENTED_EDGE('',*,*,#17054,.F.);
#24035=ORIENTED_EDGE('',*,*,#17055,.T.);
#24036=ORIENTED_EDGE('',*,*,#17051,.T.);
#24037=ORIENTED_EDGE('',*,*,#17056,.F.);
#24038=ORIENTED_EDGE('',*,*,#17057,.F.);
#24039=ORIENTED_EDGE('',*,*,#17058,.T.);
#24040=ORIENTED_EDGE('',*,*,#17054,.T.);
#24041=ORIENTED_EDGE('',*,*,#17059,.F.);
#24042=ORIENTED_EDGE('',*,*,#17060,.F.);
#24043=ORIENTED_EDGE('',*,*,#17061,.T.);
#24044=ORIENTED_EDGE('',*,*,#17057,.T.);
#24045=ORIENTED_EDGE('',*,*,#17062,.F.);
#24046=ORIENTED_EDGE('',*,*,#17063,.F.);
#24047=ORIENTED_EDGE('',*,*,#17064,.T.);
#24048=ORIENTED_EDGE('',*,*,#17060,.T.);
#24049=ORIENTED_EDGE('',*,*,#17065,.F.);
#24050=ORIENTED_EDGE('',*,*,#17066,.F.);
#24051=ORIENTED_EDGE('',*,*,#17067,.T.);
#24052=ORIENTED_EDGE('',*,*,#17063,.T.);
#24053=ORIENTED_EDGE('',*,*,#17068,.F.);
#24054=ORIENTED_EDGE('',*,*,#17069,.F.);
#24055=ORIENTED_EDGE('',*,*,#17070,.T.);
#24056=ORIENTED_EDGE('',*,*,#17066,.T.);
#24057=ORIENTED_EDGE('',*,*,#17071,.F.);
#24058=ORIENTED_EDGE('',*,*,#17072,.F.);
#24059=ORIENTED_EDGE('',*,*,#17073,.T.);
#24060=ORIENTED_EDGE('',*,*,#17069,.T.);
#24061=ORIENTED_EDGE('',*,*,#17074,.F.);
#24062=ORIENTED_EDGE('',*,*,#17075,.F.);
#24063=ORIENTED_EDGE('',*,*,#17076,.T.);
#24064=ORIENTED_EDGE('',*,*,#17072,.T.);
#24065=ORIENTED_EDGE('',*,*,#17077,.F.);
#24066=ORIENTED_EDGE('',*,*,#17078,.F.);
#24067=ORIENTED_EDGE('',*,*,#17079,.T.);
#24068=ORIENTED_EDGE('',*,*,#17075,.T.);
#24069=ORIENTED_EDGE('',*,*,#17080,.F.);
#24070=ORIENTED_EDGE('',*,*,#17081,.F.);
#24071=ORIENTED_EDGE('',*,*,#17082,.F.);
#24072=ORIENTED_EDGE('',*,*,#17019,.F.);
#24073=ORIENTED_EDGE('',*,*,#17016,.F.);
#24074=ORIENTED_EDGE('',*,*,#17013,.F.);
#24075=ORIENTED_EDGE('',*,*,#17010,.F.);
#24076=ORIENTED_EDGE('',*,*,#17007,.F.);
#24077=ORIENTED_EDGE('',*,*,#17004,.F.);
#24078=ORIENTED_EDGE('',*,*,#17001,.F.);
#24079=ORIENTED_EDGE('',*,*,#16998,.F.);
#24080=ORIENTED_EDGE('',*,*,#16995,.F.);
#24081=ORIENTED_EDGE('',*,*,#16992,.F.);
#24082=ORIENTED_EDGE('',*,*,#16989,.F.);
#24083=ORIENTED_EDGE('',*,*,#16986,.F.);
#24084=ORIENTED_EDGE('',*,*,#16983,.F.);
#24085=ORIENTED_EDGE('',*,*,#16980,.F.);
#24086=ORIENTED_EDGE('',*,*,#16977,.F.);
#24087=ORIENTED_EDGE('',*,*,#16974,.F.);
#24088=ORIENTED_EDGE('',*,*,#16971,.F.);
#24089=ORIENTED_EDGE('',*,*,#16968,.F.);
#24090=ORIENTED_EDGE('',*,*,#16965,.F.);
#24091=ORIENTED_EDGE('',*,*,#16962,.F.);
#24092=ORIENTED_EDGE('',*,*,#17083,.F.);
#24093=ORIENTED_EDGE('',*,*,#17084,.T.);
#24094=ORIENTED_EDGE('',*,*,#17080,.T.);
#24095=ORIENTED_EDGE('',*,*,#17077,.T.);
#24096=ORIENTED_EDGE('',*,*,#17074,.T.);
#24097=ORIENTED_EDGE('',*,*,#17071,.T.);
#24098=ORIENTED_EDGE('',*,*,#17068,.T.);
#24099=ORIENTED_EDGE('',*,*,#17065,.T.);
#24100=ORIENTED_EDGE('',*,*,#17062,.T.);
#24101=ORIENTED_EDGE('',*,*,#17059,.T.);
#24102=ORIENTED_EDGE('',*,*,#17056,.T.);
#24103=ORIENTED_EDGE('',*,*,#17053,.T.);
#24104=ORIENTED_EDGE('',*,*,#17050,.T.);
#24105=ORIENTED_EDGE('',*,*,#17047,.T.);
#24106=ORIENTED_EDGE('',*,*,#17044,.T.);
#24107=ORIENTED_EDGE('',*,*,#17041,.T.);
#24108=ORIENTED_EDGE('',*,*,#17038,.T.);
#24109=ORIENTED_EDGE('',*,*,#17035,.T.);
#24110=ORIENTED_EDGE('',*,*,#17032,.T.);
#24111=ORIENTED_EDGE('',*,*,#17029,.T.);
#24112=ORIENTED_EDGE('',*,*,#17026,.T.);
#24113=ORIENTED_EDGE('',*,*,#17085,.T.);
#24114=ORIENTED_EDGE('',*,*,#17086,.T.);
#24115=ORIENTED_EDGE('',*,*,#17087,.T.);
#24116=ORIENTED_EDGE('',*,*,#17088,.T.);
#24117=ORIENTED_EDGE('',*,*,#17083,.T.);
#24118=ORIENTED_EDGE('',*,*,#17078,.T.);
#24119=ORIENTED_EDGE('',*,*,#17084,.F.);
#24120=ORIENTED_EDGE('',*,*,#17088,.F.);
#24121=ORIENTED_EDGE('',*,*,#17089,.T.);
#24122=ORIENTED_EDGE('',*,*,#17090,.F.);
#24123=ORIENTED_EDGE('',*,*,#17021,.F.);
#24124=ORIENTED_EDGE('',*,*,#17024,.F.);
#24125=ORIENTED_EDGE('',*,*,#17028,.F.);
#24126=ORIENTED_EDGE('',*,*,#17031,.F.);
#24127=ORIENTED_EDGE('',*,*,#17034,.F.);
#24128=ORIENTED_EDGE('',*,*,#17037,.F.);
#24129=ORIENTED_EDGE('',*,*,#17040,.F.);
#24130=ORIENTED_EDGE('',*,*,#17043,.F.);
#24131=ORIENTED_EDGE('',*,*,#17046,.F.);
#24132=ORIENTED_EDGE('',*,*,#17049,.F.);
#24133=ORIENTED_EDGE('',*,*,#17052,.F.);
#24134=ORIENTED_EDGE('',*,*,#17055,.F.);
#24135=ORIENTED_EDGE('',*,*,#17058,.F.);
#24136=ORIENTED_EDGE('',*,*,#17061,.F.);
#24137=ORIENTED_EDGE('',*,*,#17064,.F.);
#24138=ORIENTED_EDGE('',*,*,#17067,.F.);
#24139=ORIENTED_EDGE('',*,*,#17070,.F.);
#24140=ORIENTED_EDGE('',*,*,#17073,.F.);
#24141=ORIENTED_EDGE('',*,*,#17076,.F.);
#24142=ORIENTED_EDGE('',*,*,#17079,.F.);
#24143=ORIENTED_EDGE('',*,*,#17089,.F.);
#24144=ORIENTED_EDGE('',*,*,#17087,.F.);
#24145=ORIENTED_EDGE('',*,*,#16960,.F.);
#24146=ORIENTED_EDGE('',*,*,#16964,.F.);
#24147=ORIENTED_EDGE('',*,*,#16967,.F.);
#24148=ORIENTED_EDGE('',*,*,#16970,.F.);
#24149=ORIENTED_EDGE('',*,*,#16973,.F.);
#24150=ORIENTED_EDGE('',*,*,#16976,.F.);
#24151=ORIENTED_EDGE('',*,*,#16979,.F.);
#24152=ORIENTED_EDGE('',*,*,#16982,.F.);
#24153=ORIENTED_EDGE('',*,*,#16985,.F.);
#24154=ORIENTED_EDGE('',*,*,#16988,.F.);
#24155=ORIENTED_EDGE('',*,*,#16991,.F.);
#24156=ORIENTED_EDGE('',*,*,#16994,.F.);
#24157=ORIENTED_EDGE('',*,*,#16997,.F.);
#24158=ORIENTED_EDGE('',*,*,#17000,.F.);
#24159=ORIENTED_EDGE('',*,*,#17003,.F.);
#24160=ORIENTED_EDGE('',*,*,#17006,.F.);
#24161=ORIENTED_EDGE('',*,*,#17009,.F.);
#24162=ORIENTED_EDGE('',*,*,#17012,.F.);
#24163=ORIENTED_EDGE('',*,*,#17015,.F.);
#24164=ORIENTED_EDGE('',*,*,#17018,.F.);
#24165=ORIENTED_EDGE('',*,*,#17091,.F.);
#24166=ORIENTED_EDGE('',*,*,#17092,.F.);
#24167=ORIENTED_EDGE('',*,*,#17093,.F.);
#24168=ORIENTED_EDGE('',*,*,#17094,.F.);
#24169=ORIENTED_EDGE('',*,*,#17095,.F.);
#24170=ORIENTED_EDGE('',*,*,#17096,.F.);
#24171=ORIENTED_EDGE('',*,*,#17097,.T.);
#24172=ORIENTED_EDGE('',*,*,#17098,.F.);
#24173=ORIENTED_EDGE('',*,*,#17097,.F.);
#24174=ORIENTED_EDGE('',*,*,#17099,.F.);
#24175=ORIENTED_EDGE('',*,*,#17100,.F.);
#24176=ORIENTED_EDGE('',*,*,#17095,.T.);
#24177=ORIENTED_EDGE('',*,*,#17101,.F.);
#24178=ORIENTED_EDGE('',*,*,#17102,.T.);
#24179=ORIENTED_EDGE('',*,*,#17103,.T.);
#24180=ORIENTED_EDGE('',*,*,#17094,.T.);
#24181=ORIENTED_EDGE('',*,*,#17104,.F.);
#24182=ORIENTED_EDGE('',*,*,#17105,.T.);
#24183=ORIENTED_EDGE('',*,*,#17101,.T.);
#24184=ORIENTED_EDGE('',*,*,#17093,.T.);
#24185=ORIENTED_EDGE('',*,*,#17106,.F.);
#24186=ORIENTED_EDGE('',*,*,#17107,.T.);
#24187=ORIENTED_EDGE('',*,*,#17104,.T.);
#24188=ORIENTED_EDGE('',*,*,#17107,.F.);
#24189=ORIENTED_EDGE('',*,*,#17108,.F.);
#24190=ORIENTED_EDGE('',*,*,#17109,.F.);
#24191=ORIENTED_EDGE('',*,*,#17110,.F.);
#24192=ORIENTED_EDGE('',*,*,#17102,.F.);
#24193=ORIENTED_EDGE('',*,*,#17105,.F.);
#24194=ORIENTED_EDGE('',*,*,#17111,.T.);
#24195=ORIENTED_EDGE('',*,*,#17081,.T.);
#24196=ORIENTED_EDGE('',*,*,#17025,.T.);
#24197=ORIENTED_EDGE('',*,*,#17022,.T.);
#24198=ORIENTED_EDGE('',*,*,#17090,.T.);
#24199=ORIENTED_EDGE('',*,*,#17092,.T.);
#24200=ORIENTED_EDGE('',*,*,#17112,.F.);
#24201=ORIENTED_EDGE('',*,*,#17108,.T.);
#24202=ORIENTED_EDGE('',*,*,#17106,.T.);
#24203=ORIENTED_EDGE('',*,*,#17100,.T.);
#24204=ORIENTED_EDGE('',*,*,#17113,.F.);
#24205=ORIENTED_EDGE('',*,*,#17109,.T.);
#24206=ORIENTED_EDGE('',*,*,#17112,.T.);
#24207=ORIENTED_EDGE('',*,*,#17099,.T.);
#24208=ORIENTED_EDGE('',*,*,#17096,.T.);
#24209=ORIENTED_EDGE('',*,*,#17103,.F.);
#24210=ORIENTED_EDGE('',*,*,#17110,.T.);
#24211=ORIENTED_EDGE('',*,*,#17113,.T.);
#24212=ORIENTED_EDGE('',*,*,#17098,.T.);
#24213=ORIENTED_EDGE('',*,*,#17114,.F.);
#24214=ORIENTED_EDGE('',*,*,#17085,.F.);
#24215=ORIENTED_EDGE('',*,*,#16961,.F.);
#24216=ORIENTED_EDGE('',*,*,#17086,.F.);
#24217=ORIENTED_EDGE('',*,*,#17115,.T.);
#24218=ORIENTED_EDGE('',*,*,#17114,.T.);
#24219=ORIENTED_EDGE('',*,*,#17115,.F.);
#24220=ORIENTED_EDGE('',*,*,#17017,.T.);
#24221=ORIENTED_EDGE('',*,*,#17082,.T.);
#24222=ORIENTED_EDGE('',*,*,#17111,.F.);
#24223=ORIENTED_EDGE('',*,*,#17091,.T.);
#24224=ORIENTED_EDGE('',*,*,#17116,.F.);
#24225=ORIENTED_EDGE('',*,*,#17117,.T.);
#24226=ORIENTED_EDGE('',*,*,#17118,.T.);
#24227=ORIENTED_EDGE('',*,*,#17119,.T.);
#24228=ORIENTED_EDGE('',*,*,#17120,.F.);
#24229=ORIENTED_EDGE('',*,*,#17121,.T.);
#24230=ORIENTED_EDGE('',*,*,#17116,.T.);
#24231=ORIENTED_EDGE('',*,*,#17122,.T.);
#24232=ORIENTED_EDGE('',*,*,#17123,.F.);
#24233=ORIENTED_EDGE('',*,*,#17124,.T.);
#24234=ORIENTED_EDGE('',*,*,#17120,.T.);
#24235=ORIENTED_EDGE('',*,*,#17125,.T.);
#24236=ORIENTED_EDGE('',*,*,#17126,.F.);
#24237=ORIENTED_EDGE('',*,*,#17127,.T.);
#24238=ORIENTED_EDGE('',*,*,#17123,.T.);
#24239=ORIENTED_EDGE('',*,*,#17128,.T.);
#24240=ORIENTED_EDGE('',*,*,#17129,.F.);
#24241=ORIENTED_EDGE('',*,*,#17130,.T.);
#24242=ORIENTED_EDGE('',*,*,#17126,.T.);
#24243=ORIENTED_EDGE('',*,*,#17131,.T.);
#24244=ORIENTED_EDGE('',*,*,#17132,.F.);
#24245=ORIENTED_EDGE('',*,*,#17133,.T.);
#24246=ORIENTED_EDGE('',*,*,#17129,.T.);
#24247=ORIENTED_EDGE('',*,*,#17134,.T.);
#24248=ORIENTED_EDGE('',*,*,#17135,.F.);
#24249=ORIENTED_EDGE('',*,*,#17136,.T.);
#24250=ORIENTED_EDGE('',*,*,#17132,.T.);
#24251=ORIENTED_EDGE('',*,*,#17137,.T.);
#24252=ORIENTED_EDGE('',*,*,#17138,.F.);
#24253=ORIENTED_EDGE('',*,*,#17139,.T.);
#24254=ORIENTED_EDGE('',*,*,#17135,.T.);
#24255=ORIENTED_EDGE('',*,*,#17140,.T.);
#24256=ORIENTED_EDGE('',*,*,#17141,.F.);
#24257=ORIENTED_EDGE('',*,*,#17142,.T.);
#24258=ORIENTED_EDGE('',*,*,#17138,.T.);
#24259=ORIENTED_EDGE('',*,*,#17143,.T.);
#24260=ORIENTED_EDGE('',*,*,#17144,.F.);
#24261=ORIENTED_EDGE('',*,*,#17145,.T.);
#24262=ORIENTED_EDGE('',*,*,#17141,.T.);
#24263=ORIENTED_EDGE('',*,*,#17146,.T.);
#24264=ORIENTED_EDGE('',*,*,#17147,.F.);
#24265=ORIENTED_EDGE('',*,*,#17148,.T.);
#24266=ORIENTED_EDGE('',*,*,#17144,.T.);
#24267=ORIENTED_EDGE('',*,*,#17149,.T.);
#24268=ORIENTED_EDGE('',*,*,#17150,.F.);
#24269=ORIENTED_EDGE('',*,*,#17151,.T.);
#24270=ORIENTED_EDGE('',*,*,#17147,.T.);
#24271=ORIENTED_EDGE('',*,*,#17152,.T.);
#24272=ORIENTED_EDGE('',*,*,#17153,.F.);
#24273=ORIENTED_EDGE('',*,*,#17154,.T.);
#24274=ORIENTED_EDGE('',*,*,#17150,.T.);
#24275=ORIENTED_EDGE('',*,*,#17155,.T.);
#24276=ORIENTED_EDGE('',*,*,#17156,.F.);
#24277=ORIENTED_EDGE('',*,*,#17157,.T.);
#24278=ORIENTED_EDGE('',*,*,#17153,.T.);
#24279=ORIENTED_EDGE('',*,*,#17158,.T.);
#24280=ORIENTED_EDGE('',*,*,#17159,.F.);
#24281=ORIENTED_EDGE('',*,*,#17160,.T.);
#24282=ORIENTED_EDGE('',*,*,#17156,.T.);
#24283=ORIENTED_EDGE('',*,*,#17161,.T.);
#24284=ORIENTED_EDGE('',*,*,#17162,.F.);
#24285=ORIENTED_EDGE('',*,*,#17163,.T.);
#24286=ORIENTED_EDGE('',*,*,#17159,.T.);
#24287=ORIENTED_EDGE('',*,*,#17164,.T.);
#24288=ORIENTED_EDGE('',*,*,#17165,.F.);
#24289=ORIENTED_EDGE('',*,*,#17166,.T.);
#24290=ORIENTED_EDGE('',*,*,#17162,.T.);
#24291=ORIENTED_EDGE('',*,*,#17167,.T.);
#24292=ORIENTED_EDGE('',*,*,#17168,.F.);
#24293=ORIENTED_EDGE('',*,*,#17169,.T.);
#24294=ORIENTED_EDGE('',*,*,#17165,.T.);
#24295=ORIENTED_EDGE('',*,*,#17170,.T.);
#24296=ORIENTED_EDGE('',*,*,#17171,.F.);
#24297=ORIENTED_EDGE('',*,*,#17172,.T.);
#24298=ORIENTED_EDGE('',*,*,#17168,.T.);
#24299=ORIENTED_EDGE('',*,*,#17173,.T.);
#24300=ORIENTED_EDGE('',*,*,#17174,.F.);
#24301=ORIENTED_EDGE('',*,*,#17175,.T.);
#24302=ORIENTED_EDGE('',*,*,#17171,.T.);
#24303=ORIENTED_EDGE('',*,*,#17176,.T.);
#24304=ORIENTED_EDGE('',*,*,#17177,.F.);
#24305=ORIENTED_EDGE('',*,*,#17178,.T.);
#24306=ORIENTED_EDGE('',*,*,#17179,.F.);
#24307=ORIENTED_EDGE('',*,*,#17180,.F.);
#24308=ORIENTED_EDGE('',*,*,#17181,.T.);
#24309=ORIENTED_EDGE('',*,*,#17177,.T.);
#24310=ORIENTED_EDGE('',*,*,#17182,.F.);
#24311=ORIENTED_EDGE('',*,*,#17183,.F.);
#24312=ORIENTED_EDGE('',*,*,#17184,.F.);
#24313=ORIENTED_EDGE('',*,*,#17185,.T.);
#24314=ORIENTED_EDGE('',*,*,#17180,.T.);
#24315=ORIENTED_EDGE('',*,*,#17186,.F.);
#24316=ORIENTED_EDGE('',*,*,#17187,.F.);
#24317=ORIENTED_EDGE('',*,*,#17188,.T.);
#24318=ORIENTED_EDGE('',*,*,#17184,.T.);
#24319=ORIENTED_EDGE('',*,*,#17189,.F.);
#24320=ORIENTED_EDGE('',*,*,#17190,.F.);
#24321=ORIENTED_EDGE('',*,*,#17191,.T.);
#24322=ORIENTED_EDGE('',*,*,#17187,.T.);
#24323=ORIENTED_EDGE('',*,*,#17192,.F.);
#24324=ORIENTED_EDGE('',*,*,#17193,.F.);
#24325=ORIENTED_EDGE('',*,*,#17194,.T.);
#24326=ORIENTED_EDGE('',*,*,#17190,.T.);
#24327=ORIENTED_EDGE('',*,*,#17195,.F.);
#24328=ORIENTED_EDGE('',*,*,#17196,.F.);
#24329=ORIENTED_EDGE('',*,*,#17197,.T.);
#24330=ORIENTED_EDGE('',*,*,#17193,.T.);
#24331=ORIENTED_EDGE('',*,*,#17198,.F.);
#24332=ORIENTED_EDGE('',*,*,#17199,.F.);
#24333=ORIENTED_EDGE('',*,*,#17200,.T.);
#24334=ORIENTED_EDGE('',*,*,#17196,.T.);
#24335=ORIENTED_EDGE('',*,*,#17201,.F.);
#24336=ORIENTED_EDGE('',*,*,#17202,.F.);
#24337=ORIENTED_EDGE('',*,*,#17203,.T.);
#24338=ORIENTED_EDGE('',*,*,#17199,.T.);
#24339=ORIENTED_EDGE('',*,*,#17204,.F.);
#24340=ORIENTED_EDGE('',*,*,#17205,.F.);
#24341=ORIENTED_EDGE('',*,*,#17206,.T.);
#24342=ORIENTED_EDGE('',*,*,#17202,.T.);
#24343=ORIENTED_EDGE('',*,*,#17207,.F.);
#24344=ORIENTED_EDGE('',*,*,#17208,.F.);
#24345=ORIENTED_EDGE('',*,*,#17209,.T.);
#24346=ORIENTED_EDGE('',*,*,#17205,.T.);
#24347=ORIENTED_EDGE('',*,*,#17210,.F.);
#24348=ORIENTED_EDGE('',*,*,#17211,.F.);
#24349=ORIENTED_EDGE('',*,*,#17212,.T.);
#24350=ORIENTED_EDGE('',*,*,#17208,.T.);
#24351=ORIENTED_EDGE('',*,*,#17213,.F.);
#24352=ORIENTED_EDGE('',*,*,#17214,.F.);
#24353=ORIENTED_EDGE('',*,*,#17215,.T.);
#24354=ORIENTED_EDGE('',*,*,#17211,.T.);
#24355=ORIENTED_EDGE('',*,*,#17216,.F.);
#24356=ORIENTED_EDGE('',*,*,#17217,.F.);
#24357=ORIENTED_EDGE('',*,*,#17218,.T.);
#24358=ORIENTED_EDGE('',*,*,#17214,.T.);
#24359=ORIENTED_EDGE('',*,*,#17219,.F.);
#24360=ORIENTED_EDGE('',*,*,#17220,.F.);
#24361=ORIENTED_EDGE('',*,*,#17221,.T.);
#24362=ORIENTED_EDGE('',*,*,#17217,.T.);
#24363=ORIENTED_EDGE('',*,*,#17222,.F.);
#24364=ORIENTED_EDGE('',*,*,#17223,.F.);
#24365=ORIENTED_EDGE('',*,*,#17224,.T.);
#24366=ORIENTED_EDGE('',*,*,#17220,.T.);
#24367=ORIENTED_EDGE('',*,*,#17225,.F.);
#24368=ORIENTED_EDGE('',*,*,#17226,.F.);
#24369=ORIENTED_EDGE('',*,*,#17227,.T.);
#24370=ORIENTED_EDGE('',*,*,#17223,.T.);
#24371=ORIENTED_EDGE('',*,*,#17228,.F.);
#24372=ORIENTED_EDGE('',*,*,#17229,.F.);
#24373=ORIENTED_EDGE('',*,*,#17230,.T.);
#24374=ORIENTED_EDGE('',*,*,#17226,.T.);
#24375=ORIENTED_EDGE('',*,*,#17231,.F.);
#24376=ORIENTED_EDGE('',*,*,#17232,.F.);
#24377=ORIENTED_EDGE('',*,*,#17233,.T.);
#24378=ORIENTED_EDGE('',*,*,#17229,.T.);
#24379=ORIENTED_EDGE('',*,*,#17234,.F.);
#24380=ORIENTED_EDGE('',*,*,#17235,.F.);
#24381=ORIENTED_EDGE('',*,*,#17236,.T.);
#24382=ORIENTED_EDGE('',*,*,#17232,.T.);
#24383=ORIENTED_EDGE('',*,*,#17237,.F.);
#24384=ORIENTED_EDGE('',*,*,#17238,.F.);
#24385=ORIENTED_EDGE('',*,*,#17239,.F.);
#24386=ORIENTED_EDGE('',*,*,#17176,.F.);
#24387=ORIENTED_EDGE('',*,*,#17173,.F.);
#24388=ORIENTED_EDGE('',*,*,#17170,.F.);
#24389=ORIENTED_EDGE('',*,*,#17167,.F.);
#24390=ORIENTED_EDGE('',*,*,#17164,.F.);
#24391=ORIENTED_EDGE('',*,*,#17161,.F.);
#24392=ORIENTED_EDGE('',*,*,#17158,.F.);
#24393=ORIENTED_EDGE('',*,*,#17155,.F.);
#24394=ORIENTED_EDGE('',*,*,#17152,.F.);
#24395=ORIENTED_EDGE('',*,*,#17149,.F.);
#24396=ORIENTED_EDGE('',*,*,#17146,.F.);
#24397=ORIENTED_EDGE('',*,*,#17143,.F.);
#24398=ORIENTED_EDGE('',*,*,#17140,.F.);
#24399=ORIENTED_EDGE('',*,*,#17137,.F.);
#24400=ORIENTED_EDGE('',*,*,#17134,.F.);
#24401=ORIENTED_EDGE('',*,*,#17131,.F.);
#24402=ORIENTED_EDGE('',*,*,#17128,.F.);
#24403=ORIENTED_EDGE('',*,*,#17125,.F.);
#24404=ORIENTED_EDGE('',*,*,#17122,.F.);
#24405=ORIENTED_EDGE('',*,*,#17119,.F.);
#24406=ORIENTED_EDGE('',*,*,#17240,.F.);
#24407=ORIENTED_EDGE('',*,*,#17241,.T.);
#24408=ORIENTED_EDGE('',*,*,#17237,.T.);
#24409=ORIENTED_EDGE('',*,*,#17234,.T.);
#24410=ORIENTED_EDGE('',*,*,#17231,.T.);
#24411=ORIENTED_EDGE('',*,*,#17228,.T.);
#24412=ORIENTED_EDGE('',*,*,#17225,.T.);
#24413=ORIENTED_EDGE('',*,*,#17222,.T.);
#24414=ORIENTED_EDGE('',*,*,#17219,.T.);
#24415=ORIENTED_EDGE('',*,*,#17216,.T.);
#24416=ORIENTED_EDGE('',*,*,#17213,.T.);
#24417=ORIENTED_EDGE('',*,*,#17210,.T.);
#24418=ORIENTED_EDGE('',*,*,#17207,.T.);
#24419=ORIENTED_EDGE('',*,*,#17204,.T.);
#24420=ORIENTED_EDGE('',*,*,#17201,.T.);
#24421=ORIENTED_EDGE('',*,*,#17198,.T.);
#24422=ORIENTED_EDGE('',*,*,#17195,.T.);
#24423=ORIENTED_EDGE('',*,*,#17192,.T.);
#24424=ORIENTED_EDGE('',*,*,#17189,.T.);
#24425=ORIENTED_EDGE('',*,*,#17186,.T.);
#24426=ORIENTED_EDGE('',*,*,#17183,.T.);
#24427=ORIENTED_EDGE('',*,*,#17242,.T.);
#24428=ORIENTED_EDGE('',*,*,#17243,.T.);
#24429=ORIENTED_EDGE('',*,*,#17244,.T.);
#24430=ORIENTED_EDGE('',*,*,#17245,.T.);
#24431=ORIENTED_EDGE('',*,*,#17240,.T.);
#24432=ORIENTED_EDGE('',*,*,#17235,.T.);
#24433=ORIENTED_EDGE('',*,*,#17241,.F.);
#24434=ORIENTED_EDGE('',*,*,#17245,.F.);
#24435=ORIENTED_EDGE('',*,*,#17246,.T.);
#24436=ORIENTED_EDGE('',*,*,#17247,.F.);
#24437=ORIENTED_EDGE('',*,*,#17178,.F.);
#24438=ORIENTED_EDGE('',*,*,#17181,.F.);
#24439=ORIENTED_EDGE('',*,*,#17185,.F.);
#24440=ORIENTED_EDGE('',*,*,#17188,.F.);
#24441=ORIENTED_EDGE('',*,*,#17191,.F.);
#24442=ORIENTED_EDGE('',*,*,#17194,.F.);
#24443=ORIENTED_EDGE('',*,*,#17197,.F.);
#24444=ORIENTED_EDGE('',*,*,#17200,.F.);
#24445=ORIENTED_EDGE('',*,*,#17203,.F.);
#24446=ORIENTED_EDGE('',*,*,#17206,.F.);
#24447=ORIENTED_EDGE('',*,*,#17209,.F.);
#24448=ORIENTED_EDGE('',*,*,#17212,.F.);
#24449=ORIENTED_EDGE('',*,*,#17215,.F.);
#24450=ORIENTED_EDGE('',*,*,#17218,.F.);
#24451=ORIENTED_EDGE('',*,*,#17221,.F.);
#24452=ORIENTED_EDGE('',*,*,#17224,.F.);
#24453=ORIENTED_EDGE('',*,*,#17227,.F.);
#24454=ORIENTED_EDGE('',*,*,#17230,.F.);
#24455=ORIENTED_EDGE('',*,*,#17233,.F.);
#24456=ORIENTED_EDGE('',*,*,#17236,.F.);
#24457=ORIENTED_EDGE('',*,*,#17246,.F.);
#24458=ORIENTED_EDGE('',*,*,#17244,.F.);
#24459=ORIENTED_EDGE('',*,*,#17117,.F.);
#24460=ORIENTED_EDGE('',*,*,#17121,.F.);
#24461=ORIENTED_EDGE('',*,*,#17124,.F.);
#24462=ORIENTED_EDGE('',*,*,#17127,.F.);
#24463=ORIENTED_EDGE('',*,*,#17130,.F.);
#24464=ORIENTED_EDGE('',*,*,#17133,.F.);
#24465=ORIENTED_EDGE('',*,*,#17136,.F.);
#24466=ORIENTED_EDGE('',*,*,#17139,.F.);
#24467=ORIENTED_EDGE('',*,*,#17142,.F.);
#24468=ORIENTED_EDGE('',*,*,#17145,.F.);
#24469=ORIENTED_EDGE('',*,*,#17148,.F.);
#24470=ORIENTED_EDGE('',*,*,#17151,.F.);
#24471=ORIENTED_EDGE('',*,*,#17154,.F.);
#24472=ORIENTED_EDGE('',*,*,#17157,.F.);
#24473=ORIENTED_EDGE('',*,*,#17160,.F.);
#24474=ORIENTED_EDGE('',*,*,#17163,.F.);
#24475=ORIENTED_EDGE('',*,*,#17166,.F.);
#24476=ORIENTED_EDGE('',*,*,#17169,.F.);
#24477=ORIENTED_EDGE('',*,*,#17172,.F.);
#24478=ORIENTED_EDGE('',*,*,#17175,.F.);
#24479=ORIENTED_EDGE('',*,*,#17248,.F.);
#24480=ORIENTED_EDGE('',*,*,#17249,.F.);
#24481=ORIENTED_EDGE('',*,*,#17250,.T.);
#24482=ORIENTED_EDGE('',*,*,#17251,.F.);
#24483=ORIENTED_EDGE('',*,*,#17252,.F.);
#24484=ORIENTED_EDGE('',*,*,#17253,.F.);
#24485=ORIENTED_EDGE('',*,*,#17252,.T.);
#24486=ORIENTED_EDGE('',*,*,#17254,.T.);
#24487=ORIENTED_EDGE('',*,*,#17255,.F.);
#24488=ORIENTED_EDGE('',*,*,#17254,.F.);
#24489=ORIENTED_EDGE('',*,*,#17251,.T.);
#24490=ORIENTED_EDGE('',*,*,#17256,.T.);
#24491=ORIENTED_EDGE('',*,*,#17257,.F.);
#24492=ORIENTED_EDGE('',*,*,#17256,.F.);
#24493=ORIENTED_EDGE('',*,*,#17250,.F.);
#24494=ORIENTED_EDGE('',*,*,#17258,.F.);
#24495=ORIENTED_EDGE('',*,*,#17259,.T.);
#24496=ORIENTED_EDGE('',*,*,#17260,.F.);
#24497=ORIENTED_EDGE('',*,*,#17261,.F.);
#24498=ORIENTED_EDGE('',*,*,#17262,.F.);
#24499=ORIENTED_EDGE('',*,*,#17261,.T.);
#24500=ORIENTED_EDGE('',*,*,#17263,.T.);
#24501=ORIENTED_EDGE('',*,*,#17264,.F.);
#24502=ORIENTED_EDGE('',*,*,#17263,.F.);
#24503=ORIENTED_EDGE('',*,*,#17260,.T.);
#24504=ORIENTED_EDGE('',*,*,#17265,.T.);
#24505=ORIENTED_EDGE('',*,*,#17266,.F.);
#24506=ORIENTED_EDGE('',*,*,#17265,.F.);
#24507=ORIENTED_EDGE('',*,*,#17259,.F.);
#24508=ORIENTED_EDGE('',*,*,#17267,.F.);
#24509=ORIENTED_EDGE('',*,*,#17268,.T.);
#24510=ORIENTED_EDGE('',*,*,#17269,.F.);
#24511=ORIENTED_EDGE('',*,*,#17270,.F.);
#24512=ORIENTED_EDGE('',*,*,#17271,.F.);
#24513=ORIENTED_EDGE('',*,*,#17270,.T.);
#24514=ORIENTED_EDGE('',*,*,#17272,.T.);
#24515=ORIENTED_EDGE('',*,*,#17273,.F.);
#24516=ORIENTED_EDGE('',*,*,#17272,.F.);
#24517=ORIENTED_EDGE('',*,*,#17269,.T.);
#24518=ORIENTED_EDGE('',*,*,#17274,.T.);
#24519=ORIENTED_EDGE('',*,*,#17275,.F.);
#24520=ORIENTED_EDGE('',*,*,#17274,.F.);
#24521=ORIENTED_EDGE('',*,*,#17268,.F.);
#24522=ORIENTED_EDGE('',*,*,#17276,.F.);
#24523=ORIENTED_EDGE('',*,*,#17277,.T.);
#24524=ORIENTED_EDGE('',*,*,#17278,.F.);
#24525=ORIENTED_EDGE('',*,*,#17279,.F.);
#24526=ORIENTED_EDGE('',*,*,#17280,.F.);
#24527=ORIENTED_EDGE('',*,*,#17279,.T.);
#24528=ORIENTED_EDGE('',*,*,#17281,.T.);
#24529=ORIENTED_EDGE('',*,*,#17282,.F.);
#24530=ORIENTED_EDGE('',*,*,#17281,.F.);
#24531=ORIENTED_EDGE('',*,*,#17278,.T.);
#24532=ORIENTED_EDGE('',*,*,#17283,.T.);
#24533=ORIENTED_EDGE('',*,*,#17284,.F.);
#24534=ORIENTED_EDGE('',*,*,#17283,.F.);
#24535=ORIENTED_EDGE('',*,*,#17277,.F.);
#24536=ORIENTED_EDGE('',*,*,#17285,.F.);
#24537=ORIENTED_EDGE('',*,*,#17286,.T.);
#24538=ORIENTED_EDGE('',*,*,#17287,.F.);
#24539=ORIENTED_EDGE('',*,*,#17288,.F.);
#24540=ORIENTED_EDGE('',*,*,#17289,.F.);
#24541=ORIENTED_EDGE('',*,*,#17288,.T.);
#24542=ORIENTED_EDGE('',*,*,#17290,.T.);
#24543=ORIENTED_EDGE('',*,*,#17291,.F.);
#24544=ORIENTED_EDGE('',*,*,#17290,.F.);
#24545=ORIENTED_EDGE('',*,*,#17287,.T.);
#24546=ORIENTED_EDGE('',*,*,#17292,.T.);
#24547=ORIENTED_EDGE('',*,*,#17293,.F.);
#24548=ORIENTED_EDGE('',*,*,#17292,.F.);
#24549=ORIENTED_EDGE('',*,*,#17286,.F.);
#24550=ORIENTED_EDGE('',*,*,#17294,.F.);
#24551=ORIENTED_EDGE('',*,*,#17295,.T.);
#24552=ORIENTED_EDGE('',*,*,#17296,.F.);
#24553=ORIENTED_EDGE('',*,*,#17297,.F.);
#24554=ORIENTED_EDGE('',*,*,#17298,.F.);
#24555=ORIENTED_EDGE('',*,*,#17297,.T.);
#24556=ORIENTED_EDGE('',*,*,#17299,.T.);
#24557=ORIENTED_EDGE('',*,*,#17300,.F.);
#24558=ORIENTED_EDGE('',*,*,#17299,.F.);
#24559=ORIENTED_EDGE('',*,*,#17296,.T.);
#24560=ORIENTED_EDGE('',*,*,#17301,.T.);
#24561=ORIENTED_EDGE('',*,*,#17302,.F.);
#24562=ORIENTED_EDGE('',*,*,#17301,.F.);
#24563=ORIENTED_EDGE('',*,*,#17295,.F.);
#24564=ORIENTED_EDGE('',*,*,#17303,.F.);
#24565=ORIENTED_EDGE('',*,*,#17304,.T.);
#24566=ORIENTED_EDGE('',*,*,#17305,.F.);
#24567=ORIENTED_EDGE('',*,*,#17306,.F.);
#24568=ORIENTED_EDGE('',*,*,#17307,.F.);
#24569=ORIENTED_EDGE('',*,*,#17306,.T.);
#24570=ORIENTED_EDGE('',*,*,#17308,.T.);
#24571=ORIENTED_EDGE('',*,*,#17309,.F.);
#24572=ORIENTED_EDGE('',*,*,#17308,.F.);
#24573=ORIENTED_EDGE('',*,*,#17305,.T.);
#24574=ORIENTED_EDGE('',*,*,#17310,.T.);
#24575=ORIENTED_EDGE('',*,*,#17311,.F.);
#24576=ORIENTED_EDGE('',*,*,#17310,.F.);
#24577=ORIENTED_EDGE('',*,*,#17304,.F.);
#24578=ORIENTED_EDGE('',*,*,#17312,.F.);
#24579=ORIENTED_EDGE('',*,*,#17313,.T.);
#24580=ORIENTED_EDGE('',*,*,#17314,.F.);
#24581=ORIENTED_EDGE('',*,*,#17315,.F.);
#24582=ORIENTED_EDGE('',*,*,#17316,.F.);
#24583=ORIENTED_EDGE('',*,*,#17315,.T.);
#24584=ORIENTED_EDGE('',*,*,#17317,.T.);
#24585=ORIENTED_EDGE('',*,*,#17318,.F.);
#24586=ORIENTED_EDGE('',*,*,#17317,.F.);
#24587=ORIENTED_EDGE('',*,*,#17314,.T.);
#24588=ORIENTED_EDGE('',*,*,#17319,.T.);
#24589=ORIENTED_EDGE('',*,*,#17320,.F.);
#24590=ORIENTED_EDGE('',*,*,#17319,.F.);
#24591=ORIENTED_EDGE('',*,*,#17313,.F.);
#24592=ORIENTED_EDGE('',*,*,#17321,.F.);
#24593=ORIENTED_EDGE('',*,*,#17322,.T.);
#24594=ORIENTED_EDGE('',*,*,#17323,.F.);
#24595=ORIENTED_EDGE('',*,*,#17324,.F.);
#24596=ORIENTED_EDGE('',*,*,#17325,.F.);
#24597=ORIENTED_EDGE('',*,*,#17324,.T.);
#24598=ORIENTED_EDGE('',*,*,#17326,.T.);
#24599=ORIENTED_EDGE('',*,*,#17327,.F.);
#24600=ORIENTED_EDGE('',*,*,#17326,.F.);
#24601=ORIENTED_EDGE('',*,*,#17323,.T.);
#24602=ORIENTED_EDGE('',*,*,#17328,.T.);
#24603=ORIENTED_EDGE('',*,*,#17329,.F.);
#24604=ORIENTED_EDGE('',*,*,#17328,.F.);
#24605=ORIENTED_EDGE('',*,*,#17322,.F.);
#24606=ORIENTED_EDGE('',*,*,#17330,.F.);
#24607=ORIENTED_EDGE('',*,*,#17331,.T.);
#24608=ORIENTED_EDGE('',*,*,#17332,.F.);
#24609=ORIENTED_EDGE('',*,*,#17333,.F.);
#24610=ORIENTED_EDGE('',*,*,#17334,.F.);
#24611=ORIENTED_EDGE('',*,*,#17333,.T.);
#24612=ORIENTED_EDGE('',*,*,#17335,.T.);
#24613=ORIENTED_EDGE('',*,*,#17336,.F.);
#24614=ORIENTED_EDGE('',*,*,#17335,.F.);
#24615=ORIENTED_EDGE('',*,*,#17332,.T.);
#24616=ORIENTED_EDGE('',*,*,#17337,.T.);
#24617=ORIENTED_EDGE('',*,*,#17338,.F.);
#24618=ORIENTED_EDGE('',*,*,#17337,.F.);
#24619=ORIENTED_EDGE('',*,*,#17331,.F.);
#24620=ORIENTED_EDGE('',*,*,#17339,.F.);
#24621=ORIENTED_EDGE('',*,*,#17340,.T.);
#24622=ORIENTED_EDGE('',*,*,#17341,.F.);
#24623=ORIENTED_EDGE('',*,*,#17342,.F.);
#24624=ORIENTED_EDGE('',*,*,#17343,.F.);
#24625=ORIENTED_EDGE('',*,*,#17342,.T.);
#24626=ORIENTED_EDGE('',*,*,#17344,.T.);
#24627=ORIENTED_EDGE('',*,*,#17345,.F.);
#24628=ORIENTED_EDGE('',*,*,#17344,.F.);
#24629=ORIENTED_EDGE('',*,*,#17341,.T.);
#24630=ORIENTED_EDGE('',*,*,#17346,.T.);
#24631=ORIENTED_EDGE('',*,*,#17347,.F.);
#24632=ORIENTED_EDGE('',*,*,#17346,.F.);
#24633=ORIENTED_EDGE('',*,*,#17340,.F.);
#24634=ORIENTED_EDGE('',*,*,#17348,.F.);
#24635=ORIENTED_EDGE('',*,*,#17349,.T.);
#24636=ORIENTED_EDGE('',*,*,#17350,.F.);
#24637=ORIENTED_EDGE('',*,*,#17351,.F.);
#24638=ORIENTED_EDGE('',*,*,#17352,.F.);
#24639=ORIENTED_EDGE('',*,*,#17351,.T.);
#24640=ORIENTED_EDGE('',*,*,#17353,.T.);
#24641=ORIENTED_EDGE('',*,*,#17354,.F.);
#24642=ORIENTED_EDGE('',*,*,#17353,.F.);
#24643=ORIENTED_EDGE('',*,*,#17350,.T.);
#24644=ORIENTED_EDGE('',*,*,#17355,.T.);
#24645=ORIENTED_EDGE('',*,*,#17356,.F.);
#24646=ORIENTED_EDGE('',*,*,#17355,.F.);
#24647=ORIENTED_EDGE('',*,*,#17349,.F.);
#24648=ORIENTED_EDGE('',*,*,#17357,.F.);
#24649=ORIENTED_EDGE('',*,*,#17358,.T.);
#24650=ORIENTED_EDGE('',*,*,#17359,.F.);
#24651=ORIENTED_EDGE('',*,*,#17360,.F.);
#24652=ORIENTED_EDGE('',*,*,#17361,.F.);
#24653=ORIENTED_EDGE('',*,*,#17360,.T.);
#24654=ORIENTED_EDGE('',*,*,#17362,.T.);
#24655=ORIENTED_EDGE('',*,*,#17363,.F.);
#24656=ORIENTED_EDGE('',*,*,#17362,.F.);
#24657=ORIENTED_EDGE('',*,*,#17359,.T.);
#24658=ORIENTED_EDGE('',*,*,#17364,.T.);
#24659=ORIENTED_EDGE('',*,*,#17365,.F.);
#24660=ORIENTED_EDGE('',*,*,#17364,.F.);
#24661=ORIENTED_EDGE('',*,*,#17358,.F.);
#24662=ORIENTED_EDGE('',*,*,#17366,.F.);
#24663=ORIENTED_EDGE('',*,*,#17367,.T.);
#24664=ORIENTED_EDGE('',*,*,#17368,.F.);
#24665=ORIENTED_EDGE('',*,*,#17369,.F.);
#24666=ORIENTED_EDGE('',*,*,#17370,.F.);
#24667=ORIENTED_EDGE('',*,*,#17369,.T.);
#24668=ORIENTED_EDGE('',*,*,#17371,.T.);
#24669=ORIENTED_EDGE('',*,*,#17372,.F.);
#24670=ORIENTED_EDGE('',*,*,#17371,.F.);
#24671=ORIENTED_EDGE('',*,*,#17368,.T.);
#24672=ORIENTED_EDGE('',*,*,#17373,.T.);
#24673=ORIENTED_EDGE('',*,*,#17374,.F.);
#24674=ORIENTED_EDGE('',*,*,#17373,.F.);
#24675=ORIENTED_EDGE('',*,*,#17367,.F.);
#24676=ORIENTED_EDGE('',*,*,#17375,.F.);
#24677=ORIENTED_EDGE('',*,*,#17376,.T.);
#24678=ORIENTED_EDGE('',*,*,#17377,.F.);
#24679=ORIENTED_EDGE('',*,*,#17378,.F.);
#24680=ORIENTED_EDGE('',*,*,#17379,.F.);
#24681=ORIENTED_EDGE('',*,*,#17378,.T.);
#24682=ORIENTED_EDGE('',*,*,#17380,.T.);
#24683=ORIENTED_EDGE('',*,*,#17381,.F.);
#24684=ORIENTED_EDGE('',*,*,#17380,.F.);
#24685=ORIENTED_EDGE('',*,*,#17377,.T.);
#24686=ORIENTED_EDGE('',*,*,#17382,.T.);
#24687=ORIENTED_EDGE('',*,*,#17383,.F.);
#24688=ORIENTED_EDGE('',*,*,#17382,.F.);
#24689=ORIENTED_EDGE('',*,*,#17376,.F.);
#24690=ORIENTED_EDGE('',*,*,#17384,.F.);
#24691=ORIENTED_EDGE('',*,*,#17385,.T.);
#24692=ORIENTED_EDGE('',*,*,#17386,.F.);
#24693=ORIENTED_EDGE('',*,*,#17387,.F.);
#24694=ORIENTED_EDGE('',*,*,#17388,.F.);
#24695=ORIENTED_EDGE('',*,*,#17387,.T.);
#24696=ORIENTED_EDGE('',*,*,#17389,.T.);
#24697=ORIENTED_EDGE('',*,*,#17390,.F.);
#24698=ORIENTED_EDGE('',*,*,#17389,.F.);
#24699=ORIENTED_EDGE('',*,*,#17386,.T.);
#24700=ORIENTED_EDGE('',*,*,#17391,.T.);
#24701=ORIENTED_EDGE('',*,*,#17392,.F.);
#24702=ORIENTED_EDGE('',*,*,#17391,.F.);
#24703=ORIENTED_EDGE('',*,*,#17385,.F.);
#24704=ORIENTED_EDGE('',*,*,#17393,.F.);
#24705=ORIENTED_EDGE('',*,*,#17394,.T.);
#24706=ORIENTED_EDGE('',*,*,#17395,.F.);
#24707=ORIENTED_EDGE('',*,*,#17396,.F.);
#24708=ORIENTED_EDGE('',*,*,#17397,.F.);
#24709=ORIENTED_EDGE('',*,*,#17396,.T.);
#24710=ORIENTED_EDGE('',*,*,#17398,.T.);
#24711=ORIENTED_EDGE('',*,*,#17399,.F.);
#24712=ORIENTED_EDGE('',*,*,#17398,.F.);
#24713=ORIENTED_EDGE('',*,*,#17395,.T.);
#24714=ORIENTED_EDGE('',*,*,#17400,.T.);
#24715=ORIENTED_EDGE('',*,*,#17401,.F.);
#24716=ORIENTED_EDGE('',*,*,#17400,.F.);
#24717=ORIENTED_EDGE('',*,*,#17394,.F.);
#24718=ORIENTED_EDGE('',*,*,#17402,.F.);
#24719=ORIENTED_EDGE('',*,*,#17403,.T.);
#24720=ORIENTED_EDGE('',*,*,#17404,.F.);
#24721=ORIENTED_EDGE('',*,*,#17405,.F.);
#24722=ORIENTED_EDGE('',*,*,#17406,.F.);
#24723=ORIENTED_EDGE('',*,*,#17405,.T.);
#24724=ORIENTED_EDGE('',*,*,#17407,.T.);
#24725=ORIENTED_EDGE('',*,*,#17408,.F.);
#24726=ORIENTED_EDGE('',*,*,#17409,.F.);
#24727=ORIENTED_EDGE('',*,*,#17407,.F.);
#24728=ORIENTED_EDGE('',*,*,#17404,.T.);
#24729=ORIENTED_EDGE('',*,*,#17410,.T.);
#24730=ORIENTED_EDGE('',*,*,#17411,.F.);
#24731=ORIENTED_EDGE('',*,*,#17410,.F.);
#24732=ORIENTED_EDGE('',*,*,#17403,.F.);
#24733=ORIENTED_EDGE('',*,*,#17412,.F.);
#24734=ORIENTED_EDGE('',*,*,#17413,.F.);
#24735=ORIENTED_EDGE('',*,*,#17414,.T.);
#24736=ORIENTED_EDGE('',*,*,#17415,.F.);
#24737=ORIENTED_EDGE('',*,*,#17416,.F.);
#24738=ORIENTED_EDGE('',*,*,#17417,.F.);
#24739=ORIENTED_EDGE('',*,*,#17416,.T.);
#24740=ORIENTED_EDGE('',*,*,#17418,.T.);
#24741=ORIENTED_EDGE('',*,*,#17419,.F.);
#24742=ORIENTED_EDGE('',*,*,#17418,.F.);
#24743=ORIENTED_EDGE('',*,*,#17415,.T.);
#24744=ORIENTED_EDGE('',*,*,#17420,.T.);
#24745=ORIENTED_EDGE('',*,*,#17421,.F.);
#24746=ORIENTED_EDGE('',*,*,#17420,.F.);
#24747=ORIENTED_EDGE('',*,*,#17414,.F.);
#24748=ORIENTED_EDGE('',*,*,#17422,.F.);
#24749=ORIENTED_EDGE('',*,*,#17423,.T.);
#24750=ORIENTED_EDGE('',*,*,#17424,.F.);
#24751=ORIENTED_EDGE('',*,*,#17425,.F.);
#24752=ORIENTED_EDGE('',*,*,#17426,.F.);
#24753=ORIENTED_EDGE('',*,*,#17425,.T.);
#24754=ORIENTED_EDGE('',*,*,#17427,.T.);
#24755=ORIENTED_EDGE('',*,*,#17428,.F.);
#24756=ORIENTED_EDGE('',*,*,#17427,.F.);
#24757=ORIENTED_EDGE('',*,*,#17424,.T.);
#24758=ORIENTED_EDGE('',*,*,#17429,.T.);
#24759=ORIENTED_EDGE('',*,*,#17430,.F.);
#24760=ORIENTED_EDGE('',*,*,#17429,.F.);
#24761=ORIENTED_EDGE('',*,*,#17423,.F.);
#24762=ORIENTED_EDGE('',*,*,#17431,.F.);
#24763=ORIENTED_EDGE('',*,*,#17432,.T.);
#24764=ORIENTED_EDGE('',*,*,#17433,.F.);
#24765=ORIENTED_EDGE('',*,*,#17434,.F.);
#24766=ORIENTED_EDGE('',*,*,#17435,.F.);
#24767=ORIENTED_EDGE('',*,*,#17434,.T.);
#24768=ORIENTED_EDGE('',*,*,#17436,.T.);
#24769=ORIENTED_EDGE('',*,*,#17437,.F.);
#24770=ORIENTED_EDGE('',*,*,#17436,.F.);
#24771=ORIENTED_EDGE('',*,*,#17433,.T.);
#24772=ORIENTED_EDGE('',*,*,#17438,.T.);
#24773=ORIENTED_EDGE('',*,*,#17439,.F.);
#24774=ORIENTED_EDGE('',*,*,#17438,.F.);
#24775=ORIENTED_EDGE('',*,*,#17432,.F.);
#24776=ORIENTED_EDGE('',*,*,#17440,.F.);
#24777=ORIENTED_EDGE('',*,*,#17441,.T.);
#24778=ORIENTED_EDGE('',*,*,#17442,.F.);
#24779=ORIENTED_EDGE('',*,*,#17443,.F.);
#24780=ORIENTED_EDGE('',*,*,#17444,.F.);
#24781=ORIENTED_EDGE('',*,*,#17443,.T.);
#24782=ORIENTED_EDGE('',*,*,#17445,.T.);
#24783=ORIENTED_EDGE('',*,*,#17446,.F.);
#24784=ORIENTED_EDGE('',*,*,#17445,.F.);
#24785=ORIENTED_EDGE('',*,*,#17442,.T.);
#24786=ORIENTED_EDGE('',*,*,#17447,.T.);
#24787=ORIENTED_EDGE('',*,*,#17448,.F.);
#24788=ORIENTED_EDGE('',*,*,#17447,.F.);
#24789=ORIENTED_EDGE('',*,*,#17441,.F.);
#24790=ORIENTED_EDGE('',*,*,#17449,.F.);
#24791=ORIENTED_EDGE('',*,*,#17450,.T.);
#24792=ORIENTED_EDGE('',*,*,#17451,.F.);
#24793=ORIENTED_EDGE('',*,*,#17452,.F.);
#24794=ORIENTED_EDGE('',*,*,#17453,.F.);
#24795=ORIENTED_EDGE('',*,*,#17452,.T.);
#24796=ORIENTED_EDGE('',*,*,#17454,.T.);
#24797=ORIENTED_EDGE('',*,*,#17455,.F.);
#24798=ORIENTED_EDGE('',*,*,#17454,.F.);
#24799=ORIENTED_EDGE('',*,*,#17451,.T.);
#24800=ORIENTED_EDGE('',*,*,#17456,.T.);
#24801=ORIENTED_EDGE('',*,*,#17457,.F.);
#24802=ORIENTED_EDGE('',*,*,#17456,.F.);
#24803=ORIENTED_EDGE('',*,*,#17450,.F.);
#24804=ORIENTED_EDGE('',*,*,#17458,.F.);
#24805=ORIENTED_EDGE('',*,*,#17459,.T.);
#24806=ORIENTED_EDGE('',*,*,#17460,.F.);
#24807=ORIENTED_EDGE('',*,*,#17461,.F.);
#24808=ORIENTED_EDGE('',*,*,#17462,.F.);
#24809=ORIENTED_EDGE('',*,*,#17461,.T.);
#24810=ORIENTED_EDGE('',*,*,#17463,.T.);
#24811=ORIENTED_EDGE('',*,*,#17464,.F.);
#24812=ORIENTED_EDGE('',*,*,#17463,.F.);
#24813=ORIENTED_EDGE('',*,*,#17460,.T.);
#24814=ORIENTED_EDGE('',*,*,#17465,.T.);
#24815=ORIENTED_EDGE('',*,*,#17466,.F.);
#24816=ORIENTED_EDGE('',*,*,#17465,.F.);
#24817=ORIENTED_EDGE('',*,*,#17459,.F.);
#24818=ORIENTED_EDGE('',*,*,#17467,.F.);
#24819=ORIENTED_EDGE('',*,*,#17468,.T.);
#24820=ORIENTED_EDGE('',*,*,#17469,.F.);
#24821=ORIENTED_EDGE('',*,*,#17470,.F.);
#24822=ORIENTED_EDGE('',*,*,#17471,.F.);
#24823=ORIENTED_EDGE('',*,*,#17470,.T.);
#24824=ORIENTED_EDGE('',*,*,#17472,.T.);
#24825=ORIENTED_EDGE('',*,*,#17473,.F.);
#24826=ORIENTED_EDGE('',*,*,#17472,.F.);
#24827=ORIENTED_EDGE('',*,*,#17469,.T.);
#24828=ORIENTED_EDGE('',*,*,#17474,.T.);
#24829=ORIENTED_EDGE('',*,*,#17475,.F.);
#24830=ORIENTED_EDGE('',*,*,#17474,.F.);
#24831=ORIENTED_EDGE('',*,*,#17468,.F.);
#24832=ORIENTED_EDGE('',*,*,#17476,.F.);
#24833=ORIENTED_EDGE('',*,*,#17477,.T.);
#24834=ORIENTED_EDGE('',*,*,#17478,.F.);
#24835=ORIENTED_EDGE('',*,*,#17479,.F.);
#24836=ORIENTED_EDGE('',*,*,#17480,.F.);
#24837=ORIENTED_EDGE('',*,*,#17479,.T.);
#24838=ORIENTED_EDGE('',*,*,#17481,.T.);
#24839=ORIENTED_EDGE('',*,*,#17482,.F.);
#24840=ORIENTED_EDGE('',*,*,#17481,.F.);
#24841=ORIENTED_EDGE('',*,*,#17478,.T.);
#24842=ORIENTED_EDGE('',*,*,#17483,.T.);
#24843=ORIENTED_EDGE('',*,*,#17484,.F.);
#24844=ORIENTED_EDGE('',*,*,#17483,.F.);
#24845=ORIENTED_EDGE('',*,*,#17477,.F.);
#24846=ORIENTED_EDGE('',*,*,#17485,.F.);
#24847=ORIENTED_EDGE('',*,*,#17486,.T.);
#24848=ORIENTED_EDGE('',*,*,#17487,.F.);
#24849=ORIENTED_EDGE('',*,*,#17488,.F.);
#24850=ORIENTED_EDGE('',*,*,#17489,.F.);
#24851=ORIENTED_EDGE('',*,*,#17488,.T.);
#24852=ORIENTED_EDGE('',*,*,#17490,.T.);
#24853=ORIENTED_EDGE('',*,*,#17491,.F.);
#24854=ORIENTED_EDGE('',*,*,#17490,.F.);
#24855=ORIENTED_EDGE('',*,*,#17487,.T.);
#24856=ORIENTED_EDGE('',*,*,#17492,.T.);
#24857=ORIENTED_EDGE('',*,*,#17493,.F.);
#24858=ORIENTED_EDGE('',*,*,#17492,.F.);
#24859=ORIENTED_EDGE('',*,*,#17486,.F.);
#24860=ORIENTED_EDGE('',*,*,#17494,.F.);
#24861=ORIENTED_EDGE('',*,*,#17495,.T.);
#24862=ORIENTED_EDGE('',*,*,#17496,.F.);
#24863=ORIENTED_EDGE('',*,*,#17497,.F.);
#24864=ORIENTED_EDGE('',*,*,#17498,.F.);
#24865=ORIENTED_EDGE('',*,*,#17497,.T.);
#24866=ORIENTED_EDGE('',*,*,#17499,.T.);
#24867=ORIENTED_EDGE('',*,*,#17500,.F.);
#24868=ORIENTED_EDGE('',*,*,#17499,.F.);
#24869=ORIENTED_EDGE('',*,*,#17496,.T.);
#24870=ORIENTED_EDGE('',*,*,#17501,.T.);
#24871=ORIENTED_EDGE('',*,*,#17502,.F.);
#24872=ORIENTED_EDGE('',*,*,#17501,.F.);
#24873=ORIENTED_EDGE('',*,*,#17495,.F.);
#24874=ORIENTED_EDGE('',*,*,#17503,.F.);
#24875=ORIENTED_EDGE('',*,*,#17504,.T.);
#24876=ORIENTED_EDGE('',*,*,#17505,.F.);
#24877=ORIENTED_EDGE('',*,*,#17506,.F.);
#24878=ORIENTED_EDGE('',*,*,#17507,.F.);
#24879=ORIENTED_EDGE('',*,*,#17506,.T.);
#24880=ORIENTED_EDGE('',*,*,#17508,.T.);
#24881=ORIENTED_EDGE('',*,*,#17509,.F.);
#24882=ORIENTED_EDGE('',*,*,#17508,.F.);
#24883=ORIENTED_EDGE('',*,*,#17505,.T.);
#24884=ORIENTED_EDGE('',*,*,#17510,.T.);
#24885=ORIENTED_EDGE('',*,*,#17511,.F.);
#24886=ORIENTED_EDGE('',*,*,#17510,.F.);
#24887=ORIENTED_EDGE('',*,*,#17504,.F.);
#24888=ORIENTED_EDGE('',*,*,#17512,.F.);
#24889=ORIENTED_EDGE('',*,*,#17513,.T.);
#24890=ORIENTED_EDGE('',*,*,#17514,.F.);
#24891=ORIENTED_EDGE('',*,*,#17515,.F.);
#24892=ORIENTED_EDGE('',*,*,#17516,.F.);
#24893=ORIENTED_EDGE('',*,*,#17515,.T.);
#24894=ORIENTED_EDGE('',*,*,#17517,.T.);
#24895=ORIENTED_EDGE('',*,*,#17518,.F.);
#24896=ORIENTED_EDGE('',*,*,#17517,.F.);
#24897=ORIENTED_EDGE('',*,*,#17514,.T.);
#24898=ORIENTED_EDGE('',*,*,#17519,.T.);
#24899=ORIENTED_EDGE('',*,*,#17520,.F.);
#24900=ORIENTED_EDGE('',*,*,#17519,.F.);
#24901=ORIENTED_EDGE('',*,*,#17513,.F.);
#24902=ORIENTED_EDGE('',*,*,#17521,.F.);
#24903=ORIENTED_EDGE('',*,*,#17522,.T.);
#24904=ORIENTED_EDGE('',*,*,#17523,.F.);
#24905=ORIENTED_EDGE('',*,*,#17524,.F.);
#24906=ORIENTED_EDGE('',*,*,#17525,.F.);
#24907=ORIENTED_EDGE('',*,*,#17524,.T.);
#24908=ORIENTED_EDGE('',*,*,#17526,.T.);
#24909=ORIENTED_EDGE('',*,*,#17527,.F.);
#24910=ORIENTED_EDGE('',*,*,#17526,.F.);
#24911=ORIENTED_EDGE('',*,*,#17523,.T.);
#24912=ORIENTED_EDGE('',*,*,#17528,.T.);
#24913=ORIENTED_EDGE('',*,*,#17529,.F.);
#24914=ORIENTED_EDGE('',*,*,#17528,.F.);
#24915=ORIENTED_EDGE('',*,*,#17522,.F.);
#24916=ORIENTED_EDGE('',*,*,#17530,.F.);
#24917=ORIENTED_EDGE('',*,*,#17531,.T.);
#24918=ORIENTED_EDGE('',*,*,#17532,.F.);
#24919=ORIENTED_EDGE('',*,*,#17533,.F.);
#24920=ORIENTED_EDGE('',*,*,#17534,.F.);
#24921=ORIENTED_EDGE('',*,*,#17533,.T.);
#24922=ORIENTED_EDGE('',*,*,#17535,.T.);
#24923=ORIENTED_EDGE('',*,*,#17536,.F.);
#24924=ORIENTED_EDGE('',*,*,#17535,.F.);
#24925=ORIENTED_EDGE('',*,*,#17532,.T.);
#24926=ORIENTED_EDGE('',*,*,#17537,.T.);
#24927=ORIENTED_EDGE('',*,*,#17538,.F.);
#24928=ORIENTED_EDGE('',*,*,#17537,.F.);
#24929=ORIENTED_EDGE('',*,*,#17531,.F.);
#24930=ORIENTED_EDGE('',*,*,#17539,.F.);
#24931=ORIENTED_EDGE('',*,*,#17540,.T.);
#24932=ORIENTED_EDGE('',*,*,#17541,.F.);
#24933=ORIENTED_EDGE('',*,*,#17542,.F.);
#24934=ORIENTED_EDGE('',*,*,#17543,.F.);
#24935=ORIENTED_EDGE('',*,*,#17542,.T.);
#24936=ORIENTED_EDGE('',*,*,#17544,.T.);
#24937=ORIENTED_EDGE('',*,*,#17545,.F.);
#24938=ORIENTED_EDGE('',*,*,#17544,.F.);
#24939=ORIENTED_EDGE('',*,*,#17541,.T.);
#24940=ORIENTED_EDGE('',*,*,#17546,.T.);
#24941=ORIENTED_EDGE('',*,*,#17547,.F.);
#24942=ORIENTED_EDGE('',*,*,#17546,.F.);
#24943=ORIENTED_EDGE('',*,*,#17540,.F.);
#24944=ORIENTED_EDGE('',*,*,#17548,.F.);
#24945=ORIENTED_EDGE('',*,*,#17549,.T.);
#24946=ORIENTED_EDGE('',*,*,#17550,.F.);
#24947=ORIENTED_EDGE('',*,*,#17551,.F.);
#24948=ORIENTED_EDGE('',*,*,#17552,.F.);
#24949=ORIENTED_EDGE('',*,*,#17551,.T.);
#24950=ORIENTED_EDGE('',*,*,#17553,.T.);
#24951=ORIENTED_EDGE('',*,*,#17554,.F.);
#24952=ORIENTED_EDGE('',*,*,#17553,.F.);
#24953=ORIENTED_EDGE('',*,*,#17550,.T.);
#24954=ORIENTED_EDGE('',*,*,#17555,.T.);
#24955=ORIENTED_EDGE('',*,*,#17556,.F.);
#24956=ORIENTED_EDGE('',*,*,#17555,.F.);
#24957=ORIENTED_EDGE('',*,*,#17549,.F.);
#24958=ORIENTED_EDGE('',*,*,#17557,.F.);
#24959=ORIENTED_EDGE('',*,*,#17558,.T.);
#24960=ORIENTED_EDGE('',*,*,#17559,.F.);
#24961=ORIENTED_EDGE('',*,*,#17560,.F.);
#24962=ORIENTED_EDGE('',*,*,#17561,.F.);
#24963=ORIENTED_EDGE('',*,*,#17560,.T.);
#24964=ORIENTED_EDGE('',*,*,#17562,.T.);
#24965=ORIENTED_EDGE('',*,*,#17563,.F.);
#24966=ORIENTED_EDGE('',*,*,#17562,.F.);
#24967=ORIENTED_EDGE('',*,*,#17559,.T.);
#24968=ORIENTED_EDGE('',*,*,#17564,.T.);
#24969=ORIENTED_EDGE('',*,*,#17565,.F.);
#24970=ORIENTED_EDGE('',*,*,#17564,.F.);
#24971=ORIENTED_EDGE('',*,*,#17558,.F.);
#24972=ORIENTED_EDGE('',*,*,#17566,.F.);
#24973=ORIENTED_EDGE('',*,*,#17567,.T.);
#24974=ORIENTED_EDGE('',*,*,#17568,.F.);
#24975=ORIENTED_EDGE('',*,*,#17569,.F.);
#24976=ORIENTED_EDGE('',*,*,#17570,.F.);
#24977=ORIENTED_EDGE('',*,*,#17569,.T.);
#24978=ORIENTED_EDGE('',*,*,#17571,.T.);
#24979=ORIENTED_EDGE('',*,*,#17572,.F.);
#24980=ORIENTED_EDGE('',*,*,#17571,.F.);
#24981=ORIENTED_EDGE('',*,*,#17568,.T.);
#24982=ORIENTED_EDGE('',*,*,#17573,.T.);
#24983=ORIENTED_EDGE('',*,*,#17574,.F.);
#24984=ORIENTED_EDGE('',*,*,#17573,.F.);
#24985=ORIENTED_EDGE('',*,*,#17567,.F.);
#24986=ORIENTED_EDGE('',*,*,#17575,.F.);
#24987=ORIENTED_EDGE('',*,*,#17576,.T.);
#24988=ORIENTED_EDGE('',*,*,#17577,.T.);
#24989=ORIENTED_EDGE('',*,*,#17578,.F.);
#24990=ORIENTED_EDGE('',*,*,#17579,.F.);
#24991=ORIENTED_EDGE('',*,*,#17580,.T.);
#24992=ORIENTED_EDGE('',*,*,#17581,.T.);
#24993=ORIENTED_EDGE('',*,*,#17576,.F.);
#24994=ORIENTED_EDGE('',*,*,#17582,.F.);
#24995=ORIENTED_EDGE('',*,*,#17583,.T.);
#24996=ORIENTED_EDGE('',*,*,#17584,.T.);
#24997=ORIENTED_EDGE('',*,*,#17580,.F.);
#24998=ORIENTED_EDGE('',*,*,#17585,.F.);
#24999=ORIENTED_EDGE('',*,*,#17586,.T.);
#25000=ORIENTED_EDGE('',*,*,#17587,.T.);
#25001=ORIENTED_EDGE('',*,*,#17583,.F.);
#25002=ORIENTED_EDGE('',*,*,#17588,.F.);
#25003=ORIENTED_EDGE('',*,*,#17589,.T.);
#25004=ORIENTED_EDGE('',*,*,#17590,.T.);
#25005=ORIENTED_EDGE('',*,*,#17586,.F.);
#25006=ORIENTED_EDGE('',*,*,#17591,.F.);
#25007=ORIENTED_EDGE('',*,*,#17578,.T.);
#25008=ORIENTED_EDGE('',*,*,#17592,.T.);
#25009=ORIENTED_EDGE('',*,*,#17589,.F.);
#25010=ORIENTED_EDGE('',*,*,#17592,.F.);
#25011=ORIENTED_EDGE('',*,*,#17577,.F.);
#25012=ORIENTED_EDGE('',*,*,#17581,.F.);
#25013=ORIENTED_EDGE('',*,*,#17584,.F.);
#25014=ORIENTED_EDGE('',*,*,#17587,.F.);
#25015=ORIENTED_EDGE('',*,*,#17590,.F.);
#25016=ORIENTED_EDGE('',*,*,#17593,.F.);
#25017=ORIENTED_EDGE('',*,*,#17242,.F.);
#25018=ORIENTED_EDGE('',*,*,#17118,.F.);
#25019=ORIENTED_EDGE('',*,*,#17243,.F.);
#25020=ORIENTED_EDGE('',*,*,#17594,.T.);
#25021=ORIENTED_EDGE('',*,*,#17593,.T.);
#25022=ORIENTED_EDGE('',*,*,#17594,.F.);
#25023=ORIENTED_EDGE('',*,*,#17174,.T.);
#25024=ORIENTED_EDGE('',*,*,#17239,.T.);
#25025=ORIENTED_EDGE('',*,*,#17595,.F.);
#25026=ORIENTED_EDGE('',*,*,#17248,.T.);
#25027=ORIENTED_EDGE('',*,*,#17596,.F.);
#25028=ORIENTED_EDGE('',*,*,#17595,.T.);
#25029=ORIENTED_EDGE('',*,*,#17238,.T.);
#25030=ORIENTED_EDGE('',*,*,#17182,.T.);
#25031=ORIENTED_EDGE('',*,*,#17179,.T.);
#25032=ORIENTED_EDGE('',*,*,#17247,.T.);
#25033=ORIENTED_EDGE('',*,*,#17597,.F.);
#25034=ORIENTED_EDGE('',*,*,#17598,.T.);
#25035=ORIENTED_EDGE('',*,*,#17412,.T.);
#25036=ORIENTED_EDGE('',*,*,#17402,.T.);
#25037=ORIENTED_EDGE('',*,*,#17406,.T.);
#25038=ORIENTED_EDGE('',*,*,#17599,.T.);
#25039=ORIENTED_EDGE('',*,*,#17596,.T.);
#25040=ORIENTED_EDGE('',*,*,#17599,.F.);
#25041=ORIENTED_EDGE('',*,*,#17408,.T.);
#25042=ORIENTED_EDGE('',*,*,#17409,.T.);
#25043=ORIENTED_EDGE('',*,*,#17411,.T.);
#25044=ORIENTED_EDGE('',*,*,#17598,.F.);
#25045=ORIENTED_EDGE('',*,*,#17255,.T.);
#25046=ORIENTED_EDGE('',*,*,#17257,.T.);
#25047=ORIENTED_EDGE('',*,*,#17249,.T.);
#25048=ORIENTED_EDGE('',*,*,#17253,.T.);
#25049=ORIENTED_EDGE('',*,*,#17264,.T.);
#25050=ORIENTED_EDGE('',*,*,#17266,.T.);
#25051=ORIENTED_EDGE('',*,*,#17258,.T.);
#25052=ORIENTED_EDGE('',*,*,#17262,.T.);
#25053=ORIENTED_EDGE('',*,*,#17273,.T.);
#25054=ORIENTED_EDGE('',*,*,#17275,.T.);
#25055=ORIENTED_EDGE('',*,*,#17267,.T.);
#25056=ORIENTED_EDGE('',*,*,#17271,.T.);
#25057=ORIENTED_EDGE('',*,*,#17282,.T.);
#25058=ORIENTED_EDGE('',*,*,#17284,.T.);
#25059=ORIENTED_EDGE('',*,*,#17276,.T.);
#25060=ORIENTED_EDGE('',*,*,#17280,.T.);
#25061=ORIENTED_EDGE('',*,*,#17291,.T.);
#25062=ORIENTED_EDGE('',*,*,#17293,.T.);
#25063=ORIENTED_EDGE('',*,*,#17285,.T.);
#25064=ORIENTED_EDGE('',*,*,#17289,.T.);
#25065=ORIENTED_EDGE('',*,*,#17300,.T.);
#25066=ORIENTED_EDGE('',*,*,#17302,.T.);
#25067=ORIENTED_EDGE('',*,*,#17294,.T.);
#25068=ORIENTED_EDGE('',*,*,#17298,.T.);
#25069=ORIENTED_EDGE('',*,*,#17309,.T.);
#25070=ORIENTED_EDGE('',*,*,#17311,.T.);
#25071=ORIENTED_EDGE('',*,*,#17303,.T.);
#25072=ORIENTED_EDGE('',*,*,#17307,.T.);
#25073=ORIENTED_EDGE('',*,*,#17318,.T.);
#25074=ORIENTED_EDGE('',*,*,#17320,.T.);
#25075=ORIENTED_EDGE('',*,*,#17312,.T.);
#25076=ORIENTED_EDGE('',*,*,#17316,.T.);
#25077=ORIENTED_EDGE('',*,*,#17327,.T.);
#25078=ORIENTED_EDGE('',*,*,#17329,.T.);
#25079=ORIENTED_EDGE('',*,*,#17321,.T.);
#25080=ORIENTED_EDGE('',*,*,#17325,.T.);
#25081=ORIENTED_EDGE('',*,*,#17336,.T.);
#25082=ORIENTED_EDGE('',*,*,#17338,.T.);
#25083=ORIENTED_EDGE('',*,*,#17330,.T.);
#25084=ORIENTED_EDGE('',*,*,#17334,.T.);
#25085=ORIENTED_EDGE('',*,*,#17345,.T.);
#25086=ORIENTED_EDGE('',*,*,#17347,.T.);
#25087=ORIENTED_EDGE('',*,*,#17339,.T.);
#25088=ORIENTED_EDGE('',*,*,#17343,.T.);
#25089=ORIENTED_EDGE('',*,*,#17354,.T.);
#25090=ORIENTED_EDGE('',*,*,#17356,.T.);
#25091=ORIENTED_EDGE('',*,*,#17348,.T.);
#25092=ORIENTED_EDGE('',*,*,#17352,.T.);
#25093=ORIENTED_EDGE('',*,*,#17363,.T.);
#25094=ORIENTED_EDGE('',*,*,#17365,.T.);
#25095=ORIENTED_EDGE('',*,*,#17357,.T.);
#25096=ORIENTED_EDGE('',*,*,#17361,.T.);
#25097=ORIENTED_EDGE('',*,*,#17372,.T.);
#25098=ORIENTED_EDGE('',*,*,#17374,.T.);
#25099=ORIENTED_EDGE('',*,*,#17366,.T.);
#25100=ORIENTED_EDGE('',*,*,#17370,.T.);
#25101=ORIENTED_EDGE('',*,*,#17381,.T.);
#25102=ORIENTED_EDGE('',*,*,#17383,.T.);
#25103=ORIENTED_EDGE('',*,*,#17375,.T.);
#25104=ORIENTED_EDGE('',*,*,#17379,.T.);
#25105=ORIENTED_EDGE('',*,*,#17390,.T.);
#25106=ORIENTED_EDGE('',*,*,#17392,.T.);
#25107=ORIENTED_EDGE('',*,*,#17384,.T.);
#25108=ORIENTED_EDGE('',*,*,#17388,.T.);
#25109=ORIENTED_EDGE('',*,*,#17399,.T.);
#25110=ORIENTED_EDGE('',*,*,#17401,.T.);
#25111=ORIENTED_EDGE('',*,*,#17393,.T.);
#25112=ORIENTED_EDGE('',*,*,#17397,.T.);
#25113=ORIENTED_EDGE('',*,*,#17419,.T.);
#25114=ORIENTED_EDGE('',*,*,#17421,.T.);
#25115=ORIENTED_EDGE('',*,*,#17413,.T.);
#25116=ORIENTED_EDGE('',*,*,#17417,.T.);
#25117=ORIENTED_EDGE('',*,*,#17428,.T.);
#25118=ORIENTED_EDGE('',*,*,#17430,.T.);
#25119=ORIENTED_EDGE('',*,*,#17422,.T.);
#25120=ORIENTED_EDGE('',*,*,#17426,.T.);
#25121=ORIENTED_EDGE('',*,*,#17437,.T.);
#25122=ORIENTED_EDGE('',*,*,#17439,.T.);
#25123=ORIENTED_EDGE('',*,*,#17431,.T.);
#25124=ORIENTED_EDGE('',*,*,#17435,.T.);
#25125=ORIENTED_EDGE('',*,*,#17446,.T.);
#25126=ORIENTED_EDGE('',*,*,#17448,.T.);
#25127=ORIENTED_EDGE('',*,*,#17440,.T.);
#25128=ORIENTED_EDGE('',*,*,#17444,.T.);
#25129=ORIENTED_EDGE('',*,*,#17455,.T.);
#25130=ORIENTED_EDGE('',*,*,#17457,.T.);
#25131=ORIENTED_EDGE('',*,*,#17449,.T.);
#25132=ORIENTED_EDGE('',*,*,#17453,.T.);
#25133=ORIENTED_EDGE('',*,*,#17464,.T.);
#25134=ORIENTED_EDGE('',*,*,#17466,.T.);
#25135=ORIENTED_EDGE('',*,*,#17458,.T.);
#25136=ORIENTED_EDGE('',*,*,#17462,.T.);
#25137=ORIENTED_EDGE('',*,*,#17473,.T.);
#25138=ORIENTED_EDGE('',*,*,#17475,.T.);
#25139=ORIENTED_EDGE('',*,*,#17467,.T.);
#25140=ORIENTED_EDGE('',*,*,#17471,.T.);
#25141=ORIENTED_EDGE('',*,*,#17482,.T.);
#25142=ORIENTED_EDGE('',*,*,#17484,.T.);
#25143=ORIENTED_EDGE('',*,*,#17476,.T.);
#25144=ORIENTED_EDGE('',*,*,#17480,.T.);
#25145=ORIENTED_EDGE('',*,*,#17491,.T.);
#25146=ORIENTED_EDGE('',*,*,#17493,.T.);
#25147=ORIENTED_EDGE('',*,*,#17485,.T.);
#25148=ORIENTED_EDGE('',*,*,#17489,.T.);
#25149=ORIENTED_EDGE('',*,*,#17500,.T.);
#25150=ORIENTED_EDGE('',*,*,#17502,.T.);
#25151=ORIENTED_EDGE('',*,*,#17494,.T.);
#25152=ORIENTED_EDGE('',*,*,#17498,.T.);
#25153=ORIENTED_EDGE('',*,*,#17509,.T.);
#25154=ORIENTED_EDGE('',*,*,#17511,.T.);
#25155=ORIENTED_EDGE('',*,*,#17503,.T.);
#25156=ORIENTED_EDGE('',*,*,#17507,.T.);
#25157=ORIENTED_EDGE('',*,*,#17518,.T.);
#25158=ORIENTED_EDGE('',*,*,#17520,.T.);
#25159=ORIENTED_EDGE('',*,*,#17512,.T.);
#25160=ORIENTED_EDGE('',*,*,#17516,.T.);
#25161=ORIENTED_EDGE('',*,*,#17527,.T.);
#25162=ORIENTED_EDGE('',*,*,#17529,.T.);
#25163=ORIENTED_EDGE('',*,*,#17521,.T.);
#25164=ORIENTED_EDGE('',*,*,#17525,.T.);
#25165=ORIENTED_EDGE('',*,*,#17536,.T.);
#25166=ORIENTED_EDGE('',*,*,#17538,.T.);
#25167=ORIENTED_EDGE('',*,*,#17530,.T.);
#25168=ORIENTED_EDGE('',*,*,#17534,.T.);
#25169=ORIENTED_EDGE('',*,*,#17545,.T.);
#25170=ORIENTED_EDGE('',*,*,#17547,.T.);
#25171=ORIENTED_EDGE('',*,*,#17539,.T.);
#25172=ORIENTED_EDGE('',*,*,#17543,.T.);
#25173=ORIENTED_EDGE('',*,*,#17554,.T.);
#25174=ORIENTED_EDGE('',*,*,#17556,.T.);
#25175=ORIENTED_EDGE('',*,*,#17548,.T.);
#25176=ORIENTED_EDGE('',*,*,#17552,.T.);
#25177=ORIENTED_EDGE('',*,*,#17563,.T.);
#25178=ORIENTED_EDGE('',*,*,#17565,.T.);
#25179=ORIENTED_EDGE('',*,*,#17557,.T.);
#25180=ORIENTED_EDGE('',*,*,#17561,.T.);
#25181=ORIENTED_EDGE('',*,*,#17572,.T.);
#25182=ORIENTED_EDGE('',*,*,#17574,.T.);
#25183=ORIENTED_EDGE('',*,*,#17566,.T.);
#25184=ORIENTED_EDGE('',*,*,#17570,.T.);
#25185=ORIENTED_EDGE('',*,*,#17600,.F.);
#25186=ORIENTED_EDGE('',*,*,#17601,.T.);
#25187=ORIENTED_EDGE('',*,*,#17597,.T.);
#25188=ORIENTED_EDGE('',*,*,#17601,.F.);
#25189=ORIENTED_EDGE('',*,*,#17600,.T.);
#25190=ORIENTED_EDGE('',*,*,#17575,.T.);
#25191=ORIENTED_EDGE('',*,*,#17591,.T.);
#25192=ORIENTED_EDGE('',*,*,#17588,.T.);
#25193=ORIENTED_EDGE('',*,*,#17585,.T.);
#25194=ORIENTED_EDGE('',*,*,#17582,.T.);
#25195=ORIENTED_EDGE('',*,*,#17579,.T.);
#25196=ORIENTED_EDGE('',*,*,#17602,.F.);
#25197=ORIENTED_EDGE('',*,*,#17603,.F.);
#25198=ORIENTED_EDGE('',*,*,#17604,.F.);
#25199=ORIENTED_EDGE('',*,*,#17605,.T.);
#25200=ORIENTED_EDGE('',*,*,#17606,.T.);
#25201=ORIENTED_EDGE('',*,*,#17603,.T.);
#25202=ORIENTED_EDGE('',*,*,#17607,.T.);
#25203=ORIENTED_EDGE('',*,*,#17608,.F.);
#25204=ORIENTED_EDGE('',*,*,#17609,.F.);
#25205=ORIENTED_EDGE('',*,*,#17610,.F.);
#25206=ORIENTED_EDGE('',*,*,#17611,.T.);
#25207=ORIENTED_EDGE('',*,*,#17612,.T.);
#25208=ORIENTED_EDGE('',*,*,#17609,.T.);
#25209=ORIENTED_EDGE('',*,*,#17613,.T.);
#25210=ORIENTED_EDGE('',*,*,#17602,.T.);
#25211=ORIENTED_EDGE('',*,*,#17614,.T.);
#25212=ORIENTED_EDGE('',*,*,#17610,.T.);
#25213=ORIENTED_EDGE('',*,*,#17615,.T.);
#25214=ORIENTED_EDGE('',*,*,#17616,.F.);
#25215=ORIENTED_EDGE('',*,*,#17617,.F.);
#25216=ORIENTED_EDGE('',*,*,#17618,.F.);
#25217=ORIENTED_EDGE('',*,*,#17619,.T.);
#25218=ORIENTED_EDGE('',*,*,#17620,.T.);
#25219=ORIENTED_EDGE('',*,*,#17617,.T.);
#25220=ORIENTED_EDGE('',*,*,#17621,.T.);
#25221=ORIENTED_EDGE('',*,*,#17622,.F.);
#25222=ORIENTED_EDGE('',*,*,#17623,.F.);
#25223=ORIENTED_EDGE('',*,*,#17624,.F.);
#25224=ORIENTED_EDGE('',*,*,#17625,.T.);
#25225=ORIENTED_EDGE('',*,*,#17626,.T.);
#25226=ORIENTED_EDGE('',*,*,#17623,.T.);
#25227=ORIENTED_EDGE('',*,*,#17627,.T.);
#25228=ORIENTED_EDGE('',*,*,#17608,.T.);
#25229=ORIENTED_EDGE('',*,*,#17628,.T.);
#25230=ORIENTED_EDGE('',*,*,#17624,.T.);
#25231=ORIENTED_EDGE('',*,*,#17629,.T.);
#25232=ORIENTED_EDGE('',*,*,#17630,.F.);
#25233=ORIENTED_EDGE('',*,*,#17631,.F.);
#25234=ORIENTED_EDGE('',*,*,#17632,.F.);
#25235=ORIENTED_EDGE('',*,*,#17633,.T.);
#25236=ORIENTED_EDGE('',*,*,#17634,.T.);
#25237=ORIENTED_EDGE('',*,*,#17631,.T.);
#25238=ORIENTED_EDGE('',*,*,#17635,.T.);
#25239=ORIENTED_EDGE('',*,*,#17636,.F.);
#25240=ORIENTED_EDGE('',*,*,#17637,.F.);
#25241=ORIENTED_EDGE('',*,*,#17638,.F.);
#25242=ORIENTED_EDGE('',*,*,#17639,.T.);
#25243=ORIENTED_EDGE('',*,*,#17640,.T.);
#25244=ORIENTED_EDGE('',*,*,#17637,.T.);
#25245=ORIENTED_EDGE('',*,*,#17641,.T.);
#25246=ORIENTED_EDGE('',*,*,#17622,.T.);
#25247=ORIENTED_EDGE('',*,*,#17642,.T.);
#25248=ORIENTED_EDGE('',*,*,#17638,.T.);
#25249=ORIENTED_EDGE('',*,*,#17643,.T.);
#25250=ORIENTED_EDGE('',*,*,#17636,.T.);
#25251=ORIENTED_EDGE('',*,*,#17644,.T.);
#25252=ORIENTED_EDGE('',*,*,#17632,.T.);
#25253=ORIENTED_EDGE('',*,*,#17645,.T.);
#25254=ORIENTED_EDGE('',*,*,#17630,.T.);
#25255=ORIENTED_EDGE('',*,*,#17646,.T.);
#25256=ORIENTED_EDGE('',*,*,#17618,.T.);
#25257=ORIENTED_EDGE('',*,*,#17647,.T.);
#25258=ORIENTED_EDGE('',*,*,#17616,.T.);
#25259=ORIENTED_EDGE('',*,*,#17648,.T.);
#25260=ORIENTED_EDGE('',*,*,#17604,.T.);
#25261=ORIENTED_EDGE('',*,*,#17649,.T.);
#25262=ORIENTED_EDGE('',*,*,#17607,.F.);
#25263=ORIENTED_EDGE('',*,*,#17615,.F.);
#25264=ORIENTED_EDGE('',*,*,#17612,.F.);
#25265=ORIENTED_EDGE('',*,*,#17650,.T.);
#25266=ORIENTED_EDGE('',*,*,#17613,.F.);
#25267=ORIENTED_EDGE('',*,*,#17629,.F.);
#25268=ORIENTED_EDGE('',*,*,#17626,.F.);
#25269=ORIENTED_EDGE('',*,*,#17651,.T.);
#25270=ORIENTED_EDGE('',*,*,#17627,.F.);
#25271=ORIENTED_EDGE('',*,*,#17643,.F.);
#25272=ORIENTED_EDGE('',*,*,#17640,.F.);
#25273=ORIENTED_EDGE('',*,*,#17652,.T.);
#25274=ORIENTED_EDGE('',*,*,#17614,.F.);
#25275=ORIENTED_EDGE('',*,*,#17648,.F.);
#25276=ORIENTED_EDGE('',*,*,#17646,.F.);
#25277=ORIENTED_EDGE('',*,*,#17644,.F.);
#25278=ORIENTED_EDGE('',*,*,#17642,.F.);
#25279=ORIENTED_EDGE('',*,*,#17628,.F.);
#25280=ORIENTED_EDGE('',*,*,#17653,.F.);
#25281=ORIENTED_EDGE('',*,*,#17654,.F.);
#25282=ORIENTED_EDGE('',*,*,#17655,.F.);
#25283=ORIENTED_EDGE('',*,*,#17656,.F.);
#25284=ORIENTED_EDGE('',*,*,#17657,.F.);
#25285=ORIENTED_EDGE('',*,*,#17658,.F.);
#25286=ORIENTED_EDGE('',*,*,#17656,.T.);
#25287=ORIENTED_EDGE('',*,*,#17659,.T.);
#25288=ORIENTED_EDGE('',*,*,#17660,.T.);
#25289=ORIENTED_EDGE('',*,*,#17661,.F.);
#25290=ORIENTED_EDGE('',*,*,#17655,.T.);
#25291=ORIENTED_EDGE('',*,*,#17662,.T.);
#25292=ORIENTED_EDGE('',*,*,#17663,.T.);
#25293=ORIENTED_EDGE('',*,*,#17659,.F.);
#25294=ORIENTED_EDGE('',*,*,#17653,.T.);
#25295=ORIENTED_EDGE('',*,*,#17664,.T.);
#25296=ORIENTED_EDGE('',*,*,#17665,.T.);
#25297=ORIENTED_EDGE('',*,*,#17666,.T.);
#25298=ORIENTED_EDGE('',*,*,#17667,.T.);
#25299=ORIENTED_EDGE('',*,*,#17664,.F.);
#25300=ORIENTED_EDGE('',*,*,#17658,.T.);
#25301=ORIENTED_EDGE('',*,*,#17668,.T.);
#25302=ORIENTED_EDGE('',*,*,#17654,.T.);
#25303=ORIENTED_EDGE('',*,*,#17666,.F.);
#25304=ORIENTED_EDGE('',*,*,#17669,.T.);
#25305=ORIENTED_EDGE('',*,*,#17662,.F.);
#25306=ORIENTED_EDGE('',*,*,#17670,.T.);
#25307=ORIENTED_EDGE('',*,*,#17668,.F.);
#25308=ORIENTED_EDGE('',*,*,#17657,.T.);
#25309=ORIENTED_EDGE('',*,*,#17661,.T.);
#25310=ORIENTED_EDGE('',*,*,#17663,.F.);
#25311=ORIENTED_EDGE('',*,*,#17671,.T.);
#25312=ORIENTED_EDGE('',*,*,#17672,.T.);
#25313=ORIENTED_EDGE('',*,*,#17673,.F.);
#25314=ORIENTED_EDGE('',*,*,#17669,.F.);
#25315=ORIENTED_EDGE('',*,*,#17674,.T.);
#25316=ORIENTED_EDGE('',*,*,#17675,.T.);
#25317=ORIENTED_EDGE('',*,*,#17671,.F.);
#25318=ORIENTED_EDGE('',*,*,#17665,.F.);
#25319=ORIENTED_EDGE('',*,*,#17676,.T.);
#25320=ORIENTED_EDGE('',*,*,#17677,.T.);
#25321=ORIENTED_EDGE('',*,*,#17674,.F.);
#25322=ORIENTED_EDGE('',*,*,#17667,.F.);
#25323=ORIENTED_EDGE('',*,*,#17678,.T.);
#25324=ORIENTED_EDGE('',*,*,#17679,.T.);
#25325=ORIENTED_EDGE('',*,*,#17676,.F.);
#25326=ORIENTED_EDGE('',*,*,#17670,.F.);
#25327=ORIENTED_EDGE('',*,*,#17680,.T.);
#25328=ORIENTED_EDGE('',*,*,#17681,.T.);
#25329=ORIENTED_EDGE('',*,*,#17678,.F.);
#25330=ORIENTED_EDGE('',*,*,#17660,.F.);
#25331=ORIENTED_EDGE('',*,*,#17673,.T.);
#25332=ORIENTED_EDGE('',*,*,#17682,.T.);
#25333=ORIENTED_EDGE('',*,*,#17680,.F.);
#25334=ORIENTED_EDGE('',*,*,#17675,.F.);
#25335=ORIENTED_EDGE('',*,*,#17677,.F.);
#25336=ORIENTED_EDGE('',*,*,#17679,.F.);
#25337=ORIENTED_EDGE('',*,*,#17681,.F.);
#25338=ORIENTED_EDGE('',*,*,#17682,.F.);
#25339=ORIENTED_EDGE('',*,*,#17672,.F.);
#25340=ORIENTED_EDGE('',*,*,#17605,.F.);
#25341=ORIENTED_EDGE('',*,*,#17650,.F.);
#25342=ORIENTED_EDGE('',*,*,#17611,.F.);
#25343=ORIENTED_EDGE('',*,*,#17651,.F.);
#25344=ORIENTED_EDGE('',*,*,#17625,.F.);
#25345=ORIENTED_EDGE('',*,*,#17652,.F.);
#25346=ORIENTED_EDGE('',*,*,#17639,.F.);
#25347=ORIENTED_EDGE('',*,*,#17683,.F.);
#25348=ORIENTED_EDGE('',*,*,#17633,.F.);
#25349=ORIENTED_EDGE('',*,*,#17684,.F.);
#25350=ORIENTED_EDGE('',*,*,#17619,.F.);
#25351=ORIENTED_EDGE('',*,*,#17685,.F.);
#25352=ORIENTED_EDGE('',*,*,#17686,.T.);
#25353=ORIENTED_EDGE('',*,*,#17634,.F.);
#25354=ORIENTED_EDGE('',*,*,#17683,.T.);
#25355=ORIENTED_EDGE('',*,*,#17641,.F.);
#25356=ORIENTED_EDGE('',*,*,#17645,.F.);
#25357=ORIENTED_EDGE('',*,*,#17620,.F.);
#25358=ORIENTED_EDGE('',*,*,#17684,.T.);
#25359=ORIENTED_EDGE('',*,*,#17635,.F.);
#25360=ORIENTED_EDGE('',*,*,#17647,.F.);
#25361=ORIENTED_EDGE('',*,*,#17606,.F.);
#25362=ORIENTED_EDGE('',*,*,#17685,.T.);
#25363=ORIENTED_EDGE('',*,*,#17621,.F.);
#25364=ORIENTED_EDGE('',*,*,#17649,.F.);
#25365=ORIENTED_EDGE('',*,*,#17687,.F.);
#25366=ORIENTED_EDGE('',*,*,#17688,.F.);
#25367=ORIENTED_EDGE('',*,*,#17689,.T.);
#25368=ORIENTED_EDGE('',*,*,#17687,.T.);
#25369=ORIENTED_EDGE('',*,*,#17689,.F.);
#25370=ORIENTED_EDGE('',*,*,#17686,.F.);
#25371=ORIENTED_EDGE('',*,*,#17690,.T.);
#25372=ORIENTED_EDGE('',*,*,#17688,.T.);
#25373=ORIENTED_EDGE('',*,*,#17690,.F.);
#25374=ORIENTED_EDGE('',*,*,#17691,.F.);
#25375=ORIENTED_EDGE('',*,*,#17692,.T.);
#25376=ORIENTED_EDGE('',*,*,#17693,.T.);
#25377=ORIENTED_EDGE('',*,*,#17694,.T.);
#25378=ORIENTED_EDGE('',*,*,#17695,.F.);
#25379=ORIENTED_EDGE('',*,*,#17696,.T.);
#25380=ORIENTED_EDGE('',*,*,#17691,.T.);
#25381=ORIENTED_EDGE('',*,*,#17697,.T.);
#25382=ORIENTED_EDGE('',*,*,#17698,.F.);
#25383=ORIENTED_EDGE('',*,*,#17699,.T.);
#25384=ORIENTED_EDGE('',*,*,#17695,.T.);
#25385=ORIENTED_EDGE('',*,*,#17700,.T.);
#25386=ORIENTED_EDGE('',*,*,#17701,.F.);
#25387=ORIENTED_EDGE('',*,*,#17702,.T.);
#25388=ORIENTED_EDGE('',*,*,#17698,.T.);
#25389=ORIENTED_EDGE('',*,*,#17703,.T.);
#25390=ORIENTED_EDGE('',*,*,#17704,.F.);
#25391=ORIENTED_EDGE('',*,*,#17705,.T.);
#25392=ORIENTED_EDGE('',*,*,#17701,.T.);
#25393=ORIENTED_EDGE('',*,*,#17706,.T.);
#25394=ORIENTED_EDGE('',*,*,#17707,.F.);
#25395=ORIENTED_EDGE('',*,*,#17708,.T.);
#25396=ORIENTED_EDGE('',*,*,#17704,.T.);
#25397=ORIENTED_EDGE('',*,*,#17709,.T.);
#25398=ORIENTED_EDGE('',*,*,#17710,.F.);
#25399=ORIENTED_EDGE('',*,*,#17711,.T.);
#25400=ORIENTED_EDGE('',*,*,#17707,.T.);
#25401=ORIENTED_EDGE('',*,*,#17712,.T.);
#25402=ORIENTED_EDGE('',*,*,#17713,.F.);
#25403=ORIENTED_EDGE('',*,*,#17714,.T.);
#25404=ORIENTED_EDGE('',*,*,#17710,.T.);
#25405=ORIENTED_EDGE('',*,*,#17715,.T.);
#25406=ORIENTED_EDGE('',*,*,#17716,.F.);
#25407=ORIENTED_EDGE('',*,*,#17717,.T.);
#25408=ORIENTED_EDGE('',*,*,#17713,.T.);
#25409=ORIENTED_EDGE('',*,*,#17718,.T.);
#25410=ORIENTED_EDGE('',*,*,#17719,.F.);
#25411=ORIENTED_EDGE('',*,*,#17720,.T.);
#25412=ORIENTED_EDGE('',*,*,#17716,.T.);
#25413=ORIENTED_EDGE('',*,*,#17721,.T.);
#25414=ORIENTED_EDGE('',*,*,#17722,.F.);
#25415=ORIENTED_EDGE('',*,*,#17723,.T.);
#25416=ORIENTED_EDGE('',*,*,#17719,.T.);
#25417=ORIENTED_EDGE('',*,*,#17724,.T.);
#25418=ORIENTED_EDGE('',*,*,#17725,.F.);
#25419=ORIENTED_EDGE('',*,*,#17726,.T.);
#25420=ORIENTED_EDGE('',*,*,#17722,.T.);
#25421=ORIENTED_EDGE('',*,*,#17727,.T.);
#25422=ORIENTED_EDGE('',*,*,#17728,.F.);
#25423=ORIENTED_EDGE('',*,*,#17729,.F.);
#25424=ORIENTED_EDGE('',*,*,#17730,.T.);
#25425=ORIENTED_EDGE('',*,*,#17725,.T.);
#25426=ORIENTED_EDGE('',*,*,#17731,.T.);
#25427=ORIENTED_EDGE('',*,*,#17732,.F.);
#25428=ORIENTED_EDGE('',*,*,#17733,.T.);
#25429=ORIENTED_EDGE('',*,*,#17734,.F.);
#25430=ORIENTED_EDGE('',*,*,#17735,.F.);
#25431=ORIENTED_EDGE('',*,*,#17736,.F.);
#25432=ORIENTED_EDGE('',*,*,#17737,.T.);
#25433=ORIENTED_EDGE('',*,*,#17732,.T.);
#25434=ORIENTED_EDGE('',*,*,#17738,.F.);
#25435=ORIENTED_EDGE('',*,*,#17739,.F.);
#25436=ORIENTED_EDGE('',*,*,#17740,.T.);
#25437=ORIENTED_EDGE('',*,*,#17736,.T.);
#25438=ORIENTED_EDGE('',*,*,#17741,.F.);
#25439=ORIENTED_EDGE('',*,*,#17742,.F.);
#25440=ORIENTED_EDGE('',*,*,#17743,.T.);
#25441=ORIENTED_EDGE('',*,*,#17739,.T.);
#25442=ORIENTED_EDGE('',*,*,#17744,.F.);
#25443=ORIENTED_EDGE('',*,*,#17745,.F.);
#25444=ORIENTED_EDGE('',*,*,#17746,.T.);
#25445=ORIENTED_EDGE('',*,*,#17742,.T.);
#25446=ORIENTED_EDGE('',*,*,#17747,.F.);
#25447=ORIENTED_EDGE('',*,*,#17748,.F.);
#25448=ORIENTED_EDGE('',*,*,#17749,.T.);
#25449=ORIENTED_EDGE('',*,*,#17745,.T.);
#25450=ORIENTED_EDGE('',*,*,#17750,.F.);
#25451=ORIENTED_EDGE('',*,*,#17751,.F.);
#25452=ORIENTED_EDGE('',*,*,#17752,.T.);
#25453=ORIENTED_EDGE('',*,*,#17748,.T.);
#25454=ORIENTED_EDGE('',*,*,#17753,.F.);
#25455=ORIENTED_EDGE('',*,*,#17754,.F.);
#25456=ORIENTED_EDGE('',*,*,#17755,.T.);
#25457=ORIENTED_EDGE('',*,*,#17751,.T.);
#25458=ORIENTED_EDGE('',*,*,#17756,.F.);
#25459=ORIENTED_EDGE('',*,*,#17757,.F.);
#25460=ORIENTED_EDGE('',*,*,#17758,.T.);
#25461=ORIENTED_EDGE('',*,*,#17754,.T.);
#25462=ORIENTED_EDGE('',*,*,#17759,.F.);
#25463=ORIENTED_EDGE('',*,*,#17760,.F.);
#25464=ORIENTED_EDGE('',*,*,#17761,.T.);
#25465=ORIENTED_EDGE('',*,*,#17757,.T.);
#25466=ORIENTED_EDGE('',*,*,#17762,.F.);
#25467=ORIENTED_EDGE('',*,*,#17763,.F.);
#25468=ORIENTED_EDGE('',*,*,#17764,.T.);
#25469=ORIENTED_EDGE('',*,*,#17760,.T.);
#25470=ORIENTED_EDGE('',*,*,#17765,.F.);
#25471=ORIENTED_EDGE('',*,*,#17766,.F.);
#25472=ORIENTED_EDGE('',*,*,#17767,.T.);
#25473=ORIENTED_EDGE('',*,*,#17763,.T.);
#25474=ORIENTED_EDGE('',*,*,#17768,.F.);
#25475=ORIENTED_EDGE('',*,*,#17769,.F.);
#25476=ORIENTED_EDGE('',*,*,#17770,.F.);
#25477=ORIENTED_EDGE('',*,*,#17731,.F.);
#25478=ORIENTED_EDGE('',*,*,#17727,.F.);
#25479=ORIENTED_EDGE('',*,*,#17724,.F.);
#25480=ORIENTED_EDGE('',*,*,#17721,.F.);
#25481=ORIENTED_EDGE('',*,*,#17718,.F.);
#25482=ORIENTED_EDGE('',*,*,#17715,.F.);
#25483=ORIENTED_EDGE('',*,*,#17712,.F.);
#25484=ORIENTED_EDGE('',*,*,#17709,.F.);
#25485=ORIENTED_EDGE('',*,*,#17706,.F.);
#25486=ORIENTED_EDGE('',*,*,#17703,.F.);
#25487=ORIENTED_EDGE('',*,*,#17700,.F.);
#25488=ORIENTED_EDGE('',*,*,#17697,.F.);
#25489=ORIENTED_EDGE('',*,*,#17694,.F.);
#25490=ORIENTED_EDGE('',*,*,#17771,.F.);
#25491=ORIENTED_EDGE('',*,*,#17772,.T.);
#25492=ORIENTED_EDGE('',*,*,#17768,.T.);
#25493=ORIENTED_EDGE('',*,*,#17765,.T.);
#25494=ORIENTED_EDGE('',*,*,#17762,.T.);
#25495=ORIENTED_EDGE('',*,*,#17759,.T.);
#25496=ORIENTED_EDGE('',*,*,#17756,.T.);
#25497=ORIENTED_EDGE('',*,*,#17753,.T.);
#25498=ORIENTED_EDGE('',*,*,#17750,.T.);
#25499=ORIENTED_EDGE('',*,*,#17747,.T.);
#25500=ORIENTED_EDGE('',*,*,#17744,.T.);
#25501=ORIENTED_EDGE('',*,*,#17741,.T.);
#25502=ORIENTED_EDGE('',*,*,#17738,.T.);
#25503=ORIENTED_EDGE('',*,*,#17735,.T.);
#25504=ORIENTED_EDGE('',*,*,#17773,.T.);
#25505=ORIENTED_EDGE('',*,*,#17774,.T.);
#25506=ORIENTED_EDGE('',*,*,#17775,.T.);
#25507=ORIENTED_EDGE('',*,*,#17776,.T.);
#25508=ORIENTED_EDGE('',*,*,#17771,.T.);
#25509=ORIENTED_EDGE('',*,*,#17766,.T.);
#25510=ORIENTED_EDGE('',*,*,#17772,.F.);
#25511=ORIENTED_EDGE('',*,*,#17776,.F.);
#25512=ORIENTED_EDGE('',*,*,#17777,.T.);
#25513=ORIENTED_EDGE('',*,*,#17778,.F.);
#25514=ORIENTED_EDGE('',*,*,#17733,.F.);
#25515=ORIENTED_EDGE('',*,*,#17737,.F.);
#25516=ORIENTED_EDGE('',*,*,#17740,.F.);
#25517=ORIENTED_EDGE('',*,*,#17743,.F.);
#25518=ORIENTED_EDGE('',*,*,#17746,.F.);
#25519=ORIENTED_EDGE('',*,*,#17749,.F.);
#25520=ORIENTED_EDGE('',*,*,#17752,.F.);
#25521=ORIENTED_EDGE('',*,*,#17755,.F.);
#25522=ORIENTED_EDGE('',*,*,#17758,.F.);
#25523=ORIENTED_EDGE('',*,*,#17761,.F.);
#25524=ORIENTED_EDGE('',*,*,#17764,.F.);
#25525=ORIENTED_EDGE('',*,*,#17767,.F.);
#25526=ORIENTED_EDGE('',*,*,#17777,.F.);
#25527=ORIENTED_EDGE('',*,*,#17775,.F.);
#25528=ORIENTED_EDGE('',*,*,#17692,.F.);
#25529=ORIENTED_EDGE('',*,*,#17696,.F.);
#25530=ORIENTED_EDGE('',*,*,#17699,.F.);
#25531=ORIENTED_EDGE('',*,*,#17702,.F.);
#25532=ORIENTED_EDGE('',*,*,#17705,.F.);
#25533=ORIENTED_EDGE('',*,*,#17708,.F.);
#25534=ORIENTED_EDGE('',*,*,#17711,.F.);
#25535=ORIENTED_EDGE('',*,*,#17714,.F.);
#25536=ORIENTED_EDGE('',*,*,#17717,.F.);
#25537=ORIENTED_EDGE('',*,*,#17720,.F.);
#25538=ORIENTED_EDGE('',*,*,#17723,.F.);
#25539=ORIENTED_EDGE('',*,*,#17726,.F.);
#25540=ORIENTED_EDGE('',*,*,#17730,.F.);
#25541=ORIENTED_EDGE('',*,*,#17779,.F.);
#25542=ORIENTED_EDGE('',*,*,#17780,.T.);
#25543=ORIENTED_EDGE('',*,*,#17781,.T.);
#25544=ORIENTED_EDGE('',*,*,#17782,.F.);
#25545=ORIENTED_EDGE('',*,*,#17783,.F.);
#25546=ORIENTED_EDGE('',*,*,#17782,.T.);
#25547=ORIENTED_EDGE('',*,*,#17784,.T.);
#25548=ORIENTED_EDGE('',*,*,#17785,.F.);
#25549=ORIENTED_EDGE('',*,*,#17786,.F.);
#25550=ORIENTED_EDGE('',*,*,#17785,.T.);
#25551=ORIENTED_EDGE('',*,*,#17787,.T.);
#25552=ORIENTED_EDGE('',*,*,#17788,.F.);
#25553=ORIENTED_EDGE('',*,*,#17789,.F.);
#25554=ORIENTED_EDGE('',*,*,#17788,.T.);
#25555=ORIENTED_EDGE('',*,*,#17790,.T.);
#25556=ORIENTED_EDGE('',*,*,#17791,.F.);
#25557=ORIENTED_EDGE('',*,*,#17792,.F.);
#25558=ORIENTED_EDGE('',*,*,#17793,.T.);
#25559=ORIENTED_EDGE('',*,*,#17794,.T.);
#25560=ORIENTED_EDGE('',*,*,#17780,.F.);
#25561=ORIENTED_EDGE('',*,*,#17795,.F.);
#25562=ORIENTED_EDGE('',*,*,#17791,.T.);
#25563=ORIENTED_EDGE('',*,*,#17796,.T.);
#25564=ORIENTED_EDGE('',*,*,#17793,.F.);
#25565=ORIENTED_EDGE('',*,*,#17796,.F.);
#25566=ORIENTED_EDGE('',*,*,#17790,.F.);
#25567=ORIENTED_EDGE('',*,*,#17787,.F.);
#25568=ORIENTED_EDGE('',*,*,#17784,.F.);
#25569=ORIENTED_EDGE('',*,*,#17781,.F.);
#25570=ORIENTED_EDGE('',*,*,#17794,.F.);
#25571=ORIENTED_EDGE('',*,*,#17797,.F.);
#25572=ORIENTED_EDGE('',*,*,#17773,.F.);
#25573=ORIENTED_EDGE('',*,*,#17693,.F.);
#25574=ORIENTED_EDGE('',*,*,#17774,.F.);
#25575=ORIENTED_EDGE('',*,*,#17798,.T.);
#25576=ORIENTED_EDGE('',*,*,#17797,.T.);
#25577=ORIENTED_EDGE('',*,*,#17798,.F.);
#25578=ORIENTED_EDGE('',*,*,#17728,.T.);
#25579=ORIENTED_EDGE('',*,*,#17770,.T.);
#25580=ORIENTED_EDGE('',*,*,#17799,.F.);
#25581=ORIENTED_EDGE('',*,*,#17800,.F.);
#25582=ORIENTED_EDGE('',*,*,#17729,.T.);
#25583=ORIENTED_EDGE('',*,*,#17799,.T.);
#25584=ORIENTED_EDGE('',*,*,#17769,.T.);
#25585=ORIENTED_EDGE('',*,*,#17734,.T.);
#25586=ORIENTED_EDGE('',*,*,#17778,.T.);
#25587=ORIENTED_EDGE('',*,*,#17789,.T.);
#25588=ORIENTED_EDGE('',*,*,#17795,.T.);
#25589=ORIENTED_EDGE('',*,*,#17792,.T.);
#25590=ORIENTED_EDGE('',*,*,#17779,.T.);
#25591=ORIENTED_EDGE('',*,*,#17783,.T.);
#25592=ORIENTED_EDGE('',*,*,#17786,.T.);
#25593=ORIENTED_EDGE('',*,*,#17801,.T.);
#25594=ORIENTED_EDGE('',*,*,#17800,.T.);
#25595=ORIENTED_EDGE('',*,*,#17801,.F.);
#25596=TOROIDAL_SURFACE('',#27464,90.,2.);
#25597=TOROIDAL_SURFACE('',#27481,90.,2.);
#25598=TOROIDAL_SURFACE('',#27609,72.2,2.);
#25599=TOROIDAL_SURFACE('',#27616,22.05,2.);
#25600=TOROIDAL_SURFACE('',#27625,55.,2.);
#25601=TOROIDAL_SURFACE('',#27632,18.75,2.);
#25602=TOROIDAL_SURFACE('',#27639,18.75,2.);
#25603=TOROIDAL_SURFACE('',#27654,3.99999999999996,2.);
#25604=TOROIDAL_SURFACE('',#27659,3.99999999999999,2.);
#25605=TOROIDAL_SURFACE('',#27669,3.99999999999996,2.);
#25606=TOROIDAL_SURFACE('',#27674,3.99999999999997,2.);
#25607=TOROIDAL_SURFACE('',#27679,3.99999999999998,2.);
#25608=TOROIDAL_SURFACE('',#27685,3.99999999999999,2.);
#25609=TOROIDAL_SURFACE('',#27696,18.75,2.);
#25610=TOROIDAL_SURFACE('',#27702,18.75,2.);
#25611=TOROIDAL_SURFACE('',#27817,90.5,1.5);
#25612=TOROIDAL_SURFACE('',#27825,90.3786796564403,1.5);
#25613=TOROIDAL_SURFACE('',#27846,90.5,1.5);
#25614=TOROIDAL_SURFACE('',#27875,54.8786796564404,1.5);
#25615=TOROIDAL_SURFACE('',#27889,55.,1.5);
#25616=TOROIDAL_SURFACE('',#27895,55.5,1.5);
#25617=TOROIDAL_SURFACE('',#27902,71.7,1.5);
#25618=TOROIDAL_SURFACE('',#27910,76.55,1.5);
#25619=TOROIDAL_SURFACE('',#28097,68.,2.);
#25620=TOROIDAL_SURFACE('',#28109,68.,2.);
#25621=TOROIDAL_SURFACE('',#28118,123.013975850864,2.);
#25622=TOROIDAL_SURFACE('',#28126,118.739209725433,2.);
#25623=TOROIDAL_SURFACE('',#28135,63.9364279314891,2.);
#25624=TOROIDAL_SURFACE('',#28138,63.9364279314891,2.);
#25625=TOROIDAL_SURFACE('',#28141,63.9364279314891,2.);
#25626=TOROIDAL_SURFACE('',#28164,123.,2.);
#25627=TOROIDAL_SURFACE('',#28168,47.,2.);
#25628=TOROIDAL_SURFACE('',#28184,92.1,2.);
#25629=TOROIDAL_SURFACE('',#28190,47.,2.);
#25630=TOROIDAL_SURFACE('',#28197,7.99999999999998,2.);
#25631=TOROIDAL_SURFACE('',#28203,7.99999999999999,2.);
#25632=TOROIDAL_SURFACE('',#28209,8.00000000000001,2.);
#25633=TOROIDAL_SURFACE('',#28215,8.00000000000001,2.);
#25634=TOROIDAL_SURFACE('',#28228,8.00000000000001,2.);
#25635=TOROIDAL_SURFACE('',#28234,8.00000000000001,2.);
#25636=TOROIDAL_SURFACE('',#28240,7.99999999999999,2.);
#25637=TOROIDAL_SURFACE('',#28245,7.99999999999998,2.);
#25638=TOROIDAL_SURFACE('',#28254,6.,2.);
#25639=TOROIDAL_SURFACE('',#28260,6.,2.);
#25640=TOROIDAL_SURFACE('',#28266,6.,2.);
#25641=TOROIDAL_SURFACE('',#28272,6.,2.);
#25642=TOROIDAL_SURFACE('',#28287,7.99999999999998,2.);
#25643=TOROIDAL_SURFACE('',#28292,8.00000000000001,2.);
#25644=TOROIDAL_SURFACE('',#28297,8.00000000000001,2.);
#25645=TOROIDAL_SURFACE('',#28302,7.99999999999999,2.);
#25646=TOROIDAL_SURFACE('',#28313,7.99999999999999,2.);
#25647=TOROIDAL_SURFACE('',#28318,8.00000000000001,2.);
#25648=TOROIDAL_SURFACE('',#28323,8.00000000000001,2.);
#25649=TOROIDAL_SURFACE('',#28327,7.99999999999998,2.);
#25650=TOROIDAL_SURFACE('',#29197,73.5,1.5);
#25651=ADVANCED_FACE('',(#6827),#25596,.T.);
#25652=ADVANCED_FACE('',(#6828),#6500,.T.);
#25653=ADVANCED_FACE('',(#6829,#605,#606,#607,#608,#609),#757,.T.);
#25654=ADVANCED_FACE('',(#6830),#25597,.T.);
#25655=ADVANCED_FACE('',(#6831,#610,#611,#612,#613,#614,#615,#616,#617,
#618),#758,.T.);
#25656=ADVANCED_FACE('',(#6832),#6501,.T.);
#25657=ADVANCED_FACE('',(#6833),#584,.F.);
#25658=ADVANCED_FACE('',(#6834),#6502,.T.);
#25659=ADVANCED_FACE('',(#6835),#585,.F.);
#25660=ADVANCED_FACE('',(#6836),#6503,.T.);
#25661=ADVANCED_FACE('',(#6837),#586,.F.);
#25662=ADVANCED_FACE('',(#6838),#6504,.T.);
#25663=ADVANCED_FACE('',(#6839),#587,.F.);
#25664=ADVANCED_FACE('',(#6840),#6505,.T.);
#25665=ADVANCED_FACE('',(#6841),#759,.T.);
#25666=ADVANCED_FACE('',(#6842),#6506,.T.);
#25667=ADVANCED_FACE('',(#6843),#760,.T.);
#25668=ADVANCED_FACE('',(#6844,#619,#620),#761,.F.);
#25669=ADVANCED_FACE('',(#6845),#6507,.T.);
#25670=ADVANCED_FACE('',(#6846),#588,.F.);
#25671=ADVANCED_FACE('',(#6847),#6508,.T.);
#25672=ADVANCED_FACE('',(#6848),#589,.F.);
#25673=ADVANCED_FACE('',(#6849),#6509,.T.);
#25674=ADVANCED_FACE('',(#6850),#590,.F.);
#25675=ADVANCED_FACE('',(#6851),#6510,.T.);
#25676=ADVANCED_FACE('',(#6852),#591,.F.);
#25677=ADVANCED_FACE('',(#6853),#762,.T.);
#25678=ADVANCED_FACE('',(#6854),#6511,.T.);
#25679=ADVANCED_FACE('',(#6855),#763,.T.);
#25680=ADVANCED_FACE('',(#6856,#621,#622,#623),#764,.T.);
#25681=ADVANCED_FACE('',(#6857),#6512,.T.);
#25682=ADVANCED_FACE('',(#6858),#592,.F.);
#25683=ADVANCED_FACE('',(#6859),#6513,.T.);
#25684=ADVANCED_FACE('',(#6860),#593,.F.);
#25685=ADVANCED_FACE('',(#6861),#6514,.T.);
#25686=ADVANCED_FACE('',(#6862),#594,.F.);
#25687=ADVANCED_FACE('',(#6863),#6515,.T.);
#25688=ADVANCED_FACE('',(#6864),#595,.F.);
#25689=ADVANCED_FACE('',(#6865),#6516,.T.);
#25690=ADVANCED_FACE('',(#6866),#765,.T.);
#25691=ADVANCED_FACE('',(#6867),#6517,.T.);
#25692=ADVANCED_FACE('',(#6868),#766,.T.);
#25693=ADVANCED_FACE('',(#6869,#624),#767,.T.);
#25694=ADVANCED_FACE('',(#6870),#6518,.T.);
#25695=ADVANCED_FACE('',(#6871),#596,.F.);
#25696=ADVANCED_FACE('',(#6872),#6519,.T.);
#25697=ADVANCED_FACE('',(#6873),#597,.F.);
#25698=ADVANCED_FACE('',(#6874),#6520,.T.);
#25699=ADVANCED_FACE('',(#6875),#598,.F.);
#25700=ADVANCED_FACE('',(#6876),#6521,.T.);
#25701=ADVANCED_FACE('',(#6877),#599,.F.);
#25702=ADVANCED_FACE('',(#6878),#6522,.T.);
#25703=ADVANCED_FACE('',(#6879),#768,.T.);
#25704=ADVANCED_FACE('',(#6880),#6523,.T.);
#25705=ADVANCED_FACE('',(#6881),#769,.T.);
#25706=ADVANCED_FACE('',(#6882,#625),#770,.T.);
#25707=ADVANCED_FACE('',(#6883),#25598,.T.);
#25708=ADVANCED_FACE('',(#6884),#6524,.F.);
#25709=ADVANCED_FACE('',(#6885),#25599,.T.);
#25710=ADVANCED_FACE('',(#6886,#626),#771,.F.);
#25711=ADVANCED_FACE('',(#6887),#6525,.F.);
#25712=ADVANCED_FACE('',(#6888),#6526,.T.);
#25713=ADVANCED_FACE('',(#6889),#25600,.T.);
#25714=ADVANCED_FACE('',(#6890),#6527,.T.);
#25715=ADVANCED_FACE('',(#6891),#772,.F.);
#25716=ADVANCED_FACE('',(#6892),#6528,.T.);
#25717=ADVANCED_FACE('',(#6893),#773,.F.);
#25718=ADVANCED_FACE('',(#6894),#25601,.T.);
#25719=ADVANCED_FACE('',(#6895),#492,.F.);
#25720=ADVANCED_FACE('',(#6896),#25602,.T.);
#25721=ADVANCED_FACE('',(#6897),#493,.F.);
#25722=ADVANCED_FACE('',(#6898),#6529,.T.);
#25723=ADVANCED_FACE('',(#6899),#774,.T.);
#25724=ADVANCED_FACE('',(#6900),#6530,.F.);
#25725=ADVANCED_FACE('',(#6901),#6531,.T.);
#25726=ADVANCED_FACE('',(#6902),#6532,.T.);
#25727=ADVANCED_FACE('',(#6903),#25603,.T.);
#25728=ADVANCED_FACE('',(#6904),#6533,.T.);
#25729=ADVANCED_FACE('',(#6905),#25604,.T.);
#25730=ADVANCED_FACE('',(#6906),#6534,.T.);
#25731=ADVANCED_FACE('',(#6907),#775,.T.);
#25732=ADVANCED_FACE('',(#6908),#776,.F.);
#25733=ADVANCED_FACE('',(#6909),#6535,.T.);
#25734=ADVANCED_FACE('',(#6910),#25605,.T.);
#25735=ADVANCED_FACE('',(#6911),#6536,.T.);
#25736=ADVANCED_FACE('',(#6912),#25606,.T.);
#25737=ADVANCED_FACE('',(#6913),#6537,.T.);
#25738=ADVANCED_FACE('',(#6914),#25607,.T.);
#25739=ADVANCED_FACE('',(#6915),#6538,.T.);
#25740=ADVANCED_FACE('',(#6916),#25608,.T.);
#25741=ADVANCED_FACE('',(#6917),#777,.T.);
#25742=ADVANCED_FACE('',(#6918,#627,#628,#629),#778,.T.);
#25743=ADVANCED_FACE('',(#6919),#25609,.T.);
#25744=ADVANCED_FACE('',(#6920),#494,.F.);
#25745=ADVANCED_FACE('',(#6921),#25610,.T.);
#25746=ADVANCED_FACE('',(#6922),#495,.F.);
#25747=ADVANCED_FACE('',(#6923),#6539,.T.);
#25748=ADVANCED_FACE('',(#6924),#6540,.F.);
#25749=ADVANCED_FACE('',(#6925),#6541,.F.);
#25750=ADVANCED_FACE('',(#6926),#6542,.F.);
#25751=ADVANCED_FACE('',(#6927),#6543,.F.);
#25752=ADVANCED_FACE('',(#6928),#779,.T.);
#25753=ADVANCED_FACE('',(#6929),#6544,.F.);
#25754=ADVANCED_FACE('',(#6930),#780,.T.);
#25755=ADVANCED_FACE('',(#6931),#6545,.F.);
#25756=ADVANCED_FACE('',(#6932),#781,.T.);
#25757=ADVANCED_FACE('',(#6933),#782,.F.);
#25758=ADVANCED_FACE('',(#6934),#783,.T.);
#25759=ADVANCED_FACE('',(#6935),#784,.T.);
#25760=ADVANCED_FACE('',(#6936),#785,.T.);
#25761=ADVANCED_FACE('',(#6937),#6546,.F.);
#25762=ADVANCED_FACE('',(#6938),#786,.T.);
#25763=ADVANCED_FACE('',(#6939),#6547,.F.);
#25764=ADVANCED_FACE('',(#6940),#787,.T.);
#25765=ADVANCED_FACE('',(#6941),#6548,.F.);
#25766=ADVANCED_FACE('',(#6942),#788,.T.);
#25767=ADVANCED_FACE('',(#6943),#6549,.F.);
#25768=ADVANCED_FACE('',(#6944),#789,.T.);
#25769=ADVANCED_FACE('',(#6945),#6550,.F.);
#25770=ADVANCED_FACE('',(#6946),#790,.F.);
#25771=ADVANCED_FACE('',(#6947),#6551,.F.);
#25772=ADVANCED_FACE('',(#6948),#791,.F.);
#25773=ADVANCED_FACE('',(#6949),#6552,.F.);
#25774=ADVANCED_FACE('',(#6950),#792,.F.);
#25775=ADVANCED_FACE('',(#6951),#6553,.F.);
#25776=ADVANCED_FACE('',(#6952),#793,.F.);
#25777=ADVANCED_FACE('',(#6953),#6554,.F.);
#25778=ADVANCED_FACE('',(#6954),#794,.F.);
#25779=ADVANCED_FACE('',(#6955),#6555,.F.);
#25780=ADVANCED_FACE('',(#6956),#795,.F.);
#25781=ADVANCED_FACE('',(#6957),#6556,.F.);
#25782=ADVANCED_FACE('',(#6958),#796,.F.);
#25783=ADVANCED_FACE('',(#6959),#6557,.F.);
#25784=ADVANCED_FACE('',(#6960),#797,.F.);
#25785=ADVANCED_FACE('',(#6961),#798,.F.);
#25786=ADVANCED_FACE('',(#6962,#630),#799,.F.);
#25787=ADVANCED_FACE('',(#6963),#6558,.F.);
#25788=ADVANCED_FACE('',(#6964),#6559,.T.);
#25789=ADVANCED_FACE('',(#6965),#800,.T.);
#25790=ADVANCED_FACE('',(#6966),#6560,.T.);
#25791=ADVANCED_FACE('',(#6967),#801,.T.);
#25792=ADVANCED_FACE('',(#6968),#6561,.T.);
#25793=ADVANCED_FACE('',(#6969),#802,.T.);
#25794=ADVANCED_FACE('',(#6970),#6562,.T.);
#25795=ADVANCED_FACE('',(#6971),#803,.T.);
#25796=ADVANCED_FACE('',(#6972),#6563,.T.);
#25797=ADVANCED_FACE('',(#6973),#6564,.T.);
#25798=ADVANCED_FACE('',(#6974),#804,.T.);
#25799=ADVANCED_FACE('',(#6975),#6565,.T.);
#25800=ADVANCED_FACE('',(#6976),#805,.T.);
#25801=ADVANCED_FACE('',(#6977),#6566,.T.);
#25802=ADVANCED_FACE('',(#6978),#806,.T.);
#25803=ADVANCED_FACE('',(#6979),#6567,.T.);
#25804=ADVANCED_FACE('',(#6980),#807,.T.);
#25805=ADVANCED_FACE('',(#6981),#808,.F.);
#25806=ADVANCED_FACE('',(#6982),#809,.T.);
#25807=ADVANCED_FACE('',(#6983),#6568,.T.);
#25808=ADVANCED_FACE('',(#6984),#496,.T.);
#25809=ADVANCED_FACE('',(#6985),#497,.T.);
#25810=ADVANCED_FACE('',(#6986),#810,.T.);
#25811=ADVANCED_FACE('',(#6987),#811,.T.);
#25812=ADVANCED_FACE('',(#6988),#6569,.T.);
#25813=ADVANCED_FACE('',(#6989),#812,.T.);
#25814=ADVANCED_FACE('',(#6990),#498,.T.);
#25815=ADVANCED_FACE('',(#6991),#499,.T.);
#25816=ADVANCED_FACE('',(#6992),#813,.T.);
#25817=ADVANCED_FACE('',(#6993),#6570,.T.);
#25818=ADVANCED_FACE('',(#6994),#814,.T.);
#25819=ADVANCED_FACE('',(#6995),#500,.T.);
#25820=ADVANCED_FACE('',(#6996),#501,.T.);
#25821=ADVANCED_FACE('',(#6997),#815,.T.);
#25822=ADVANCED_FACE('',(#6998),#816,.T.);
#25823=ADVANCED_FACE('',(#6999),#6571,.T.);
#25824=ADVANCED_FACE('',(#7000),#817,.T.);
#25825=ADVANCED_FACE('',(#7001),#502,.T.);
#25826=ADVANCED_FACE('',(#7002),#503,.T.);
#25827=ADVANCED_FACE('',(#7003),#818,.T.);
#25828=ADVANCED_FACE('',(#7004),#819,.T.);
#25829=ADVANCED_FACE('',(#7005),#6572,.T.);
#25830=ADVANCED_FACE('',(#7006),#820,.T.);
#25831=ADVANCED_FACE('',(#7007),#504,.T.);
#25832=ADVANCED_FACE('',(#7008),#505,.T.);
#25833=ADVANCED_FACE('',(#7009),#821,.T.);
#25834=ADVANCED_FACE('',(#7010),#6573,.T.);
#25835=ADVANCED_FACE('',(#7011),#822,.T.);
#25836=ADVANCED_FACE('',(#7012),#506,.T.);
#25837=ADVANCED_FACE('',(#7013),#507,.T.);
#25838=ADVANCED_FACE('',(#7014),#823,.T.);
#25839=ADVANCED_FACE('',(#7015),#824,.T.);
#25840=ADVANCED_FACE('',(#7016),#6574,.T.);
#25841=ADVANCED_FACE('',(#7017),#825,.T.);
#25842=ADVANCED_FACE('',(#7018),#508,.T.);
#25843=ADVANCED_FACE('',(#7019),#509,.T.);
#25844=ADVANCED_FACE('',(#7020),#826,.T.);
#25845=ADVANCED_FACE('',(#7021),#6575,.T.);
#25846=ADVANCED_FACE('',(#7022),#827,.T.);
#25847=ADVANCED_FACE('',(#7023),#25611,.T.);
#25848=ADVANCED_FACE('',(#7024),#339,.T.);
#25849=ADVANCED_FACE('',(#7025),#6576,.T.);
#25850=ADVANCED_FACE('',(#7026),#25612,.T.);
#25851=ADVANCED_FACE('',(#7027,#631,#632,#633,#634,#635,#636,#637,#638,
#639),#828,.T.);
#25852=ADVANCED_FACE('',(#7028),#6577,.T.);
#25853=ADVANCED_FACE('',(#7029),#829,.T.);
#25854=ADVANCED_FACE('',(#7030),#6578,.T.);
#25855=ADVANCED_FACE('',(#7031),#830,.T.);
#25856=ADVANCED_FACE('',(#7032),#25613,.T.);
#25857=ADVANCED_FACE('',(#7033,#640),#831,.T.);
#25858=ADVANCED_FACE('',(#7034),#25614,.T.);
#25859=ADVANCED_FACE('',(#7035),#340,.T.);
#25860=ADVANCED_FACE('',(#7036,#641,#642,#643,#644,#645),#832,.T.);
#25861=ADVANCED_FACE('',(#7037),#6579,.T.);
#25862=ADVANCED_FACE('',(#7038),#6580,.T.);
#25863=ADVANCED_FACE('',(#7039),#338,.T.);
#25864=ADVANCED_FACE('',(#7040),#6581,.T.);
#25865=ADVANCED_FACE('',(#7041),#833,.T.);
#25866=ADVANCED_FACE('',(#7042),#25615,.T.);
#25867=ADVANCED_FACE('',(#7043),#6582,.T.);
#25868=ADVANCED_FACE('',(#7044),#6583,.T.);
#25869=ADVANCED_FACE('',(#7045),#834,.T.);
#25870=ADVANCED_FACE('',(#7046),#25616,.T.);
#25871=ADVANCED_FACE('',(#7047),#6584,.T.);
#25872=ADVANCED_FACE('',(#7048),#6585,.T.);
#25873=ADVANCED_FACE('',(#7049),#835,.F.);
#25874=ADVANCED_FACE('',(#7050),#25617,.T.);
#25875=ADVANCED_FACE('',(#7051),#6586,.F.);
#25876=ADVANCED_FACE('',(#7052),#25618,.T.);
#25877=ADVANCED_FACE('',(#7053),#6587,.F.);
#25878=ADVANCED_FACE('',(#7054),#6588,.F.);
#25879=ADVANCED_FACE('',(#7055),#6589,.F.);
#25880=ADVANCED_FACE('',(#7056),#6590,.F.);
#25881=ADVANCED_FACE('',(#7057),#6591,.F.);
#25882=ADVANCED_FACE('',(#7058),#6592,.T.);
#25883=ADVANCED_FACE('',(#7059),#6593,.T.);
#25884=ADVANCED_FACE('',(#7060),#6594,.T.);
#25885=ADVANCED_FACE('',(#7061),#6595,.T.);
#25886=ADVANCED_FACE('',(#7062),#6596,.T.);
#25887=ADVANCED_FACE('',(#7063),#836,.F.);
#25888=ADVANCED_FACE('',(#7064),#837,.F.);
#25889=ADVANCED_FACE('',(#7065),#838,.F.);
#25890=ADVANCED_FACE('',(#7066),#839,.F.);
#25891=ADVANCED_FACE('',(#7067),#840,.F.);
#25892=ADVANCED_FACE('',(#7068),#841,.F.);
#25893=ADVANCED_FACE('',(#7069),#842,.F.);
#25894=ADVANCED_FACE('',(#7070),#843,.F.);
#25895=ADVANCED_FACE('',(#7071),#844,.F.);
#25896=ADVANCED_FACE('',(#7072),#845,.F.);
#25897=ADVANCED_FACE('',(#7073),#846,.F.);
#25898=ADVANCED_FACE('',(#7074),#847,.F.);
#25899=ADVANCED_FACE('',(#7075),#848,.F.);
#25900=ADVANCED_FACE('',(#7076),#849,.F.);
#25901=ADVANCED_FACE('',(#7077),#850,.F.);
#25902=ADVANCED_FACE('',(#7078),#851,.F.);
#25903=ADVANCED_FACE('',(#7079),#852,.F.);
#25904=ADVANCED_FACE('',(#7080),#853,.F.);
#25905=ADVANCED_FACE('',(#7081),#854,.F.);
#25906=ADVANCED_FACE('',(#7082),#510,.F.);
#25907=ADVANCED_FACE('',(#7083),#511,.F.);
#25908=ADVANCED_FACE('',(#7084),#512,.F.);
#25909=ADVANCED_FACE('',(#7085),#513,.F.);
#25910=ADVANCED_FACE('',(#7086),#514,.F.);
#25911=ADVANCED_FACE('',(#7087),#515,.F.);
#25912=ADVANCED_FACE('',(#7088),#516,.F.);
#25913=ADVANCED_FACE('',(#7089),#517,.F.);
#25914=ADVANCED_FACE('',(#7090),#518,.F.);
#25915=ADVANCED_FACE('',(#7091),#519,.F.);
#25916=ADVANCED_FACE('',(#7092),#855,.F.);
#25917=ADVANCED_FACE('',(#7093),#856,.F.);
#25918=ADVANCED_FACE('',(#7094),#520,.F.);
#25919=ADVANCED_FACE('',(#7095),#857,.T.);
#25920=ADVANCED_FACE('',(#7096),#521,.F.);
#25921=ADVANCED_FACE('',(#7097),#522,.F.);
#25922=ADVANCED_FACE('',(#7098),#523,.F.);
#25923=ADVANCED_FACE('',(#7099),#524,.F.);
#25924=ADVANCED_FACE('',(#7100),#525,.F.);
#25925=ADVANCED_FACE('',(#7101),#526,.F.);
#25926=ADVANCED_FACE('',(#7102),#527,.F.);
#25927=ADVANCED_FACE('',(#7103),#528,.F.);
#25928=ADVANCED_FACE('',(#7104),#529,.F.);
#25929=ADVANCED_FACE('',(#7105),#530,.F.);
#25930=ADVANCED_FACE('',(#7106),#531,.F.);
#25931=ADVANCED_FACE('',(#7107),#532,.F.);
#25932=ADVANCED_FACE('',(#7108),#533,.F.);
#25933=ADVANCED_FACE('',(#7109),#858,.F.);
#25934=ADVANCED_FACE('',(#7110),#534,.F.);
#25935=ADVANCED_FACE('',(#7111),#535,.F.);
#25936=ADVANCED_FACE('',(#7112),#536,.F.);
#25937=ADVANCED_FACE('',(#7113),#537,.F.);
#25938=ADVANCED_FACE('',(#7114),#538,.F.);
#25939=ADVANCED_FACE('',(#7115),#539,.F.);
#25940=ADVANCED_FACE('',(#7116),#540,.F.);
#25941=ADVANCED_FACE('',(#7117),#541,.F.);
#25942=ADVANCED_FACE('',(#7118),#542,.F.);
#25943=ADVANCED_FACE('',(#7119),#543,.F.);
#25944=ADVANCED_FACE('',(#7120),#544,.F.);
#25945=ADVANCED_FACE('',(#7121),#545,.F.);
#25946=ADVANCED_FACE('',(#7122),#546,.F.);
#25947=ADVANCED_FACE('',(#7123),#547,.F.);
#25948=ADVANCED_FACE('',(#7124),#548,.F.);
#25949=ADVANCED_FACE('',(#7125),#549,.F.);
#25950=ADVANCED_FACE('',(#7126),#550,.F.);
#25951=ADVANCED_FACE('',(#7127),#551,.F.);
#25952=ADVANCED_FACE('',(#7128),#859,.F.);
#25953=ADVANCED_FACE('',(#7129),#552,.F.);
#25954=ADVANCED_FACE('',(#7130),#553,.F.);
#25955=ADVANCED_FACE('',(#7131),#860,.T.);
#25956=ADVANCED_FACE('',(#7132),#861,.F.);
#25957=ADVANCED_FACE('',(#7133),#554,.F.);
#25958=ADVANCED_FACE('',(#7134),#555,.F.);
#25959=ADVANCED_FACE('',(#7135),#556,.F.);
#25960=ADVANCED_FACE('',(#7136),#557,.F.);
#25961=ADVANCED_FACE('',(#7137),#862,.F.);
#25962=ADVANCED_FACE('',(#7138),#863,.F.);
#25963=ADVANCED_FACE('',(#7139),#558,.F.);
#25964=ADVANCED_FACE('',(#7140),#559,.F.);
#25965=ADVANCED_FACE('',(#7141),#560,.F.);
#25966=ADVANCED_FACE('',(#7142),#561,.F.);
#25967=ADVANCED_FACE('',(#7143),#562,.F.);
#25968=ADVANCED_FACE('',(#7144),#563,.F.);
#25969=ADVANCED_FACE('',(#7145),#564,.F.);
#25970=ADVANCED_FACE('',(#7146),#864,.F.);
#25971=ADVANCED_FACE('',(#7147),#865,.F.);
#25972=ADVANCED_FACE('',(#7148),#866,.F.);
#25973=ADVANCED_FACE('',(#7149),#867,.T.);
#25974=ADVANCED_FACE('',(#7150),#868,.F.);
#25975=ADVANCED_FACE('',(#7151),#869,.F.);
#25976=ADVANCED_FACE('',(#7152),#870,.F.);
#25977=ADVANCED_FACE('',(#7153),#565,.F.);
#25978=ADVANCED_FACE('',(#7154),#566,.F.);
#25979=ADVANCED_FACE('',(#7155),#871,.F.);
#25980=ADVANCED_FACE('',(#7156),#872,.F.);
#25981=ADVANCED_FACE('',(#7157),#873,.F.);
#25982=ADVANCED_FACE('',(#7158),#874,.F.);
#25983=ADVANCED_FACE('',(#7159),#875,.F.);
#25984=ADVANCED_FACE('',(#7160),#876,.F.);
#25985=ADVANCED_FACE('',(#7161),#877,.T.);
#25986=ADVANCED_FACE('',(#7162),#6597,.F.);
#25987=ADVANCED_FACE('',(#7163),#6598,.F.);
#25988=ADVANCED_FACE('',(#7164),#6599,.F.);
#25989=ADVANCED_FACE('',(#7165),#6600,.F.);
#25990=ADVANCED_FACE('',(#7166,#646),#878,.F.);
#25991=ADVANCED_FACE('',(#7167),#6601,.T.);
#25992=ADVANCED_FACE('',(#7168),#879,.F.);
#25993=ADVANCED_FACE('',(#7169),#880,.F.);
#25994=ADVANCED_FACE('',(#7170),#881,.T.);
#25995=ADVANCED_FACE('',(#7171),#882,.T.);
#25996=ADVANCED_FACE('',(#7172),#341,.F.);
#25997=ADVANCED_FACE('',(#7173),#6602,.F.);
#25998=ADVANCED_FACE('',(#7174,#647),#883,.T.);
#25999=ADVANCED_FACE('',(#7175),#342,.F.);
#26000=ADVANCED_FACE('',(#7176,#648),#884,.F.);
#26001=ADVANCED_FACE('',(#7177),#343,.F.);
#26002=ADVANCED_FACE('',(#7178,#649,#650,#651),#885,.T.);
#26003=ADVANCED_FACE('',(#7179),#6603,.F.);
#26004=ADVANCED_FACE('',(#7180),#344,.F.);
#26005=ADVANCED_FACE('',(#7181),#6604,.F.);
#26006=ADVANCED_FACE('',(#7182),#345,.F.);
#26007=ADVANCED_FACE('',(#7183),#567,.T.);
#26008=ADVANCED_FACE('',(#7184,#652),#886,.F.);
#26009=ADVANCED_FACE('',(#7185),#6605,.F.);
#26010=ADVANCED_FACE('',(#7186),#346,.F.);
#26011=ADVANCED_FACE('',(#7187),#568,.T.);
#26012=ADVANCED_FACE('',(#7188),#6606,.F.);
#26013=ADVANCED_FACE('',(#7189),#6607,.F.);
#26014=ADVANCED_FACE('',(#7190),#347,.F.);
#26015=ADVANCED_FACE('',(#7191),#569,.T.);
#26016=ADVANCED_FACE('',(#7192),#6608,.F.);
#26017=ADVANCED_FACE('',(#7193),#348,.F.);
#26018=ADVANCED_FACE('',(#7194),#570,.T.);
#26019=ADVANCED_FACE('',(#7195),#6609,.F.);
#26020=ADVANCED_FACE('',(#7196),#349,.F.);
#26021=ADVANCED_FACE('',(#7197,#653,#654,#655,#656,#657),#887,.T.);
#26022=ADVANCED_FACE('',(#7198),#350,.F.);
#26023=ADVANCED_FACE('',(#7199),#351,.F.);
#26024=ADVANCED_FACE('',(#7200),#352,.F.);
#26025=ADVANCED_FACE('',(#7201),#353,.F.);
#26026=ADVANCED_FACE('',(#7202,#658,#659,#660,#661,#662),#888,.T.);
#26027=ADVANCED_FACE('',(#7203),#6610,.F.);
#26028=ADVANCED_FACE('',(#7204),#354,.F.);
#26029=ADVANCED_FACE('',(#7205),#6611,.F.);
#26030=ADVANCED_FACE('',(#7206),#355,.F.);
#26031=ADVANCED_FACE('',(#7207),#6612,.F.);
#26032=ADVANCED_FACE('',(#7208),#356,.F.);
#26033=ADVANCED_FACE('',(#7209),#6613,.F.);
#26034=ADVANCED_FACE('',(#7210),#357,.F.);
#26035=ADVANCED_FACE('',(#7211,#663,#664),#889,.F.);
#26036=ADVANCED_FACE('',(#7212),#358,.F.);
#26037=ADVANCED_FACE('',(#7213),#25619,.T.);
#26038=ADVANCED_FACE('',(#7214),#6614,.T.);
#26039=ADVANCED_FACE('',(#7215,#665,#666,#667,#668,#669),#890,.T.);
#26040=ADVANCED_FACE('',(#7216),#25620,.T.);
#26041=ADVANCED_FACE('',(#7217,#670,#671,#672,#673,#674),#891,.T.);
#26042=ADVANCED_FACE('',(#7218),#25621,.T.);
#26043=ADVANCED_FACE('',(#7219),#359,.T.);
#26044=ADVANCED_FACE('',(#7220),#360,.T.);
#26045=ADVANCED_FACE('',(#7221),#25622,.T.);
#26046=ADVANCED_FACE('',(#7222),#361,.T.);
#26047=ADVANCED_FACE('',(#7223),#25623,.T.);
#26048=ADVANCED_FACE('',(#7224),#892,.T.);
#26049=ADVANCED_FACE('',(#7225),#25624,.T.);
#26050=ADVANCED_FACE('',(#7226),#893,.T.);
#26051=ADVANCED_FACE('',(#7227),#25625,.T.);
#26052=ADVANCED_FACE('',(#7228),#894,.T.);
#26053=ADVANCED_FACE('',(#7229),#6615,.T.);
#26054=ADVANCED_FACE('',(#7230),#600,.F.);
#26055=ADVANCED_FACE('',(#7231),#6616,.T.);
#26056=ADVANCED_FACE('',(#7232),#601,.F.);
#26057=ADVANCED_FACE('',(#7233),#6617,.T.);
#26058=ADVANCED_FACE('',(#7234),#602,.F.);
#26059=ADVANCED_FACE('',(#7235),#6618,.T.);
#26060=ADVANCED_FACE('',(#7236),#603,.F.);
#26061=ADVANCED_FACE('',(#7237),#6619,.T.);
#26062=ADVANCED_FACE('',(#7238),#895,.T.);
#26063=ADVANCED_FACE('',(#7239),#6620,.T.);
#26064=ADVANCED_FACE('',(#7240),#896,.T.);
#26065=ADVANCED_FACE('',(#7241),#25626,.T.);
#26066=ADVANCED_FACE('',(#7242),#6621,.T.);
#26067=ADVANCED_FACE('',(#7243),#25627,.T.);
#26068=ADVANCED_FACE('',(#7244),#897,.F.);
#26069=ADVANCED_FACE('',(#7245),#898,.F.);
#26070=ADVANCED_FACE('',(#7246),#899,.F.);
#26071=ADVANCED_FACE('',(#7247),#900,.F.);
#26072=ADVANCED_FACE('',(#7248),#6622,.F.);
#26073=ADVANCED_FACE('',(#7249),#25628,.T.);
#26074=ADVANCED_FACE('',(#7250),#6623,.F.);
#26075=ADVANCED_FACE('',(#7251),#25629,.T.);
#26076=ADVANCED_FACE('',(#7252,#675),#901,.F.);
#26077=ADVANCED_FACE('',(#7253),#6624,.T.);
#26078=ADVANCED_FACE('',(#7254),#25630,.T.);
#26079=ADVANCED_FACE('',(#7255),#6625,.T.);
#26080=ADVANCED_FACE('',(#7256),#25631,.T.);
#26081=ADVANCED_FACE('',(#7257),#6626,.T.);
#26082=ADVANCED_FACE('',(#7258),#25632,.T.);
#26083=ADVANCED_FACE('',(#7259),#6627,.T.);
#26084=ADVANCED_FACE('',(#7260),#25633,.T.);
#26085=ADVANCED_FACE('',(#7261),#6628,.F.);
#26086=ADVANCED_FACE('',(#7262),#902,.F.);
#26087=ADVANCED_FACE('',(#7263),#6629,.F.);
#26088=ADVANCED_FACE('',(#7264),#903,.F.);
#26089=ADVANCED_FACE('',(#7265,#676),#904,.T.);
#26090=ADVANCED_FACE('',(#7266),#6630,.T.);
#26091=ADVANCED_FACE('',(#7267),#25634,.T.);
#26092=ADVANCED_FACE('',(#7268),#6631,.T.);
#26093=ADVANCED_FACE('',(#7269),#25635,.T.);
#26094=ADVANCED_FACE('',(#7270),#6632,.T.);
#26095=ADVANCED_FACE('',(#7271),#25636,.T.);
#26096=ADVANCED_FACE('',(#7272),#6633,.T.);
#26097=ADVANCED_FACE('',(#7273),#25637,.T.);
#26098=ADVANCED_FACE('',(#7274),#6634,.F.);
#26099=ADVANCED_FACE('',(#7275),#905,.F.);
#26100=ADVANCED_FACE('',(#7276),#6635,.F.);
#26101=ADVANCED_FACE('',(#7277,#677),#906,.F.);
#26102=ADVANCED_FACE('',(#7278),#6636,.T.);
#26103=ADVANCED_FACE('',(#7279),#25638,.T.);
#26104=ADVANCED_FACE('',(#7280),#6637,.T.);
#26105=ADVANCED_FACE('',(#7281),#25639,.T.);
#26106=ADVANCED_FACE('',(#7282),#6638,.T.);
#26107=ADVANCED_FACE('',(#7283),#25640,.T.);
#26108=ADVANCED_FACE('',(#7284),#6639,.T.);
#26109=ADVANCED_FACE('',(#7285),#25641,.T.);
#26110=ADVANCED_FACE('',(#7286),#6640,.T.);
#26111=ADVANCED_FACE('',(#7287),#907,.T.);
#26112=ADVANCED_FACE('',(#7288),#6641,.T.);
#26113=ADVANCED_FACE('',(#7289,#678),#908,.F.);
#26114=ADVANCED_FACE('',(#7290),#6642,.T.);
#26115=ADVANCED_FACE('',(#7291),#25642,.T.);
#26116=ADVANCED_FACE('',(#7292),#6643,.T.);
#26117=ADVANCED_FACE('',(#7293),#25643,.T.);
#26118=ADVANCED_FACE('',(#7294),#6644,.T.);
#26119=ADVANCED_FACE('',(#7295),#25644,.T.);
#26120=ADVANCED_FACE('',(#7296),#6645,.T.);
#26121=ADVANCED_FACE('',(#7297),#25645,.T.);
#26122=ADVANCED_FACE('',(#7298),#6646,.F.);
#26123=ADVANCED_FACE('',(#7299),#909,.F.);
#26124=ADVANCED_FACE('',(#7300),#6647,.F.);
#26125=ADVANCED_FACE('',(#7301),#910,.F.);
#26126=ADVANCED_FACE('',(#7302),#6648,.T.);
#26127=ADVANCED_FACE('',(#7303),#25646,.T.);
#26128=ADVANCED_FACE('',(#7304),#6649,.T.);
#26129=ADVANCED_FACE('',(#7305),#25647,.T.);
#26130=ADVANCED_FACE('',(#7306),#6650,.T.);
#26131=ADVANCED_FACE('',(#7307),#25648,.T.);
#26132=ADVANCED_FACE('',(#7308),#6651,.T.);
#26133=ADVANCED_FACE('',(#7309),#25649,.T.);
#26134=ADVANCED_FACE('',(#7310),#6652,.F.);
#26135=ADVANCED_FACE('',(#7311),#911,.F.);
#26136=ADVANCED_FACE('',(#7312),#6653,.F.);
#26137=ADVANCED_FACE('',(#7313),#912,.T.);
#26138=ADVANCED_FACE('',(#7314),#913,.T.);
#26139=ADVANCED_FACE('',(#7315),#914,.T.);
#26140=ADVANCED_FACE('',(#7316),#915,.T.);
#26141=ADVANCED_FACE('',(#7317),#6654,.F.);
#26142=ADVANCED_FACE('',(#7318),#6655,.F.);
#26143=ADVANCED_FACE('',(#7319),#6656,.F.);
#26144=ADVANCED_FACE('',(#7320),#6657,.F.);
#26145=ADVANCED_FACE('',(#7321),#916,.F.);
#26146=ADVANCED_FACE('',(#7322),#917,.F.);
#26147=ADVANCED_FACE('',(#7323,#679),#918,.F.);
#26148=ADVANCED_FACE('',(#7324),#6658,.F.);
#26149=ADVANCED_FACE('',(#7325,#680),#919,.F.);
#26150=ADVANCED_FACE('',(#7326),#6659,.F.);
#26151=ADVANCED_FACE('',(#7327),#6660,.F.);
#26152=ADVANCED_FACE('',(#7328),#920,.F.);
#26153=ADVANCED_FACE('',(#7329),#6661,.F.);
#26154=ADVANCED_FACE('',(#7330),#921,.F.);
#26155=ADVANCED_FACE('',(#7331),#6662,.F.);
#26156=ADVANCED_FACE('',(#7332),#922,.T.);
#26157=ADVANCED_FACE('',(#7333),#6663,.T.);
#26158=ADVANCED_FACE('',(#7334),#923,.T.);
#26159=ADVANCED_FACE('',(#7335),#6664,.T.);
#26160=ADVANCED_FACE('',(#7336),#924,.T.);
#26161=ADVANCED_FACE('',(#7337),#6665,.T.);
#26162=ADVANCED_FACE('',(#7338),#925,.T.);
#26163=ADVANCED_FACE('',(#7339),#6666,.T.);
#26164=ADVANCED_FACE('',(#7340),#926,.T.);
#26165=ADVANCED_FACE('',(#7341),#6667,.T.);
#26166=ADVANCED_FACE('',(#7342),#927,.T.);
#26167=ADVANCED_FACE('',(#7343),#6668,.T.);
#26168=ADVANCED_FACE('',(#7344),#928,.T.);
#26169=ADVANCED_FACE('',(#7345),#6669,.T.);
#26170=ADVANCED_FACE('',(#7346),#6670,.T.);
#26171=ADVANCED_FACE('',(#7347),#6671,.F.);
#26172=ADVANCED_FACE('',(#7348),#362,.T.);
#26173=ADVANCED_FACE('',(#7349),#929,.T.);
#26174=ADVANCED_FACE('',(#7350),#930,.F.);
#26175=ADVANCED_FACE('',(#7351),#6672,.T.);
#26176=ADVANCED_FACE('',(#7352),#931,.T.);
#26177=ADVANCED_FACE('',(#7353),#932,.T.);
#26178=ADVANCED_FACE('',(#7354),#933,.T.);
#26179=ADVANCED_FACE('',(#7355),#934,.F.);
#26180=ADVANCED_FACE('',(#7356),#935,.F.);
#26181=ADVANCED_FACE('',(#7357),#936,.F.);
#26182=ADVANCED_FACE('',(#7358),#937,.T.);
#26183=ADVANCED_FACE('',(#7359),#938,.T.);
#26184=ADVANCED_FACE('',(#7360),#939,.T.);
#26185=ADVANCED_FACE('',(#7361),#940,.F.);
#26186=ADVANCED_FACE('',(#7362),#941,.F.);
#26187=ADVANCED_FACE('',(#7363),#942,.F.);
#26188=ADVANCED_FACE('',(#7364),#943,.T.);
#26189=ADVANCED_FACE('',(#7365),#944,.T.);
#26190=ADVANCED_FACE('',(#7366),#945,.T.);
#26191=ADVANCED_FACE('',(#7367),#946,.F.);
#26192=ADVANCED_FACE('',(#7368),#947,.F.);
#26193=ADVANCED_FACE('',(#7369),#948,.F.);
#26194=ADVANCED_FACE('',(#7370),#949,.T.);
#26195=ADVANCED_FACE('',(#7371),#950,.T.);
#26196=ADVANCED_FACE('',(#7372),#951,.F.);
#26197=ADVANCED_FACE('',(#7373),#952,.F.);
#26198=ADVANCED_FACE('',(#7374),#953,.T.);
#26199=ADVANCED_FACE('',(#7375,#681),#954,.T.);
#26200=ADVANCED_FACE('',(#7376),#955,.T.);
#26201=ADVANCED_FACE('',(#7377),#956,.T.);
#26202=ADVANCED_FACE('',(#7378),#957,.T.);
#26203=ADVANCED_FACE('',(#7379),#958,.T.);
#26204=ADVANCED_FACE('',(#7380),#959,.T.);
#26205=ADVANCED_FACE('',(#7381),#960,.T.);
#26206=ADVANCED_FACE('',(#7382),#961,.T.);
#26207=ADVANCED_FACE('',(#7383),#962,.T.);
#26208=ADVANCED_FACE('',(#7384),#963,.T.);
#26209=ADVANCED_FACE('',(#7385),#964,.T.);
#26210=ADVANCED_FACE('',(#7386),#965,.T.);
#26211=ADVANCED_FACE('',(#7387),#966,.T.);
#26212=ADVANCED_FACE('',(#7388),#967,.T.);
#26213=ADVANCED_FACE('',(#7389),#968,.T.);
#26214=ADVANCED_FACE('',(#7390),#969,.T.);
#26215=ADVANCED_FACE('',(#7391),#970,.T.);
#26216=ADVANCED_FACE('',(#7392),#971,.T.);
#26217=ADVANCED_FACE('',(#7393),#972,.T.);
#26218=ADVANCED_FACE('',(#7394),#973,.T.);
#26219=ADVANCED_FACE('',(#7395),#974,.F.);
#26220=ADVANCED_FACE('',(#7396),#975,.T.);
#26221=ADVANCED_FACE('',(#7397),#976,.T.);
#26222=ADVANCED_FACE('',(#7398),#977,.T.);
#26223=ADVANCED_FACE('',(#7399),#978,.T.);
#26224=ADVANCED_FACE('',(#7400),#979,.F.);
#26225=ADVANCED_FACE('',(#7401),#980,.F.);
#26226=ADVANCED_FACE('',(#7402),#981,.F.);
#26227=ADVANCED_FACE('',(#7403),#982,.T.);
#26228=ADVANCED_FACE('',(#7404),#983,.T.);
#26229=ADVANCED_FACE('',(#7405),#984,.T.);
#26230=ADVANCED_FACE('',(#7406),#985,.F.);
#26231=ADVANCED_FACE('',(#7407),#986,.F.);
#26232=ADVANCED_FACE('',(#7408),#987,.F.);
#26233=ADVANCED_FACE('',(#7409),#988,.T.);
#26234=ADVANCED_FACE('',(#7410),#989,.T.);
#26235=ADVANCED_FACE('',(#7411),#990,.T.);
#26236=ADVANCED_FACE('',(#7412),#991,.F.);
#26237=ADVANCED_FACE('',(#7413),#992,.F.);
#26238=ADVANCED_FACE('',(#7414),#993,.F.);
#26239=ADVANCED_FACE('',(#7415),#994,.T.);
#26240=ADVANCED_FACE('',(#7416),#995,.T.);
#26241=ADVANCED_FACE('',(#7417),#996,.T.);
#26242=ADVANCED_FACE('',(#7418),#997,.F.);
#26243=ADVANCED_FACE('',(#7419),#998,.F.);
#26244=ADVANCED_FACE('',(#7420),#999,.F.);
#26245=ADVANCED_FACE('',(#7421),#1000,.T.);
#26246=ADVANCED_FACE('',(#7422),#1001,.T.);
#26247=ADVANCED_FACE('',(#7423),#1002,.T.);
#26248=ADVANCED_FACE('',(#7424),#1003,.F.);
#26249=ADVANCED_FACE('',(#7425),#1004,.F.);
#26250=ADVANCED_FACE('',(#7426),#1005,.F.);
#26251=ADVANCED_FACE('',(#7427),#1006,.T.);
#26252=ADVANCED_FACE('',(#7428),#1007,.T.);
#26253=ADVANCED_FACE('',(#7429),#1008,.T.);
#26254=ADVANCED_FACE('',(#7430),#1009,.F.);
#26255=ADVANCED_FACE('',(#7431),#1010,.F.);
#26256=ADVANCED_FACE('',(#7432),#1011,.F.);
#26257=ADVANCED_FACE('',(#7433),#1012,.T.);
#26258=ADVANCED_FACE('',(#7434),#1013,.F.);
#26259=ADVANCED_FACE('',(#7435),#1014,.T.);
#26260=ADVANCED_FACE('',(#7436),#1015,.T.);
#26261=ADVANCED_FACE('',(#7437),#1016,.F.);
#26262=ADVANCED_FACE('',(#7438),#1017,.F.);
#26263=ADVANCED_FACE('',(#7439),#1018,.T.);
#26264=ADVANCED_FACE('',(#7440),#1019,.T.);
#26265=ADVANCED_FACE('',(#7441),#1020,.T.);
#26266=ADVANCED_FACE('',(#7442),#1021,.F.);
#26267=ADVANCED_FACE('',(#7443),#1022,.F.);
#26268=ADVANCED_FACE('',(#7444),#1023,.F.);
#26269=ADVANCED_FACE('',(#7445),#1024,.T.);
#26270=ADVANCED_FACE('',(#7446),#1025,.T.);
#26271=ADVANCED_FACE('',(#7447),#1026,.T.);
#26272=ADVANCED_FACE('',(#7448),#1027,.F.);
#26273=ADVANCED_FACE('',(#7449),#1028,.F.);
#26274=ADVANCED_FACE('',(#7450),#1029,.F.);
#26275=ADVANCED_FACE('',(#7451),#1030,.T.);
#26276=ADVANCED_FACE('',(#7452),#1031,.T.);
#26277=ADVANCED_FACE('',(#7453),#1032,.T.);
#26278=ADVANCED_FACE('',(#7454),#1033,.F.);
#26279=ADVANCED_FACE('',(#7455),#1034,.F.);
#26280=ADVANCED_FACE('',(#7456),#1035,.F.);
#26281=ADVANCED_FACE('',(#7457),#1036,.T.);
#26282=ADVANCED_FACE('',(#7458),#1037,.T.);
#26283=ADVANCED_FACE('',(#7459),#1038,.T.);
#26284=ADVANCED_FACE('',(#7460),#1039,.F.);
#26285=ADVANCED_FACE('',(#7461),#1040,.F.);
#26286=ADVANCED_FACE('',(#7462),#1041,.F.);
#26287=ADVANCED_FACE('',(#7463),#1042,.T.);
#26288=ADVANCED_FACE('',(#7464),#1043,.T.);
#26289=ADVANCED_FACE('',(#7465),#1044,.T.);
#26290=ADVANCED_FACE('',(#7466),#1045,.F.);
#26291=ADVANCED_FACE('',(#7467),#1046,.F.);
#26292=ADVANCED_FACE('',(#7468),#1047,.F.);
#26293=ADVANCED_FACE('',(#7469),#1048,.T.);
#26294=ADVANCED_FACE('',(#7470),#1049,.T.);
#26295=ADVANCED_FACE('',(#7471),#1050,.T.);
#26296=ADVANCED_FACE('',(#7472),#1051,.F.);
#26297=ADVANCED_FACE('',(#7473),#1052,.F.);
#26298=ADVANCED_FACE('',(#7474),#1053,.F.);
#26299=ADVANCED_FACE('',(#7475),#1054,.T.);
#26300=ADVANCED_FACE('',(#7476),#1055,.T.);
#26301=ADVANCED_FACE('',(#7477),#1056,.T.);
#26302=ADVANCED_FACE('',(#7478),#1057,.F.);
#26303=ADVANCED_FACE('',(#7479),#1058,.F.);
#26304=ADVANCED_FACE('',(#7480),#1059,.F.);
#26305=ADVANCED_FACE('',(#7481),#1060,.T.);
#26306=ADVANCED_FACE('',(#7482),#1061,.T.);
#26307=ADVANCED_FACE('',(#7483),#1062,.T.);
#26308=ADVANCED_FACE('',(#7484),#1063,.F.);
#26309=ADVANCED_FACE('',(#7485),#1064,.F.);
#26310=ADVANCED_FACE('',(#7486),#1065,.F.);
#26311=ADVANCED_FACE('',(#7487),#1066,.T.);
#26312=ADVANCED_FACE('',(#7488),#1067,.T.);
#26313=ADVANCED_FACE('',(#7489),#1068,.T.);
#26314=ADVANCED_FACE('',(#7490),#1069,.F.);
#26315=ADVANCED_FACE('',(#7491),#1070,.F.);
#26316=ADVANCED_FACE('',(#7492),#1071,.F.);
#26317=ADVANCED_FACE('',(#7493),#1072,.T.);
#26318=ADVANCED_FACE('',(#7494),#1073,.T.);
#26319=ADVANCED_FACE('',(#7495),#1074,.T.);
#26320=ADVANCED_FACE('',(#7496),#1075,.F.);
#26321=ADVANCED_FACE('',(#7497),#1076,.F.);
#26322=ADVANCED_FACE('',(#7498),#1077,.F.);
#26323=ADVANCED_FACE('',(#7499),#1078,.T.);
#26324=ADVANCED_FACE('',(#7500),#1079,.T.);
#26325=ADVANCED_FACE('',(#7501),#1080,.T.);
#26326=ADVANCED_FACE('',(#7502),#1081,.F.);
#26327=ADVANCED_FACE('',(#7503),#1082,.F.);
#26328=ADVANCED_FACE('',(#7504),#1083,.F.);
#26329=ADVANCED_FACE('',(#7505),#1084,.T.);
#26330=ADVANCED_FACE('',(#7506),#1085,.T.);
#26331=ADVANCED_FACE('',(#7507),#1086,.T.);
#26332=ADVANCED_FACE('',(#7508),#1087,.F.);
#26333=ADVANCED_FACE('',(#7509),#1088,.F.);
#26334=ADVANCED_FACE('',(#7510),#1089,.F.);
#26335=ADVANCED_FACE('',(#7511),#1090,.T.);
#26336=ADVANCED_FACE('',(#7512),#1091,.T.);
#26337=ADVANCED_FACE('',(#7513,#682),#1092,.T.);
#26338=ADVANCED_FACE('',(#7514),#1093,.T.);
#26339=ADVANCED_FACE('',(#7515),#1094,.T.);
#26340=ADVANCED_FACE('',(#7516),#1095,.T.);
#26341=ADVANCED_FACE('',(#7517),#1096,.T.);
#26342=ADVANCED_FACE('',(#7518),#1097,.T.);
#26343=ADVANCED_FACE('',(#7519),#1098,.T.);
#26344=ADVANCED_FACE('',(#7520),#1099,.T.);
#26345=ADVANCED_FACE('',(#7521),#1100,.F.);
#26346=ADVANCED_FACE('',(#7522),#1101,.F.);
#26347=ADVANCED_FACE('',(#7523),#1102,.T.);
#26348=ADVANCED_FACE('',(#7524),#1103,.T.);
#26349=ADVANCED_FACE('',(#7525),#1104,.T.);
#26350=ADVANCED_FACE('',(#7526),#1105,.T.);
#26351=ADVANCED_FACE('',(#7527),#1106,.T.);
#26352=ADVANCED_FACE('',(#7528),#1107,.T.);
#26353=ADVANCED_FACE('',(#7529),#1108,.F.);
#26354=ADVANCED_FACE('',(#7530),#1109,.F.);
#26355=ADVANCED_FACE('',(#7531),#1110,.T.);
#26356=ADVANCED_FACE('',(#7532),#1111,.T.);
#26357=ADVANCED_FACE('',(#7533),#1112,.T.);
#26358=ADVANCED_FACE('',(#7534),#1113,.T.);
#26359=ADVANCED_FACE('',(#7535),#1114,.T.);
#26360=ADVANCED_FACE('',(#7536),#1115,.T.);
#26361=ADVANCED_FACE('',(#7537),#1116,.F.);
#26362=ADVANCED_FACE('',(#7538),#1117,.F.);
#26363=ADVANCED_FACE('',(#7539),#1118,.T.);
#26364=ADVANCED_FACE('',(#7540),#1119,.T.);
#26365=ADVANCED_FACE('',(#7541),#1120,.T.);
#26366=ADVANCED_FACE('',(#7542),#1121,.T.);
#26367=ADVANCED_FACE('',(#7543),#1122,.T.);
#26368=ADVANCED_FACE('',(#7544),#1123,.T.);
#26369=ADVANCED_FACE('',(#7545),#1124,.T.);
#26370=ADVANCED_FACE('',(#7546),#1125,.T.);
#26371=ADVANCED_FACE('',(#7547),#1126,.T.);
#26372=ADVANCED_FACE('',(#7548),#1127,.F.);
#26373=ADVANCED_FACE('',(#7549),#1128,.F.);
#26374=ADVANCED_FACE('',(#7550),#1129,.T.);
#26375=ADVANCED_FACE('',(#7551),#1130,.T.);
#26376=ADVANCED_FACE('',(#7552),#1131,.T.);
#26377=ADVANCED_FACE('',(#7553),#1132,.T.);
#26378=ADVANCED_FACE('',(#7554),#1133,.T.);
#26379=ADVANCED_FACE('',(#7555),#1134,.T.);
#26380=ADVANCED_FACE('',(#7556),#1135,.F.);
#26381=ADVANCED_FACE('',(#7557),#1136,.F.);
#26382=ADVANCED_FACE('',(#7558),#1137,.T.);
#26383=ADVANCED_FACE('',(#7559),#1138,.T.);
#26384=ADVANCED_FACE('',(#7560),#1139,.T.);
#26385=ADVANCED_FACE('',(#7561),#1140,.T.);
#26386=ADVANCED_FACE('',(#7562),#1141,.T.);
#26387=ADVANCED_FACE('',(#7563),#1142,.T.);
#26388=ADVANCED_FACE('',(#7564),#1143,.F.);
#26389=ADVANCED_FACE('',(#7565),#1144,.F.);
#26390=ADVANCED_FACE('',(#7566),#1145,.T.);
#26391=ADVANCED_FACE('',(#7567),#1146,.T.);
#26392=ADVANCED_FACE('',(#7568),#1147,.T.);
#26393=ADVANCED_FACE('',(#7569),#1148,.T.);
#26394=ADVANCED_FACE('',(#7570),#1149,.T.);
#26395=ADVANCED_FACE('',(#7571),#1150,.T.);
#26396=ADVANCED_FACE('',(#7572),#1151,.F.);
#26397=ADVANCED_FACE('',(#7573),#1152,.F.);
#26398=ADVANCED_FACE('',(#7574),#1153,.T.);
#26399=ADVANCED_FACE('',(#7575),#1154,.T.);
#26400=ADVANCED_FACE('',(#7576),#1155,.T.);
#26401=ADVANCED_FACE('',(#7577),#1156,.T.);
#26402=ADVANCED_FACE('',(#7578),#1157,.T.);
#26403=ADVANCED_FACE('',(#7579),#1158,.T.);
#26404=ADVANCED_FACE('',(#7580),#1159,.F.);
#26405=ADVANCED_FACE('',(#7581),#1160,.F.);
#26406=ADVANCED_FACE('',(#7582),#1161,.T.);
#26407=ADVANCED_FACE('',(#7583),#1162,.T.);
#26408=ADVANCED_FACE('',(#7584),#1163,.T.);
#26409=ADVANCED_FACE('',(#7585),#1164,.T.);
#26410=ADVANCED_FACE('',(#7586),#1165,.T.);
#26411=ADVANCED_FACE('',(#7587),#1166,.T.);
#26412=ADVANCED_FACE('',(#7588),#1167,.F.);
#26413=ADVANCED_FACE('',(#7589),#1168,.F.);
#26414=ADVANCED_FACE('',(#7590),#1169,.T.);
#26415=ADVANCED_FACE('',(#7591),#1170,.T.);
#26416=ADVANCED_FACE('',(#7592),#1171,.T.);
#26417=ADVANCED_FACE('',(#7593),#1172,.T.);
#26418=ADVANCED_FACE('',(#7594),#1173,.T.);
#26419=ADVANCED_FACE('',(#7595),#1174,.T.);
#26420=ADVANCED_FACE('',(#7596),#1175,.T.);
#26421=ADVANCED_FACE('',(#7597),#1176,.T.);
#26422=ADVANCED_FACE('',(#7598),#1177,.T.);
#26423=ADVANCED_FACE('',(#7599),#1178,.F.);
#26424=ADVANCED_FACE('',(#7600),#1179,.F.);
#26425=ADVANCED_FACE('',(#7601),#1180,.T.);
#26426=ADVANCED_FACE('',(#7602),#1181,.T.);
#26427=ADVANCED_FACE('',(#7603),#1182,.T.);
#26428=ADVANCED_FACE('',(#7604),#1183,.T.);
#26429=ADVANCED_FACE('',(#7605),#1184,.T.);
#26430=ADVANCED_FACE('',(#7606),#1185,.T.);
#26431=ADVANCED_FACE('',(#7607),#1186,.F.);
#26432=ADVANCED_FACE('',(#7608),#1187,.F.);
#26433=ADVANCED_FACE('',(#7609),#1188,.T.);
#26434=ADVANCED_FACE('',(#7610),#1189,.T.);
#26435=ADVANCED_FACE('',(#7611),#1190,.T.);
#26436=ADVANCED_FACE('',(#7612),#1191,.T.);
#26437=ADVANCED_FACE('',(#7613),#1192,.T.);
#26438=ADVANCED_FACE('',(#7614),#1193,.T.);
#26439=ADVANCED_FACE('',(#7615),#1194,.F.);
#26440=ADVANCED_FACE('',(#7616),#1195,.F.);
#26441=ADVANCED_FACE('',(#7617),#1196,.T.);
#26442=ADVANCED_FACE('',(#7618),#1197,.T.);
#26443=ADVANCED_FACE('',(#7619),#1198,.T.);
#26444=ADVANCED_FACE('',(#7620),#1199,.T.);
#26445=ADVANCED_FACE('',(#7621),#1200,.T.);
#26446=ADVANCED_FACE('',(#7622),#1201,.T.);
#26447=ADVANCED_FACE('',(#7623),#1202,.T.);
#26448=ADVANCED_FACE('',(#7624),#1203,.T.);
#26449=ADVANCED_FACE('',(#7625),#1204,.T.);
#26450=ADVANCED_FACE('',(#7626),#1205,.F.);
#26451=ADVANCED_FACE('',(#7627),#1206,.F.);
#26452=ADVANCED_FACE('',(#7628),#1207,.T.);
#26453=ADVANCED_FACE('',(#7629),#1208,.T.);
#26454=ADVANCED_FACE('',(#7630),#1209,.T.);
#26455=ADVANCED_FACE('',(#7631),#1210,.F.);
#26456=ADVANCED_FACE('',(#7632),#1211,.F.);
#26457=ADVANCED_FACE('',(#7633),#1212,.F.);
#26458=ADVANCED_FACE('',(#7634),#6673,.F.);
#26459=ADVANCED_FACE('',(#7635),#1213,.T.);
#26460=ADVANCED_FACE('',(#7636),#1214,.T.);
#26461=ADVANCED_FACE('',(#7637),#1215,.T.);
#26462=ADVANCED_FACE('',(#7638),#1216,.T.);
#26463=ADVANCED_FACE('',(#7639),#1217,.T.);
#26464=ADVANCED_FACE('',(#7640),#1218,.T.);
#26465=ADVANCED_FACE('',(#7641),#1219,.F.);
#26466=ADVANCED_FACE('',(#7642),#1220,.F.);
#26467=ADVANCED_FACE('',(#7643),#1221,.F.);
#26468=ADVANCED_FACE('',(#7644),#1222,.T.);
#26469=ADVANCED_FACE('',(#7645),#1223,.T.);
#26470=ADVANCED_FACE('',(#7646),#1224,.T.);
#26471=ADVANCED_FACE('',(#7647),#1225,.F.);
#26472=ADVANCED_FACE('',(#7648),#1226,.F.);
#26473=ADVANCED_FACE('',(#7649),#1227,.F.);
#26474=ADVANCED_FACE('',(#7650),#1228,.F.);
#26475=ADVANCED_FACE('',(#7651),#1229,.F.);
#26476=ADVANCED_FACE('',(#7652),#1230,.F.);
#26477=ADVANCED_FACE('',(#7653),#1231,.F.);
#26478=ADVANCED_FACE('',(#7654),#1232,.F.);
#26479=ADVANCED_FACE('',(#7655),#1233,.F.);
#26480=ADVANCED_FACE('',(#7656),#1234,.F.);
#26481=ADVANCED_FACE('',(#7657),#1235,.F.);
#26482=ADVANCED_FACE('',(#7658),#1236,.F.);
#26483=ADVANCED_FACE('',(#7659),#1237,.F.);
#26484=ADVANCED_FACE('',(#7660),#1238,.F.);
#26485=ADVANCED_FACE('',(#7661),#1239,.F.);
#26486=ADVANCED_FACE('',(#7662),#1240,.F.);
#26487=ADVANCED_FACE('',(#7663),#1241,.F.);
#26488=ADVANCED_FACE('',(#7664),#1242,.F.);
#26489=ADVANCED_FACE('',(#7665),#1243,.F.);
#26490=ADVANCED_FACE('',(#7666),#1244,.F.);
#26491=ADVANCED_FACE('',(#7667),#1245,.F.);
#26492=ADVANCED_FACE('',(#7668),#1246,.F.);
#26493=ADVANCED_FACE('',(#7669),#1247,.F.);
#26494=ADVANCED_FACE('',(#7670),#1248,.F.);
#26495=ADVANCED_FACE('',(#7671),#1249,.F.);
#26496=ADVANCED_FACE('',(#7672),#1250,.F.);
#26497=ADVANCED_FACE('',(#7673),#1251,.F.);
#26498=ADVANCED_FACE('',(#7674),#1252,.F.);
#26499=ADVANCED_FACE('',(#7675),#1253,.F.);
#26500=ADVANCED_FACE('',(#7676),#1254,.F.);
#26501=ADVANCED_FACE('',(#7677),#1255,.F.);
#26502=ADVANCED_FACE('',(#7678),#1256,.F.);
#26503=ADVANCED_FACE('',(#7679),#1257,.F.);
#26504=ADVANCED_FACE('',(#7680),#1258,.F.);
#26505=ADVANCED_FACE('',(#7681),#1259,.F.);
#26506=ADVANCED_FACE('',(#7682),#1260,.F.);
#26507=ADVANCED_FACE('',(#7683),#1261,.F.);
#26508=ADVANCED_FACE('',(#7684),#1262,.F.);
#26509=ADVANCED_FACE('',(#7685),#1263,.F.);
#26510=ADVANCED_FACE('',(#7686),#1264,.F.);
#26511=ADVANCED_FACE('',(#7687),#1265,.F.);
#26512=ADVANCED_FACE('',(#7688),#1266,.F.);
#26513=ADVANCED_FACE('',(#7689),#1267,.F.);
#26514=ADVANCED_FACE('',(#7690),#1268,.F.);
#26515=ADVANCED_FACE('',(#7691),#1269,.F.);
#26516=ADVANCED_FACE('',(#7692),#1270,.F.);
#26517=ADVANCED_FACE('',(#7693),#1271,.F.);
#26518=ADVANCED_FACE('',(#7694),#1272,.F.);
#26519=ADVANCED_FACE('',(#7695),#1273,.F.);
#26520=ADVANCED_FACE('',(#7696),#1274,.F.);
#26521=ADVANCED_FACE('',(#7697),#1275,.F.);
#26522=ADVANCED_FACE('',(#7698),#1276,.F.);
#26523=ADVANCED_FACE('',(#7699),#1277,.F.);
#26524=ADVANCED_FACE('',(#7700),#1278,.F.);
#26525=ADVANCED_FACE('',(#7701),#1279,.F.);
#26526=ADVANCED_FACE('',(#7702),#1280,.F.);
#26527=ADVANCED_FACE('',(#7703),#1281,.F.);
#26528=ADVANCED_FACE('',(#7704),#1282,.F.);
#26529=ADVANCED_FACE('',(#7705),#1283,.F.);
#26530=ADVANCED_FACE('',(#7706),#1284,.F.);
#26531=ADVANCED_FACE('',(#7707),#1285,.F.);
#26532=ADVANCED_FACE('',(#7708),#1286,.F.);
#26533=ADVANCED_FACE('',(#7709),#1287,.F.);
#26534=ADVANCED_FACE('',(#7710),#1288,.F.);
#26535=ADVANCED_FACE('',(#7711),#1289,.F.);
#26536=ADVANCED_FACE('',(#7712),#1290,.F.);
#26537=ADVANCED_FACE('',(#7713),#1291,.F.);
#26538=ADVANCED_FACE('',(#7714),#1292,.F.);
#26539=ADVANCED_FACE('',(#7715),#1293,.F.);
#26540=ADVANCED_FACE('',(#7716),#1294,.F.);
#26541=ADVANCED_FACE('',(#7717),#1295,.F.);
#26542=ADVANCED_FACE('',(#7718),#1296,.F.);
#26543=ADVANCED_FACE('',(#7719),#1297,.F.);
#26544=ADVANCED_FACE('',(#7720),#1298,.F.);
#26545=ADVANCED_FACE('',(#7721),#1299,.F.);
#26546=ADVANCED_FACE('',(#7722),#1300,.F.);
#26547=ADVANCED_FACE('',(#7723),#1301,.F.);
#26548=ADVANCED_FACE('',(#7724),#1302,.F.);
#26549=ADVANCED_FACE('',(#7725),#1303,.F.);
#26550=ADVANCED_FACE('',(#7726),#1304,.F.);
#26551=ADVANCED_FACE('',(#7727),#1305,.F.);
#26552=ADVANCED_FACE('',(#7728),#1306,.F.);
#26553=ADVANCED_FACE('',(#7729),#1307,.F.);
#26554=ADVANCED_FACE('',(#7730),#1308,.F.);
#26555=ADVANCED_FACE('',(#7731),#1309,.F.);
#26556=ADVANCED_FACE('',(#7732),#1310,.F.);
#26557=ADVANCED_FACE('',(#7733),#1311,.F.);
#26558=ADVANCED_FACE('',(#7734),#1312,.F.);
#26559=ADVANCED_FACE('',(#7735),#1313,.F.);
#26560=ADVANCED_FACE('',(#7736),#1314,.F.);
#26561=ADVANCED_FACE('',(#7737),#1315,.F.);
#26562=ADVANCED_FACE('',(#7738),#1316,.F.);
#26563=ADVANCED_FACE('',(#7739),#1317,.F.);
#26564=ADVANCED_FACE('',(#7740),#1318,.F.);
#26565=ADVANCED_FACE('',(#7741),#1319,.F.);
#26566=ADVANCED_FACE('',(#7742),#1320,.F.);
#26567=ADVANCED_FACE('',(#7743),#1321,.F.);
#26568=ADVANCED_FACE('',(#7744),#1322,.F.);
#26569=ADVANCED_FACE('',(#7745),#1323,.F.);
#26570=ADVANCED_FACE('',(#7746),#1324,.F.);
#26571=ADVANCED_FACE('',(#7747),#1325,.F.);
#26572=ADVANCED_FACE('',(#7748),#1326,.F.);
#26573=ADVANCED_FACE('',(#7749),#1327,.F.);
#26574=ADVANCED_FACE('',(#7750),#1328,.F.);
#26575=ADVANCED_FACE('',(#7751),#1329,.F.);
#26576=ADVANCED_FACE('',(#7752),#1330,.F.);
#26577=ADVANCED_FACE('',(#7753),#1331,.F.);
#26578=ADVANCED_FACE('',(#7754),#1332,.F.);
#26579=ADVANCED_FACE('',(#7755),#1333,.F.);
#26580=ADVANCED_FACE('',(#7756),#1334,.F.);
#26581=ADVANCED_FACE('',(#7757),#1335,.F.);
#26582=ADVANCED_FACE('',(#7758),#1336,.F.);
#26583=ADVANCED_FACE('',(#7759),#1337,.F.);
#26584=ADVANCED_FACE('',(#7760),#1338,.F.);
#26585=ADVANCED_FACE('',(#7761),#1339,.F.);
#26586=ADVANCED_FACE('',(#7762),#1340,.F.);
#26587=ADVANCED_FACE('',(#7763),#1341,.F.);
#26588=ADVANCED_FACE('',(#7764),#1342,.F.);
#26589=ADVANCED_FACE('',(#7765),#1343,.F.);
#26590=ADVANCED_FACE('',(#7766),#1344,.F.);
#26591=ADVANCED_FACE('',(#7767),#1345,.F.);
#26592=ADVANCED_FACE('',(#7768),#1346,.F.);
#26593=ADVANCED_FACE('',(#7769),#1347,.F.);
#26594=ADVANCED_FACE('',(#7770),#1348,.F.);
#26595=ADVANCED_FACE('',(#7771),#1349,.F.);
#26596=ADVANCED_FACE('',(#7772),#1350,.F.);
#26597=ADVANCED_FACE('',(#7773),#1351,.F.);
#26598=ADVANCED_FACE('',(#7774),#1352,.F.);
#26599=ADVANCED_FACE('',(#7775),#1353,.F.);
#26600=ADVANCED_FACE('',(#7776),#1354,.F.);
#26601=ADVANCED_FACE('',(#7777),#1355,.F.);
#26602=ADVANCED_FACE('',(#7778),#1356,.F.);
#26603=ADVANCED_FACE('',(#7779),#1357,.F.);
#26604=ADVANCED_FACE('',(#7780),#1358,.F.);
#26605=ADVANCED_FACE('',(#7781),#1359,.F.);
#26606=ADVANCED_FACE('',(#7782),#1360,.F.);
#26607=ADVANCED_FACE('',(#7783),#1361,.F.);
#26608=ADVANCED_FACE('',(#7784),#1362,.F.);
#26609=ADVANCED_FACE('',(#7785),#1363,.F.);
#26610=ADVANCED_FACE('',(#7786),#1364,.F.);
#26611=ADVANCED_FACE('',(#7787),#1365,.F.);
#26612=ADVANCED_FACE('',(#7788),#1366,.F.);
#26613=ADVANCED_FACE('',(#7789),#1367,.F.);
#26614=ADVANCED_FACE('',(#7790),#1368,.F.);
#26615=ADVANCED_FACE('',(#7791),#6674,.F.);
#26616=ADVANCED_FACE('',(#7792),#1369,.F.);
#26617=ADVANCED_FACE('',(#7793),#1370,.F.);
#26618=ADVANCED_FACE('',(#7794),#1371,.F.);
#26619=ADVANCED_FACE('',(#7795),#1372,.F.);
#26620=ADVANCED_FACE('',(#7796),#1373,.F.);
#26621=ADVANCED_FACE('',(#7797),#6675,.F.);
#26622=ADVANCED_FACE('',(#7798),#1374,.T.);
#26623=ADVANCED_FACE('',(#7799),#363,.T.);
#26624=ADVANCED_FACE('',(#7800,#683),#6676,.T.);
#26625=ADVANCED_FACE('',(#7801),#364,.T.);
#26626=ADVANCED_FACE('',(#7802),#6677,.T.);
#26627=ADVANCED_FACE('',(#7803,#684),#1375,.T.);
#26628=ADVANCED_FACE('',(#7804),#6678,.T.);
#26629=ADVANCED_FACE('',(#7805,#685),#1376,.T.);
#26630=ADVANCED_FACE('',(#7806),#6679,.T.);
#26631=ADVANCED_FACE('',(#7807,#686),#1377,.T.);
#26632=ADVANCED_FACE('',(#7808),#6680,.T.);
#26633=ADVANCED_FACE('',(#7809,#687),#1378,.T.);
#26634=ADVANCED_FACE('',(#7810),#6681,.T.);
#26635=ADVANCED_FACE('',(#7811,#688),#1379,.T.);
#26636=ADVANCED_FACE('',(#7812,#689),#6682,.T.);
#26637=ADVANCED_FACE('',(#7813),#365,.T.);
#26638=ADVANCED_FACE('',(#7814),#1380,.T.);
#26639=ADVANCED_FACE('',(#7815),#366,.T.);
#26640=ADVANCED_FACE('',(#7816,#690),#1381,.T.);
#26641=ADVANCED_FACE('',(#7817),#367,.F.);
#26642=ADVANCED_FACE('',(#7818,#691),#1382,.T.);
#26643=ADVANCED_FACE('',(#7819),#368,.T.);
#26644=ADVANCED_FACE('',(#7820),#6683,.T.);
#26645=ADVANCED_FACE('',(#7821),#369,.T.);
#26646=ADVANCED_FACE('',(#7822,#692),#1383,.T.);
#26647=ADVANCED_FACE('',(#7823),#370,.F.);
#26648=ADVANCED_FACE('',(#7824,#693),#1384,.T.);
#26649=ADVANCED_FACE('',(#7825),#371,.T.);
#26650=ADVANCED_FACE('',(#7826,#694),#1385,.T.);
#26651=ADVANCED_FACE('',(#7827),#372,.F.);
#26652=ADVANCED_FACE('',(#7828),#6684,.F.);
#26653=ADVANCED_FACE('',(#7829),#373,.F.);
#26654=ADVANCED_FACE('',(#7830,#695),#1386,.T.);
#26655=ADVANCED_FACE('',(#7831),#374,.T.);
#26656=ADVANCED_FACE('',(#7832),#6685,.T.);
#26657=ADVANCED_FACE('',(#7833,#696),#1387,.T.);
#26658=ADVANCED_FACE('',(#7834),#6686,.F.);
#26659=ADVANCED_FACE('',(#7835,#697),#1388,.T.);
#26660=ADVANCED_FACE('',(#7836),#375,.T.);
#26661=ADVANCED_FACE('',(#7837),#6687,.T.);
#26662=ADVANCED_FACE('',(#7838,#698),#1389,.T.);
#26663=ADVANCED_FACE('',(#7839),#6688,.F.);
#26664=ADVANCED_FACE('',(#7840,#699),#1390,.T.);
#26665=ADVANCED_FACE('',(#7841),#6689,.F.);
#26666=ADVANCED_FACE('',(#7842,#700),#1391,.T.);
#26667=ADVANCED_FACE('',(#7843),#376,.T.);
#26668=ADVANCED_FACE('',(#7844),#6690,.T.);
#26669=ADVANCED_FACE('',(#7845,#701),#1392,.T.);
#26670=ADVANCED_FACE('',(#7846),#1393,.T.);
#26671=ADVANCED_FACE('',(#7847),#377,.T.);
#26672=ADVANCED_FACE('',(#7848),#6691,.T.);
#26673=ADVANCED_FACE('',(#7849),#378,.T.);
#26674=ADVANCED_FACE('',(#7850),#1394,.T.);
#26675=ADVANCED_FACE('',(#7851),#6692,.F.);
#26676=ADVANCED_FACE('',(#7852,#702),#1395,.T.);
#26677=ADVANCED_FACE('',(#7853),#6693,.T.);
#26678=ADVANCED_FACE('',(#7854,#703),#1396,.T.);
#26679=ADVANCED_FACE('',(#7855),#25650,.T.);
#26680=ADVANCED_FACE('',(#7856),#1397,.T.);
#26681=ADVANCED_FACE('',(#7857),#379,.T.);
#26682=ADVANCED_FACE('',(#7858),#1398,.T.);
#26683=ADVANCED_FACE('',(#7859),#1399,.T.);
#26684=ADVANCED_FACE('',(#7860),#1400,.T.);
#26685=ADVANCED_FACE('',(#7861),#1401,.T.);
#26686=ADVANCED_FACE('',(#7862),#380,.T.);
#26687=ADVANCED_FACE('',(#7863),#1402,.F.);
#26688=ADVANCED_FACE('',(#7864),#1403,.T.);
#26689=ADVANCED_FACE('',(#7865),#6694,.T.);
#26690=ADVANCED_FACE('',(#7866),#6695,.F.);
#26691=ADVANCED_FACE('',(#7867),#1404,.T.);
#26692=ADVANCED_FACE('',(#7868),#1405,.T.);
#26693=ADVANCED_FACE('',(#7869),#1406,.T.);
#26694=ADVANCED_FACE('',(#7870),#1407,.T.);
#26695=ADVANCED_FACE('',(#7871),#1408,.T.);
#26696=ADVANCED_FACE('',(#7872),#1409,.T.);
#26697=ADVANCED_FACE('',(#7873),#381,.F.);
#26698=ADVANCED_FACE('',(#7874),#1410,.T.);
#26699=ADVANCED_FACE('',(#7875),#1411,.T.);
#26700=ADVANCED_FACE('',(#7876),#1412,.T.);
#26701=ADVANCED_FACE('',(#7877),#382,.F.);
#26702=ADVANCED_FACE('',(#7878),#1413,.T.);
#26703=ADVANCED_FACE('',(#7879),#1414,.T.);
#26704=ADVANCED_FACE('',(#7880),#1415,.F.);
#26705=ADVANCED_FACE('',(#7881),#1416,.T.);
#26706=ADVANCED_FACE('',(#7882),#6696,.F.);
#26707=ADVANCED_FACE('',(#7883),#6697,.T.);
#26708=ADVANCED_FACE('',(#7884),#1417,.T.);
#26709=ADVANCED_FACE('',(#7885),#1418,.T.);
#26710=ADVANCED_FACE('',(#7886),#383,.T.);
#26711=ADVANCED_FACE('',(#7887),#384,.T.);
#26712=ADVANCED_FACE('',(#7888),#1419,.T.);
#26713=ADVANCED_FACE('',(#7889),#1420,.T.);
#26714=ADVANCED_FACE('',(#7890),#1421,.T.);
#26715=ADVANCED_FACE('',(#7891),#1422,.T.);
#26716=ADVANCED_FACE('',(#7892),#1423,.T.);
#26717=ADVANCED_FACE('',(#7893),#1424,.T.);
#26718=ADVANCED_FACE('',(#7894),#1425,.T.);
#26719=ADVANCED_FACE('',(#7895),#571,.T.);
#26720=ADVANCED_FACE('',(#7896),#1426,.T.);
#26721=ADVANCED_FACE('',(#7897),#572,.T.);
#26722=ADVANCED_FACE('',(#7898),#573,.T.);
#26723=ADVANCED_FACE('',(#7899),#1427,.T.);
#26724=ADVANCED_FACE('',(#7900),#1428,.T.);
#26725=ADVANCED_FACE('',(#7901),#574,.T.);
#26726=ADVANCED_FACE('',(#7902),#575,.T.);
#26727=ADVANCED_FACE('',(#7903),#1429,.T.);
#26728=ADVANCED_FACE('',(#7904),#1430,.T.);
#26729=ADVANCED_FACE('',(#7905),#576,.T.);
#26730=ADVANCED_FACE('',(#7906),#1431,.T.);
#26731=ADVANCED_FACE('',(#7907),#1432,.F.);
#26732=ADVANCED_FACE('',(#7908),#1433,.T.);
#26733=ADVANCED_FACE('',(#7909),#1434,.F.);
#26734=ADVANCED_FACE('',(#7910),#1435,.T.);
#26735=ADVANCED_FACE('',(#7911),#1436,.F.);
#26736=ADVANCED_FACE('',(#7912),#1437,.T.);
#26737=ADVANCED_FACE('',(#7913),#1438,.T.);
#26738=ADVANCED_FACE('',(#7914),#1439,.T.);
#26739=ADVANCED_FACE('',(#7915),#1440,.F.);
#26740=ADVANCED_FACE('',(#7916),#1441,.F.);
#26741=ADVANCED_FACE('',(#7917),#1442,.F.);
#26742=ADVANCED_FACE('',(#7918),#1443,.T.);
#26743=ADVANCED_FACE('',(#7919),#1444,.T.);
#26744=ADVANCED_FACE('',(#7920),#1445,.T.);
#26745=ADVANCED_FACE('',(#7921),#1446,.T.);
#26746=ADVANCED_FACE('',(#7922),#1447,.T.);
#26747=ADVANCED_FACE('',(#7923),#1448,.T.);
#26748=ADVANCED_FACE('',(#7924),#1449,.T.);
#26749=ADVANCED_FACE('',(#7925),#1450,.T.);
#26750=ADVANCED_FACE('',(#7926),#385,.T.);
#26751=ADVANCED_FACE('',(#7927),#6698,.T.);
#26752=ADVANCED_FACE('',(#7928),#1451,.T.);
#26753=ADVANCED_FACE('',(#7929),#386,.T.);
#26754=ADVANCED_FACE('',(#7930),#1452,.T.);
#26755=ADVANCED_FACE('',(#7931),#387,.T.);
#26756=ADVANCED_FACE('',(#7932),#1453,.T.);
#26757=ADVANCED_FACE('',(#7933),#388,.T.);
#26758=ADVANCED_FACE('',(#7934),#1454,.T.);
#26759=ADVANCED_FACE('',(#7935),#389,.T.);
#26760=ADVANCED_FACE('',(#7936),#6699,.T.);
#26761=ADVANCED_FACE('',(#7937),#1455,.T.);
#26762=ADVANCED_FACE('',(#7938),#6700,.T.);
#26763=ADVANCED_FACE('',(#7939),#1456,.T.);
#26764=ADVANCED_FACE('',(#7940,#704,#705,#706,#707,#708),#1457,.F.);
#26765=ADVANCED_FACE('',(#7941),#1458,.T.);
#26766=ADVANCED_FACE('',(#7942),#390,.T.);
#26767=ADVANCED_FACE('',(#7943),#1459,.T.);
#26768=ADVANCED_FACE('',(#7944),#391,.T.);
#26769=ADVANCED_FACE('',(#7945),#1460,.T.);
#26770=ADVANCED_FACE('',(#7946),#392,.T.);
#26771=ADVANCED_FACE('',(#7947),#1461,.T.);
#26772=ADVANCED_FACE('',(#7948),#393,.T.);
#26773=ADVANCED_FACE('',(#7949),#6701,.T.);
#26774=ADVANCED_FACE('',(#7950),#1462,.T.);
#26775=ADVANCED_FACE('',(#7951),#6702,.T.);
#26776=ADVANCED_FACE('',(#7952,#709,#710,#711,#712),#1463,.T.);
#26777=ADVANCED_FACE('',(#7953),#1464,.T.);
#26778=ADVANCED_FACE('',(#7954),#394,.T.);
#26779=ADVANCED_FACE('',(#7955),#1465,.T.);
#26780=ADVANCED_FACE('',(#7956),#395,.T.);
#26781=ADVANCED_FACE('',(#7957),#1466,.T.);
#26782=ADVANCED_FACE('',(#7958),#396,.T.);
#26783=ADVANCED_FACE('',(#7959),#1467,.T.);
#26784=ADVANCED_FACE('',(#7960),#397,.T.);
#26785=ADVANCED_FACE('',(#7961),#6703,.T.);
#26786=ADVANCED_FACE('',(#7962),#1468,.T.);
#26787=ADVANCED_FACE('',(#7963),#6704,.T.);
#26788=ADVANCED_FACE('',(#7964),#1469,.T.);
#26789=ADVANCED_FACE('',(#7965),#1470,.F.);
#26790=ADVANCED_FACE('',(#7966),#6705,.T.);
#26791=ADVANCED_FACE('',(#7967),#1471,.T.);
#26792=ADVANCED_FACE('',(#7968),#6706,.T.);
#26793=ADVANCED_FACE('',(#7969),#1472,.T.);
#26794=ADVANCED_FACE('',(#7970),#6707,.F.);
#26795=ADVANCED_FACE('',(#7971),#6708,.F.);
#26796=ADVANCED_FACE('',(#7972),#6709,.F.);
#26797=ADVANCED_FACE('',(#7973),#6710,.F.);
#26798=ADVANCED_FACE('',(#7974),#1473,.T.);
#26799=ADVANCED_FACE('',(#7975),#398,.T.);
#26800=ADVANCED_FACE('',(#7976),#399,.T.);
#26801=ADVANCED_FACE('',(#7977),#400,.T.);
#26802=ADVANCED_FACE('',(#7978),#401,.T.);
#26803=ADVANCED_FACE('',(#7979,#713),#1474,.T.);
#26804=ADVANCED_FACE('',(#7980),#402,.T.);
#26805=ADVANCED_FACE('',(#7981),#403,.T.);
#26806=ADVANCED_FACE('',(#7982),#1475,.T.);
#26807=ADVANCED_FACE('',(#7983),#1476,.T.);
#26808=ADVANCED_FACE('',(#7984),#1477,.T.);
#26809=ADVANCED_FACE('',(#7985),#1478,.T.);
#26810=ADVANCED_FACE('',(#7986),#1479,.T.);
#26811=ADVANCED_FACE('',(#7987),#1480,.T.);
#26812=ADVANCED_FACE('',(#7988),#1481,.T.);
#26813=ADVANCED_FACE('',(#7989),#1482,.T.);
#26814=ADVANCED_FACE('',(#7990),#1483,.T.);
#26815=ADVANCED_FACE('',(#7991),#1484,.T.);
#26816=ADVANCED_FACE('',(#7992),#1485,.T.);
#26817=ADVANCED_FACE('',(#7993),#1486,.T.);
#26818=ADVANCED_FACE('',(#7994),#1487,.T.);
#26819=ADVANCED_FACE('',(#7995),#1488,.T.);
#26820=ADVANCED_FACE('',(#7996),#1489,.T.);
#26821=ADVANCED_FACE('',(#7997),#1490,.T.);
#26822=ADVANCED_FACE('',(#7998),#1491,.T.);
#26823=ADVANCED_FACE('',(#7999),#1492,.T.);
#26824=ADVANCED_FACE('',(#8000),#1493,.T.);
#26825=ADVANCED_FACE('',(#8001),#1494,.T.);
#26826=ADVANCED_FACE('',(#8002),#1495,.T.);
#26827=ADVANCED_FACE('',(#8003),#404,.T.);
#26828=ADVANCED_FACE('',(#8004,#714),#6711,.T.);
#26829=ADVANCED_FACE('',(#8005),#405,.T.);
#26830=ADVANCED_FACE('',(#8006),#1496,.T.);
#26831=ADVANCED_FACE('',(#8007),#1497,.T.);
#26832=ADVANCED_FACE('',(#8008),#1498,.T.);
#26833=ADVANCED_FACE('',(#8009),#1499,.T.);
#26834=ADVANCED_FACE('',(#8010),#1500,.T.);
#26835=ADVANCED_FACE('',(#8011),#1501,.T.);
#26836=ADVANCED_FACE('',(#8012),#1502,.T.);
#26837=ADVANCED_FACE('',(#8013),#1503,.T.);
#26838=ADVANCED_FACE('',(#8014),#1504,.T.);
#26839=ADVANCED_FACE('',(#8015),#1505,.T.);
#26840=ADVANCED_FACE('',(#8016),#1506,.T.);
#26841=ADVANCED_FACE('',(#8017),#1507,.T.);
#26842=ADVANCED_FACE('',(#8018),#1508,.T.);
#26843=ADVANCED_FACE('',(#8019),#1509,.T.);
#26844=ADVANCED_FACE('',(#8020),#1510,.T.);
#26845=ADVANCED_FACE('',(#8021),#1511,.T.);
#26846=ADVANCED_FACE('',(#8022),#1512,.F.);
#26847=ADVANCED_FACE('',(#8023),#1513,.T.);
#26848=ADVANCED_FACE('',(#8024),#1514,.T.);
#26849=ADVANCED_FACE('',(#8025),#1515,.T.);
#26850=ADVANCED_FACE('',(#8026),#1516,.T.);
#26851=ADVANCED_FACE('',(#8027),#1517,.T.);
#26852=ADVANCED_FACE('',(#8028),#1518,.T.);
#26853=ADVANCED_FACE('',(#8029),#1519,.T.);
#26854=ADVANCED_FACE('',(#8030),#1520,.T.);
#26855=ADVANCED_FACE('',(#8031),#1521,.T.);
#26856=ADVANCED_FACE('',(#8032),#1522,.T.);
#26857=ADVANCED_FACE('',(#8033),#1523,.T.);
#26858=ADVANCED_FACE('',(#8034),#1524,.T.);
#26859=ADVANCED_FACE('',(#8035),#1525,.T.);
#26860=ADVANCED_FACE('',(#8036),#1526,.T.);
#26861=ADVANCED_FACE('',(#8037),#1527,.T.);
#26862=ADVANCED_FACE('',(#8038),#1528,.T.);
#26863=ADVANCED_FACE('',(#8039),#1529,.T.);
#26864=ADVANCED_FACE('',(#8040),#1530,.T.);
#26865=ADVANCED_FACE('',(#8041),#1531,.T.);
#26866=ADVANCED_FACE('',(#8042),#1532,.T.);
#26867=ADVANCED_FACE('',(#8043),#1533,.T.);
#26868=ADVANCED_FACE('',(#8044),#1534,.T.);
#26869=ADVANCED_FACE('',(#8045),#577,.T.);
#26870=ADVANCED_FACE('',(#8046),#6712,.F.);
#26871=ADVANCED_FACE('',(#8047),#1535,.T.);
#26872=ADVANCED_FACE('',(#8048),#1536,.T.);
#26873=ADVANCED_FACE('',(#8049),#1537,.T.);
#26874=ADVANCED_FACE('',(#8050),#1538,.F.);
#26875=ADVANCED_FACE('',(#8051),#1539,.T.);
#26876=ADVANCED_FACE('',(#8052),#1540,.T.);
#26877=ADVANCED_FACE('',(#8053),#1541,.F.);
#26878=ADVANCED_FACE('',(#8054),#6713,.F.);
#26879=ADVANCED_FACE('',(#8055,#715),#1542,.T.);
#26880=ADVANCED_FACE('',(#8056),#6714,.T.);
#26881=ADVANCED_FACE('',(#8057),#6715,.T.);
#26882=ADVANCED_FACE('',(#8058),#6716,.T.);
#26883=ADVANCED_FACE('',(#8059),#6717,.T.);
#26884=ADVANCED_FACE('',(#8060),#6718,.T.);
#26885=ADVANCED_FACE('',(#8061),#6719,.T.);
#26886=ADVANCED_FACE('',(#8062),#6720,.T.);
#26887=ADVANCED_FACE('',(#8063),#6721,.T.);
#26888=ADVANCED_FACE('',(#8064),#6722,.T.);
#26889=ADVANCED_FACE('',(#8065),#6723,.T.);
#26890=ADVANCED_FACE('',(#8066),#6724,.T.);
#26891=ADVANCED_FACE('',(#8067),#6725,.T.);
#26892=ADVANCED_FACE('',(#8068),#6726,.T.);
#26893=ADVANCED_FACE('',(#8069),#6727,.T.);
#26894=ADVANCED_FACE('',(#8070),#6728,.T.);
#26895=ADVANCED_FACE('',(#8071),#6729,.T.);
#26896=ADVANCED_FACE('',(#8072),#6730,.T.);
#26897=ADVANCED_FACE('',(#8073),#6731,.T.);
#26898=ADVANCED_FACE('',(#8074),#6732,.T.);
#26899=ADVANCED_FACE('',(#8075),#6733,.T.);
#26900=ADVANCED_FACE('',(#8076),#6734,.T.);
#26901=ADVANCED_FACE('',(#8077),#6735,.T.);
#26902=ADVANCED_FACE('',(#8078),#6736,.T.);
#26903=ADVANCED_FACE('',(#8079),#6737,.T.);
#26904=ADVANCED_FACE('',(#8080),#6738,.T.);
#26905=ADVANCED_FACE('',(#8081),#6739,.T.);
#26906=ADVANCED_FACE('',(#8082),#6740,.T.);
#26907=ADVANCED_FACE('',(#8083),#6741,.T.);
#26908=ADVANCED_FACE('',(#8084),#6742,.T.);
#26909=ADVANCED_FACE('',(#8085),#6743,.T.);
#26910=ADVANCED_FACE('',(#8086),#6744,.T.);
#26911=ADVANCED_FACE('',(#8087),#6745,.T.);
#26912=ADVANCED_FACE('',(#8088),#6746,.T.);
#26913=ADVANCED_FACE('',(#8089),#6747,.T.);
#26914=ADVANCED_FACE('',(#8090),#6748,.T.);
#26915=ADVANCED_FACE('',(#8091),#6749,.T.);
#26916=ADVANCED_FACE('',(#8092),#6750,.T.);
#26917=ADVANCED_FACE('',(#8093),#6751,.T.);
#26918=ADVANCED_FACE('',(#8094),#6752,.T.);
#26919=ADVANCED_FACE('',(#8095),#6753,.T.);
#26920=ADVANCED_FACE('',(#8096),#578,.F.);
#26921=ADVANCED_FACE('',(#8097),#1543,.T.);
#26922=ADVANCED_FACE('',(#8098),#6754,.T.);
#26923=ADVANCED_FACE('',(#8099),#579,.F.);
#26924=ADVANCED_FACE('',(#8100),#406,.T.);
#26925=ADVANCED_FACE('',(#8101),#1544,.T.);
#26926=ADVANCED_FACE('',(#8102),#1545,.T.);
#26927=ADVANCED_FACE('',(#8103),#1546,.T.);
#26928=ADVANCED_FACE('',(#8104,#716),#1547,.F.);
#26929=ADVANCED_FACE('',(#8105),#1548,.T.);
#26930=ADVANCED_FACE('',(#8106),#1549,.T.);
#26931=ADVANCED_FACE('',(#8107),#1550,.T.);
#26932=ADVANCED_FACE('',(#8108),#1551,.T.);
#26933=ADVANCED_FACE('',(#8109),#1552,.T.);
#26934=ADVANCED_FACE('',(#8110),#407,.T.);
#26935=ADVANCED_FACE('',(#8111),#6755,.T.);
#26936=ADVANCED_FACE('',(#8112),#6756,.T.);
#26937=ADVANCED_FACE('',(#8113),#6757,.T.);
#26938=ADVANCED_FACE('',(#8114),#6758,.T.);
#26939=ADVANCED_FACE('',(#8115),#6759,.T.);
#26940=ADVANCED_FACE('',(#8116),#6760,.T.);
#26941=ADVANCED_FACE('',(#8117),#6761,.T.);
#26942=ADVANCED_FACE('',(#8118),#6762,.T.);
#26943=ADVANCED_FACE('',(#8119),#6763,.T.);
#26944=ADVANCED_FACE('',(#8120),#6764,.T.);
#26945=ADVANCED_FACE('',(#8121),#6765,.T.);
#26946=ADVANCED_FACE('',(#8122),#6766,.T.);
#26947=ADVANCED_FACE('',(#8123),#6767,.T.);
#26948=ADVANCED_FACE('',(#8124),#6768,.T.);
#26949=ADVANCED_FACE('',(#8125),#6769,.T.);
#26950=ADVANCED_FACE('',(#8126),#6770,.T.);
#26951=ADVANCED_FACE('',(#8127),#6771,.T.);
#26952=ADVANCED_FACE('',(#8128),#6772,.T.);
#26953=ADVANCED_FACE('',(#8129),#6773,.T.);
#26954=ADVANCED_FACE('',(#8130),#6774,.T.);
#26955=ADVANCED_FACE('',(#8131),#6775,.T.);
#26956=ADVANCED_FACE('',(#8132),#6776,.T.);
#26957=ADVANCED_FACE('',(#8133),#6777,.T.);
#26958=ADVANCED_FACE('',(#8134),#6778,.T.);
#26959=ADVANCED_FACE('',(#8135),#6779,.T.);
#26960=ADVANCED_FACE('',(#8136),#6780,.T.);
#26961=ADVANCED_FACE('',(#8137),#6781,.T.);
#26962=ADVANCED_FACE('',(#8138),#6782,.T.);
#26963=ADVANCED_FACE('',(#8139),#6783,.T.);
#26964=ADVANCED_FACE('',(#8140),#6784,.T.);
#26965=ADVANCED_FACE('',(#8141),#6785,.T.);
#26966=ADVANCED_FACE('',(#8142),#6786,.T.);
#26967=ADVANCED_FACE('',(#8143),#6787,.T.);
#26968=ADVANCED_FACE('',(#8144),#6788,.T.);
#26969=ADVANCED_FACE('',(#8145),#6789,.T.);
#26970=ADVANCED_FACE('',(#8146),#6790,.T.);
#26971=ADVANCED_FACE('',(#8147),#6791,.T.);
#26972=ADVANCED_FACE('',(#8148),#6792,.T.);
#26973=ADVANCED_FACE('',(#8149),#6793,.T.);
#26974=ADVANCED_FACE('',(#8150),#6794,.T.);
#26975=ADVANCED_FACE('',(#8151),#6795,.T.);
#26976=ADVANCED_FACE('',(#8152),#580,.F.);
#26977=ADVANCED_FACE('',(#8153),#1553,.T.);
#26978=ADVANCED_FACE('',(#8154),#6796,.T.);
#26979=ADVANCED_FACE('',(#8155),#581,.F.);
#26980=ADVANCED_FACE('',(#8156),#1554,.F.);
#26981=ADVANCED_FACE('',(#8157),#1555,.T.);
#26982=ADVANCED_FACE('',(#8158),#1556,.F.);
#26983=ADVANCED_FACE('',(#8159),#1557,.F.);
#26984=ADVANCED_FACE('',(#8160),#1558,.F.);
#26985=ADVANCED_FACE('',(#8161),#1559,.T.);
#26986=ADVANCED_FACE('',(#8162),#1560,.F.);
#26987=ADVANCED_FACE('',(#8163),#1561,.F.);
#26988=ADVANCED_FACE('',(#8164),#1562,.F.);
#26989=ADVANCED_FACE('',(#8165),#1563,.T.);
#26990=ADVANCED_FACE('',(#8166),#1564,.F.);
#26991=ADVANCED_FACE('',(#8167),#1565,.F.);
#26992=ADVANCED_FACE('',(#8168),#1566,.F.);
#26993=ADVANCED_FACE('',(#8169),#1567,.T.);
#26994=ADVANCED_FACE('',(#8170),#1568,.F.);
#26995=ADVANCED_FACE('',(#8171),#1569,.F.);
#26996=ADVANCED_FACE('',(#8172),#1570,.F.);
#26997=ADVANCED_FACE('',(#8173),#1571,.T.);
#26998=ADVANCED_FACE('',(#8174),#1572,.F.);
#26999=ADVANCED_FACE('',(#8175),#1573,.F.);
#27000=ADVANCED_FACE('',(#8176),#1574,.F.);
#27001=ADVANCED_FACE('',(#8177),#1575,.T.);
#27002=ADVANCED_FACE('',(#8178),#1576,.F.);
#27003=ADVANCED_FACE('',(#8179),#1577,.F.);
#27004=ADVANCED_FACE('',(#8180),#1578,.F.);
#27005=ADVANCED_FACE('',(#8181),#1579,.T.);
#27006=ADVANCED_FACE('',(#8182),#1580,.F.);
#27007=ADVANCED_FACE('',(#8183),#1581,.F.);
#27008=ADVANCED_FACE('',(#8184),#1582,.F.);
#27009=ADVANCED_FACE('',(#8185),#1583,.T.);
#27010=ADVANCED_FACE('',(#8186),#1584,.F.);
#27011=ADVANCED_FACE('',(#8187),#1585,.F.);
#27012=ADVANCED_FACE('',(#8188),#1586,.F.);
#27013=ADVANCED_FACE('',(#8189),#1587,.T.);
#27014=ADVANCED_FACE('',(#8190),#1588,.F.);
#27015=ADVANCED_FACE('',(#8191),#1589,.F.);
#27016=ADVANCED_FACE('',(#8192),#1590,.F.);
#27017=ADVANCED_FACE('',(#8193),#1591,.T.);
#27018=ADVANCED_FACE('',(#8194),#1592,.F.);
#27019=ADVANCED_FACE('',(#8195),#1593,.F.);
#27020=ADVANCED_FACE('',(#8196),#1594,.F.);
#27021=ADVANCED_FACE('',(#8197),#1595,.T.);
#27022=ADVANCED_FACE('',(#8198),#1596,.F.);
#27023=ADVANCED_FACE('',(#8199),#1597,.F.);
#27024=ADVANCED_FACE('',(#8200),#1598,.F.);
#27025=ADVANCED_FACE('',(#8201),#1599,.T.);
#27026=ADVANCED_FACE('',(#8202),#1600,.F.);
#27027=ADVANCED_FACE('',(#8203),#1601,.F.);
#27028=ADVANCED_FACE('',(#8204),#1602,.F.);
#27029=ADVANCED_FACE('',(#8205),#1603,.T.);
#27030=ADVANCED_FACE('',(#8206),#1604,.F.);
#27031=ADVANCED_FACE('',(#8207),#1605,.F.);
#27032=ADVANCED_FACE('',(#8208),#1606,.F.);
#27033=ADVANCED_FACE('',(#8209),#1607,.T.);
#27034=ADVANCED_FACE('',(#8210),#1608,.F.);
#27035=ADVANCED_FACE('',(#8211),#1609,.F.);
#27036=ADVANCED_FACE('',(#8212),#1610,.F.);
#27037=ADVANCED_FACE('',(#8213),#1611,.T.);
#27038=ADVANCED_FACE('',(#8214),#1612,.F.);
#27039=ADVANCED_FACE('',(#8215),#1613,.F.);
#27040=ADVANCED_FACE('',(#8216),#1614,.F.);
#27041=ADVANCED_FACE('',(#8217),#1615,.T.);
#27042=ADVANCED_FACE('',(#8218),#1616,.F.);
#27043=ADVANCED_FACE('',(#8219),#1617,.F.);
#27044=ADVANCED_FACE('',(#8220),#1618,.F.);
#27045=ADVANCED_FACE('',(#8221),#1619,.T.);
#27046=ADVANCED_FACE('',(#8222),#1620,.F.);
#27047=ADVANCED_FACE('',(#8223),#1621,.F.);
#27048=ADVANCED_FACE('',(#8224),#1622,.F.);
#27049=ADVANCED_FACE('',(#8225),#1623,.T.);
#27050=ADVANCED_FACE('',(#8226),#1624,.F.);
#27051=ADVANCED_FACE('',(#8227),#1625,.F.);
#27052=ADVANCED_FACE('',(#8228),#1626,.F.);
#27053=ADVANCED_FACE('',(#8229),#1627,.T.);
#27054=ADVANCED_FACE('',(#8230),#1628,.F.);
#27055=ADVANCED_FACE('',(#8231),#1629,.F.);
#27056=ADVANCED_FACE('',(#8232),#1630,.F.);
#27057=ADVANCED_FACE('',(#8233),#1631,.T.);
#27058=ADVANCED_FACE('',(#8234),#1632,.F.);
#27059=ADVANCED_FACE('',(#8235),#1633,.F.);
#27060=ADVANCED_FACE('',(#8236),#1634,.F.);
#27061=ADVANCED_FACE('',(#8237),#1635,.T.);
#27062=ADVANCED_FACE('',(#8238),#1636,.F.);
#27063=ADVANCED_FACE('',(#8239),#1637,.F.);
#27064=ADVANCED_FACE('',(#8240),#1638,.F.);
#27065=ADVANCED_FACE('',(#8241),#1639,.T.);
#27066=ADVANCED_FACE('',(#8242),#1640,.F.);
#27067=ADVANCED_FACE('',(#8243),#1641,.F.);
#27068=ADVANCED_FACE('',(#8244),#1642,.F.);
#27069=ADVANCED_FACE('',(#8245),#1643,.T.);
#27070=ADVANCED_FACE('',(#8246),#1644,.F.);
#27071=ADVANCED_FACE('',(#8247),#1645,.F.);
#27072=ADVANCED_FACE('',(#8248),#1646,.F.);
#27073=ADVANCED_FACE('',(#8249),#1647,.T.);
#27074=ADVANCED_FACE('',(#8250),#1648,.F.);
#27075=ADVANCED_FACE('',(#8251),#1649,.F.);
#27076=ADVANCED_FACE('',(#8252),#1650,.F.);
#27077=ADVANCED_FACE('',(#8253),#1651,.T.);
#27078=ADVANCED_FACE('',(#8254),#1652,.F.);
#27079=ADVANCED_FACE('',(#8255),#1653,.F.);
#27080=ADVANCED_FACE('',(#8256),#1654,.F.);
#27081=ADVANCED_FACE('',(#8257),#1655,.T.);
#27082=ADVANCED_FACE('',(#8258),#1656,.F.);
#27083=ADVANCED_FACE('',(#8259),#1657,.F.);
#27084=ADVANCED_FACE('',(#8260),#1658,.F.);
#27085=ADVANCED_FACE('',(#8261),#1659,.T.);
#27086=ADVANCED_FACE('',(#8262),#1660,.F.);
#27087=ADVANCED_FACE('',(#8263),#1661,.F.);
#27088=ADVANCED_FACE('',(#8264),#1662,.F.);
#27089=ADVANCED_FACE('',(#8265),#1663,.T.);
#27090=ADVANCED_FACE('',(#8266),#1664,.F.);
#27091=ADVANCED_FACE('',(#8267),#1665,.F.);
#27092=ADVANCED_FACE('',(#8268),#1666,.F.);
#27093=ADVANCED_FACE('',(#8269),#1667,.T.);
#27094=ADVANCED_FACE('',(#8270),#1668,.F.);
#27095=ADVANCED_FACE('',(#8271),#1669,.F.);
#27096=ADVANCED_FACE('',(#8272),#1670,.F.);
#27097=ADVANCED_FACE('',(#8273),#1671,.T.);
#27098=ADVANCED_FACE('',(#8274),#1672,.F.);
#27099=ADVANCED_FACE('',(#8275),#1673,.F.);
#27100=ADVANCED_FACE('',(#8276),#1674,.F.);
#27101=ADVANCED_FACE('',(#8277),#1675,.T.);
#27102=ADVANCED_FACE('',(#8278),#1676,.F.);
#27103=ADVANCED_FACE('',(#8279),#1677,.F.);
#27104=ADVANCED_FACE('',(#8280),#1678,.F.);
#27105=ADVANCED_FACE('',(#8281),#1679,.T.);
#27106=ADVANCED_FACE('',(#8282),#1680,.F.);
#27107=ADVANCED_FACE('',(#8283),#1681,.F.);
#27108=ADVANCED_FACE('',(#8284),#1682,.F.);
#27109=ADVANCED_FACE('',(#8285),#1683,.T.);
#27110=ADVANCED_FACE('',(#8286),#1684,.F.);
#27111=ADVANCED_FACE('',(#8287),#1685,.F.);
#27112=ADVANCED_FACE('',(#8288),#1686,.F.);
#27113=ADVANCED_FACE('',(#8289),#1687,.T.);
#27114=ADVANCED_FACE('',(#8290),#1688,.F.);
#27115=ADVANCED_FACE('',(#8291),#1689,.F.);
#27116=ADVANCED_FACE('',(#8292),#1690,.F.);
#27117=ADVANCED_FACE('',(#8293),#1691,.T.);
#27118=ADVANCED_FACE('',(#8294),#1692,.F.);
#27119=ADVANCED_FACE('',(#8295),#1693,.F.);
#27120=ADVANCED_FACE('',(#8296),#1694,.F.);
#27121=ADVANCED_FACE('',(#8297),#1695,.T.);
#27122=ADVANCED_FACE('',(#8298),#1696,.F.);
#27123=ADVANCED_FACE('',(#8299),#1697,.F.);
#27124=ADVANCED_FACE('',(#8300),#1698,.F.);
#27125=ADVANCED_FACE('',(#8301),#1699,.F.);
#27126=ADVANCED_FACE('',(#8302),#1700,.F.);
#27127=ADVANCED_FACE('',(#8303),#1701,.F.);
#27128=ADVANCED_FACE('',(#8304),#1702,.F.);
#27129=ADVANCED_FACE('',(#8305),#1703,.F.);
#27130=ADVANCED_FACE('',(#8306),#1704,.F.);
#27131=ADVANCED_FACE('',(#8307),#1705,.T.);
#27132=ADVANCED_FACE('',(#8308),#408,.T.);
#27133=ADVANCED_FACE('',(#8309),#6797,.T.);
#27134=ADVANCED_FACE('',(#8310,#717),#1706,.T.);
#27135=ADVANCED_FACE('',(#8311,#718,#719,#720,#721,#722,#723,#724,#725,
#726,#727,#728,#729,#730,#731,#732,#733,#734,#735,#736,#737,#738,#739,#740,
#741,#742,#743,#744,#745,#746,#747,#748,#749,#750,#751,#752),#6798,.T.);
#27136=ADVANCED_FACE('',(#8312),#409,.T.);
#27137=ADVANCED_FACE('',(#8313,#753),#1707,.T.);
#27138=ADVANCED_FACE('',(#8314),#1708,.T.);
#27139=ADVANCED_FACE('',(#8315),#1709,.T.);
#27140=ADVANCED_FACE('',(#8316),#1710,.T.);
#27141=ADVANCED_FACE('',(#8317),#1711,.T.);
#27142=ADVANCED_FACE('',(#8318),#1712,.T.);
#27143=ADVANCED_FACE('',(#8319),#1713,.T.);
#27144=ADVANCED_FACE('',(#8320),#1714,.T.);
#27145=ADVANCED_FACE('',(#8321),#1715,.T.);
#27146=ADVANCED_FACE('',(#8322),#1716,.T.);
#27147=ADVANCED_FACE('',(#8323),#1717,.T.);
#27148=ADVANCED_FACE('',(#8324),#1718,.T.);
#27149=ADVANCED_FACE('',(#8325),#1719,.T.);
#27150=ADVANCED_FACE('',(#8326),#1720,.T.);
#27151=ADVANCED_FACE('',(#8327),#1721,.T.);
#27152=ADVANCED_FACE('',(#8328),#1722,.T.);
#27153=ADVANCED_FACE('',(#8329),#1723,.T.);
#27154=ADVANCED_FACE('',(#8330),#1724,.T.);
#27155=ADVANCED_FACE('',(#8331),#1725,.T.);
#27156=ADVANCED_FACE('',(#8332),#1726,.T.);
#27157=ADVANCED_FACE('',(#8333),#1727,.T.);
#27158=ADVANCED_FACE('',(#8334),#1728,.T.);
#27159=ADVANCED_FACE('',(#8335,#754),#1729,.T.);
#27160=ADVANCED_FACE('',(#8336),#1730,.T.);
#27161=ADVANCED_FACE('',(#8337),#1731,.T.);
#27162=ADVANCED_FACE('',(#8338),#1732,.T.);
#27163=ADVANCED_FACE('',(#8339),#1733,.T.);
#27164=ADVANCED_FACE('',(#8340),#1734,.T.);
#27165=ADVANCED_FACE('',(#8341),#1735,.T.);
#27166=ADVANCED_FACE('',(#8342),#1736,.F.);
#27167=ADVANCED_FACE('',(#8343),#1737,.F.);
#27168=ADVANCED_FACE('',(#8344),#1738,.F.);
#27169=ADVANCED_FACE('',(#8345),#1739,.F.);
#27170=ADVANCED_FACE('',(#8346),#1740,.F.);
#27171=ADVANCED_FACE('',(#8347),#1741,.F.);
#27172=ADVANCED_FACE('',(#8348),#1742,.F.);
#27173=ADVANCED_FACE('',(#8349,#755),#1743,.F.);
#27174=ADVANCED_FACE('',(#8350),#1744,.T.);
#27175=ADVANCED_FACE('',(#8351),#1745,.T.);
#27176=ADVANCED_FACE('',(#8352),#1746,.T.);
#27177=ADVANCED_FACE('',(#8353),#1747,.T.);
#27178=ADVANCED_FACE('',(#8354),#410,.T.);
#27179=ADVANCED_FACE('',(#8355),#6799,.T.);
#27180=ADVANCED_FACE('',(#8356),#6800,.T.);
#27181=ADVANCED_FACE('',(#8357),#6801,.T.);
#27182=ADVANCED_FACE('',(#8358),#6802,.T.);
#27183=ADVANCED_FACE('',(#8359),#6803,.T.);
#27184=ADVANCED_FACE('',(#8360),#6804,.T.);
#27185=ADVANCED_FACE('',(#8361),#6805,.T.);
#27186=ADVANCED_FACE('',(#8362),#6806,.T.);
#27187=ADVANCED_FACE('',(#8363),#6807,.T.);
#27188=ADVANCED_FACE('',(#8364),#6808,.T.);
#27189=ADVANCED_FACE('',(#8365),#6809,.T.);
#27190=ADVANCED_FACE('',(#8366),#6810,.T.);
#27191=ADVANCED_FACE('',(#8367),#6811,.T.);
#27192=ADVANCED_FACE('',(#8368),#6812,.T.);
#27193=ADVANCED_FACE('',(#8369),#6813,.T.);
#27194=ADVANCED_FACE('',(#8370),#6814,.T.);
#27195=ADVANCED_FACE('',(#8371),#6815,.T.);
#27196=ADVANCED_FACE('',(#8372),#6816,.T.);
#27197=ADVANCED_FACE('',(#8373),#6817,.T.);
#27198=ADVANCED_FACE('',(#8374),#6818,.T.);
#27199=ADVANCED_FACE('',(#8375),#6819,.T.);
#27200=ADVANCED_FACE('',(#8376),#6820,.T.);
#27201=ADVANCED_FACE('',(#8377),#6821,.T.);
#27202=ADVANCED_FACE('',(#8378),#6822,.T.);
#27203=ADVANCED_FACE('',(#8379),#6823,.T.);
#27204=ADVANCED_FACE('',(#8380),#6824,.T.);
#27205=ADVANCED_FACE('',(#8381),#582,.F.);
#27206=ADVANCED_FACE('',(#8382),#1748,.T.);
#27207=ADVANCED_FACE('',(#8383),#6825,.T.);
#27208=ADVANCED_FACE('',(#8384),#583,.F.);
#27209=ADVANCED_FACE('',(#8385),#1749,.F.);
#27210=ADVANCED_FACE('',(#8386),#1750,.F.);
#27211=ADVANCED_FACE('',(#8387),#1751,.F.);
#27212=ADVANCED_FACE('',(#8388),#1752,.F.);
#27213=ADVANCED_FACE('',(#8389),#1753,.F.);
#27214=ADVANCED_FACE('',(#8390),#1754,.F.);
#27215=ADVANCED_FACE('',(#8391),#1755,.F.);
#27216=ADVANCED_FACE('',(#8392),#1756,.T.);
#27217=ADVANCED_FACE('',(#8393),#411,.T.);
#27218=ADVANCED_FACE('',(#8394),#6826,.T.);
#27219=ADVANCED_FACE('',(#8395,#756),#1757,.T.);
#27220=ADVANCED_FACE('',(#8396),#604,.F.);
#27221=CLOSED_SHELL('',(#25651,#25652,#25653,#25654,#25655,#25656,#25657,
#25658,#25659,#25660,#25661,#25662,#25663,#25664,#25665,#25666,#25667,#25668,
#25669,#25670,#25671,#25672,#25673,#25674,#25675,#25676,#25677,#25678,#25679,
#25680,#25681,#25682,#25683,#25684,#25685,#25686,#25687,#25688,#25689,#25690,
#25691,#25692,#25693,#25694,#25695,#25696,#25697,#25698,#25699,#25700,#25701,
#25702,#25703,#25704,#25705,#25706,#25707,#25708,#25709,#25710,#25711,#25712,
#25713,#25714,#25715,#25716,#25717,#25718,#25719,#25720,#25721,#25722,#25723,
#25724,#25725,#25726,#25727,#25728,#25729,#25730,#25731,#25732,#25733,#25734,
#25735,#25736,#25737,#25738,#25739,#25740,#25741,#25742,#25743,#25744,#25745,
#25746,#25747,#25748,#25749,#25750,#25751,#25752,#25753,#25754,#25755,#25756,
#25757,#25758,#25759,#25760,#25761,#25762,#25763,#25764,#25765,#25766,#25767,
#25768,#25769,#25770,#25771,#25772,#25773,#25774,#25775,#25776,#25777,#25778,
#25779,#25780,#25781,#25782,#25783,#25784,#25785,#25786,#25787,#25788,#25789,
#25790,#25791,#25792,#25793,#25794,#25795,#25796,#25797,#25798,#25799,#25800,
#25801,#25802,#25803,#25804,#25805,#25806,#25807));
#27222=CLOSED_SHELL('',(#25808,#25809,#25810,#25811,#25812,#25813,#25814,
#25815,#25816,#25817,#25818,#25819,#25820,#25821,#25822,#25823,#25824,#25825,
#25826,#25827,#25828,#25829,#25830,#25831,#25832,#25833,#25834,#25835,#25836,
#25837,#25838,#25839,#25840,#25841,#25842,#25843,#25844,#25845,#25846,#25847,
#25848,#25849,#25850,#25851,#25852,#25853,#25854,#25855,#25856,#25857,#25858,
#25859,#25860,#25861,#25862,#25863,#25864,#25865,#25866,#25867,#25868,#25869,
#25870,#25871,#25872,#25873,#25874,#25875,#25876,#25877,#25878,#25879,#25880,
#25881,#25882,#25883,#25884,#25885,#25886,#25887,#25888,#25889,#25890,#25891,
#25892,#25893,#25894,#25895,#25896,#25897,#25898,#25899,#25900,#25901,#25902,
#25903,#25904,#25905,#25906,#25907,#25908,#25909,#25910,#25911,#25912,#25913,
#25914,#25915,#25916,#25917,#25918,#25919,#25920,#25921,#25922,#25923,#25924,
#25925,#25926,#25927,#25928,#25929,#25930,#25931,#25932,#25933,#25934,#25935,
#25936,#25937,#25938,#25939,#25940,#25941,#25942,#25943,#25944,#25945,#25946,
#25947,#25948,#25949,#25950,#25951,#25952,#25953,#25954,#25955,#25956,#25957,
#25958,#25959,#25960,#25961,#25962,#25963,#25964,#25965,#25966,#25967,#25968,
#25969,#25970,#25971,#25972,#25973,#25974,#25975,#25976,#25977,#25978,#25979,
#25980,#25981,#25982,#25983,#25984,#25985,#25986,#25987,#25988,#25989,#25990,
#25991,#25992,#25993,#25994,#25995));
#27223=CLOSED_SHELL('',(#25996,#25997,#25998,#25999,#26000,#26001,#26002,
#26003,#26004,#26005,#26006,#26007,#26008,#26009,#26010,#26011,#26012,#26013,
#26014,#26015,#26016,#26017,#26018,#26019,#26020,#26021,#26022,#26023,#26024,
#26025,#26026,#26027,#26028,#26029,#26030,#26031,#26032,#26033,#26034,#26035,
#26036,#26037,#26038,#26039,#26040,#26041,#26042,#26043,#26044,#26045,#26046,
#26047,#26048,#26049,#26050,#26051,#26052,#26053,#26054,#26055,#26056,#26057,
#26058,#26059,#26060,#26061,#26062,#26063,#26064,#26065,#26066,#26067,#26068,
#26069,#26070,#26071,#26072,#26073,#26074,#26075,#26076,#26077,#26078,#26079,
#26080,#26081,#26082,#26083,#26084,#26085,#26086,#26087,#26088,#26089,#26090,
#26091,#26092,#26093,#26094,#26095,#26096,#26097,#26098,#26099,#26100,#26101,
#26102,#26103,#26104,#26105,#26106,#26107,#26108,#26109,#26110,#26111,#26112,
#26113,#26114,#26115,#26116,#26117,#26118,#26119,#26120,#26121,#26122,#26123,
#26124,#26125,#26126,#26127,#26128,#26129,#26130,#26131,#26132,#26133,#26134,
#26135,#26136,#26137,#26138,#26139,#26140,#26141,#26142,#26143,#26144,#26145,
#26146,#26147,#26148,#26149,#26150,#26151,#26152,#26153,#26154,#26155,#26156,
#26157,#26158,#26159,#26160,#26161,#26162,#26163,#26164,#26165,#26166,#26167,
#26168,#26169,#26170,#26171,#26172));
#27224=CLOSED_SHELL('',(#26173,#26174,#26175,#26176,#26177,#26178,#26179,
#26180,#26181,#26182,#26183,#26184,#26185,#26186,#26187,#26188,#26189,#26190,
#26191,#26192,#26193,#26194,#26195,#26196,#26197,#26198,#26199,#26200,#26201,
#26202,#26203,#26204,#26205,#26206,#26207,#26208,#26209,#26210,#26211,#26212,
#26213,#26214,#26215,#26216,#26217,#26218,#26219,#26220,#26221,#26222,#26223,
#26224,#26225,#26226,#26227,#26228,#26229,#26230,#26231,#26232,#26233,#26234,
#26235,#26236,#26237,#26238,#26239,#26240,#26241,#26242,#26243,#26244,#26245,
#26246,#26247,#26248,#26249,#26250,#26251,#26252,#26253,#26254,#26255,#26256,
#26257,#26258,#26259,#26260,#26261,#26262,#26263,#26264,#26265,#26266,#26267,
#26268,#26269,#26270,#26271,#26272,#26273,#26274,#26275,#26276,#26277,#26278,
#26279,#26280,#26281,#26282,#26283,#26284,#26285,#26286,#26287,#26288,#26289,
#26290,#26291,#26292,#26293,#26294,#26295,#26296,#26297,#26298,#26299,#26300,
#26301,#26302,#26303,#26304,#26305,#26306,#26307,#26308,#26309,#26310,#26311,
#26312,#26313,#26314,#26315,#26316,#26317,#26318,#26319,#26320,#26321,#26322,
#26323,#26324,#26325,#26326,#26327,#26328,#26329,#26330,#26331,#26332,#26333,
#26334,#26335,#26336,#26337,#26338,#26339,#26340,#26341,#26342,#26343,#26344,
#26345,#26346,#26347,#26348,#26349,#26350,#26351,#26352,#26353,#26354,#26355,
#26356,#26357,#26358,#26359,#26360,#26361,#26362,#26363,#26364,#26365,#26366,
#26367,#26368,#26369,#26370,#26371,#26372,#26373,#26374,#26375,#26376,#26377,
#26378,#26379,#26380,#26381,#26382,#26383,#26384,#26385,#26386,#26387,#26388,
#26389,#26390,#26391,#26392,#26393,#26394,#26395,#26396,#26397,#26398,#26399,
#26400,#26401,#26402,#26403,#26404,#26405,#26406,#26407,#26408,#26409,#26410,
#26411,#26412,#26413,#26414,#26415,#26416,#26417,#26418,#26419,#26420,#26421,
#26422,#26423,#26424,#26425,#26426,#26427,#26428,#26429,#26430,#26431,#26432,
#26433,#26434,#26435,#26436,#26437,#26438,#26439,#26440,#26441,#26442,#26443,
#26444,#26445,#26446,#26447,#26448,#26449,#26450,#26451,#26452,#26453,#26454,
#26455,#26456,#26457,#26458,#26459,#26460,#26461,#26462,#26463,#26464,#26465,
#26466,#26467,#26468,#26469,#26470,#26471,#26472,#26473,#26474,#26475,#26476,
#26477,#26478,#26479,#26480,#26481,#26482,#26483,#26484,#26485,#26486,#26487,
#26488,#26489,#26490,#26491,#26492,#26493,#26494,#26495,#26496,#26497,#26498,
#26499,#26500,#26501,#26502,#26503,#26504,#26505,#26506,#26507,#26508,#26509,
#26510,#26511,#26512,#26513,#26514,#26515,#26516,#26517,#26518,#26519,#26520,
#26521,#26522,#26523,#26524,#26525,#26526,#26527,#26528,#26529,#26530,#26531,
#26532,#26533,#26534,#26535,#26536,#26537,#26538,#26539,#26540,#26541,#26542,
#26543,#26544,#26545,#26546,#26547,#26548,#26549,#26550,#26551,#26552,#26553,
#26554,#26555,#26556,#26557,#26558,#26559,#26560,#26561,#26562,#26563,#26564,
#26565,#26566,#26567,#26568,#26569,#26570,#26571,#26572,#26573,#26574,#26575,
#26576,#26577,#26578,#26579,#26580,#26581,#26582,#26583,#26584,#26585,#26586,
#26587,#26588,#26589,#26590,#26591,#26592,#26593,#26594,#26595,#26596,#26597,
#26598,#26599,#26600,#26601,#26602,#26603,#26604,#26605,#26606,#26607,#26608,
#26609,#26610,#26611,#26612,#26613,#26614,#26615));
#27225=CLOSED_SHELL('',(#26616,#26617,#26618,#26619,#26620,#26621,#26622,
#26623,#26624,#26625,#26626,#26627,#26628,#26629,#26630,#26631,#26632,#26633,
#26634,#26635,#26636,#26637,#26638));
#27226=CLOSED_SHELL('',(#26639,#26640,#26641,#26642,#26643,#26644,#26645,
#26646,#26647,#26648,#26649,#26650,#26651,#26652,#26653,#26654));
#27227=CLOSED_SHELL('',(#26655,#26656,#26657,#26658,#26659,#26660,#26661,
#26662,#26663,#26664));
#27228=CLOSED_SHELL('',(#26665,#26666,#26667,#26668,#26669));
#27229=CLOSED_SHELL('',(#26670,#26671,#26672,#26673,#26674));
#27230=CLOSED_SHELL('',(#26675,#26676,#26677,#26678));
#27231=CLOSED_SHELL('',(#26679));
#27232=CLOSED_SHELL('',(#26680,#26681,#26682,#26683,#26684,#26685,#26686,
#26687,#26688,#26689,#26690,#26691));
#27233=CLOSED_SHELL('',(#26692,#26693,#26694,#26695,#26696,#26697,#26698,
#26699,#26700,#26701,#26702,#26703,#26704,#26705,#26706,#26707,#26708,#26709));
#27234=CLOSED_SHELL('',(#26710,#26711,#26712,#26713,#26714,#26715,#26716,
#26717,#26718,#26719,#26720,#26721,#26722,#26723,#26724,#26725,#26726,#26727,
#26728,#26729,#26730,#26731,#26732,#26733,#26734,#26735,#26736,#26737,#26738,
#26739,#26740,#26741,#26742,#26743,#26744,#26745,#26746,#26747,#26748,#26749,
#26750,#26751));
#27235=CLOSED_SHELL('',(#26752,#26753,#26754,#26755,#26756,#26757,#26758,
#26759,#26760,#26761,#26762,#26763,#26764,#26765,#26766,#26767,#26768,#26769,
#26770,#26771,#26772,#26773,#26774,#26775,#26776,#26777,#26778,#26779,#26780,
#26781,#26782,#26783,#26784,#26785,#26786,#26787,#26788,#26789,#26790,#26791,
#26792,#26793,#26794,#26795,#26796,#26797,#26798));
#27236=CLOSED_SHELL('',(#26799,#26800,#26801,#26802,#26803,#26804,#26805,
#26806,#26807,#26808,#26809,#26810,#26811,#26812,#26813,#26814,#26815,#26816,
#26817,#26818,#26819,#26820,#26821,#26822,#26823,#26824,#26825,#26826,#26827,
#26828,#26829,#26830,#26831,#26832,#26833,#26834,#26835,#26836,#26837,#26838,
#26839,#26840,#26841,#26842,#26843,#26844,#26845,#26846,#26847,#26848,#26849,
#26850,#26851,#26852,#26853,#26854,#26855,#26856,#26857,#26858,#26859,#26860,
#26861,#26862,#26863,#26864,#26865,#26866,#26867,#26868,#26869,#26870,#26871,
#26872,#26873,#26874,#26875,#26876,#26877,#26878,#26879));
#27237=CLOSED_SHELL('',(#26880,#26881,#26882,#26883,#26884,#26885,#26886,
#26887,#26888,#26889,#26890,#26891,#26892,#26893,#26894,#26895,#26896,#26897,
#26898,#26899,#26900,#26901,#26902,#26903,#26904,#26905,#26906,#26907,#26908,
#26909,#26910,#26911,#26912,#26913,#26914,#26915,#26916,#26917,#26918,#26919,
#26920,#26921,#26922,#26923,#26924,#26925,#26926,#26927,#26928,#26929,#26930,
#26931,#26932,#26933,#26934,#26935));
#27238=CLOSED_SHELL('',(#26936,#26937,#26938,#26939,#26940,#26941,#26942,
#26943,#26944,#26945,#26946,#26947,#26948,#26949,#26950,#26951,#26952,#26953,
#26954,#26955,#26956,#26957,#26958,#26959,#26960,#26961,#26962,#26963,#26964,
#26965,#26966,#26967,#26968,#26969,#26970,#26971,#26972,#26973,#26974,#26975,
#26976,#26977,#26978,#26979,#26980,#26981,#26982,#26983,#26984,#26985,#26986,
#26987,#26988,#26989,#26990,#26991,#26992,#26993,#26994,#26995,#26996,#26997,
#26998,#26999,#27000,#27001,#27002,#27003,#27004,#27005,#27006,#27007,#27008,
#27009,#27010,#27011,#27012,#27013,#27014,#27015,#27016,#27017,#27018,#27019,
#27020,#27021,#27022,#27023,#27024,#27025,#27026,#27027,#27028,#27029,#27030,
#27031,#27032,#27033,#27034,#27035,#27036,#27037,#27038,#27039,#27040,#27041,
#27042,#27043,#27044,#27045,#27046,#27047,#27048,#27049,#27050,#27051,#27052,
#27053,#27054,#27055,#27056,#27057,#27058,#27059,#27060,#27061,#27062,#27063,
#27064,#27065,#27066,#27067,#27068,#27069,#27070,#27071,#27072,#27073,#27074,
#27075,#27076,#27077,#27078,#27079,#27080,#27081,#27082,#27083,#27084,#27085,
#27086,#27087,#27088,#27089,#27090,#27091,#27092,#27093,#27094,#27095,#27096,
#27097,#27098,#27099,#27100,#27101,#27102,#27103,#27104,#27105,#27106,#27107,
#27108,#27109,#27110,#27111,#27112,#27113,#27114,#27115,#27116,#27117,#27118,
#27119,#27120,#27121,#27122,#27123,#27124,#27125,#27126,#27127,#27128,#27129,
#27130,#27131,#27132,#27133,#27134,#27135,#27136,#27137));
#27239=CLOSED_SHELL('',(#27138,#27139,#27140,#27141,#27142,#27143,#27144,
#27145,#27146,#27147,#27148,#27149,#27150,#27151,#27152,#27153,#27154,#27155,
#27156,#27157,#27158,#27159,#27160,#27161,#27162,#27163,#27164,#27165,#27166,
#27167,#27168,#27169,#27170,#27171,#27172,#27173,#27174,#27175,#27176,#27177,
#27178,#27179));
#27240=CLOSED_SHELL('',(#27180,#27181,#27182,#27183,#27184,#27185,#27186,
#27187,#27188,#27189,#27190,#27191,#27192,#27193,#27194,#27195,#27196,#27197,
#27198,#27199,#27200,#27201,#27202,#27203,#27204,#27205,#27206,#27207,#27208,
#27209,#27210,#27211,#27212,#27213,#27214,#27215,#27216,#27217,#27218,#27219,
#27220));
#27241=DERIVED_UNIT_ELEMENT(#27281,1.);
#27242=DERIVED_UNIT_ELEMENT(#55739,-3.);
#27243=DERIVED_UNIT_ELEMENT(#27281,1.);
#27244=DERIVED_UNIT_ELEMENT(#55739,-3.);
#27245=DERIVED_UNIT_ELEMENT(#27281,1.);
#27246=DERIVED_UNIT_ELEMENT(#55739,-3.);
#27247=DERIVED_UNIT_ELEMENT(#27281,1.);
#27248=DERIVED_UNIT_ELEMENT(#55739,-3.);
#27249=DERIVED_UNIT_ELEMENT(#27281,1.);
#27250=DERIVED_UNIT_ELEMENT(#55739,-3.);
#27251=DERIVED_UNIT_ELEMENT(#27281,1.);
#27252=DERIVED_UNIT_ELEMENT(#55739,-3.);
#27253=DERIVED_UNIT_ELEMENT(#27281,1.);
#27254=DERIVED_UNIT_ELEMENT(#55739,-3.);
#27255=DERIVED_UNIT_ELEMENT(#27281,1.);
#27256=DERIVED_UNIT_ELEMENT(#55739,-3.);
#27257=DERIVED_UNIT_ELEMENT(#27281,1.);
#27258=DERIVED_UNIT_ELEMENT(#55739,-3.);
#27259=DERIVED_UNIT_ELEMENT(#27281,1.);
#27260=DERIVED_UNIT_ELEMENT(#55739,-3.);
#27261=DERIVED_UNIT_ELEMENT(#27281,1.);
#27262=DERIVED_UNIT_ELEMENT(#55739,-3.);
#27263=DERIVED_UNIT_ELEMENT(#27281,1.);
#27264=DERIVED_UNIT_ELEMENT(#55739,-3.);
#27265=DERIVED_UNIT_ELEMENT(#27281,1.);
#27266=DERIVED_UNIT_ELEMENT(#55739,-3.);
#27267=DERIVED_UNIT_ELEMENT(#27281,1.);
#27268=DERIVED_UNIT_ELEMENT(#55739,-3.);
#27269=DERIVED_UNIT_ELEMENT(#27281,1.);
#27270=DERIVED_UNIT_ELEMENT(#55739,-3.);
#27271=DERIVED_UNIT_ELEMENT(#27281,1.);
#27272=DERIVED_UNIT_ELEMENT(#55739,-3.);
#27273=DERIVED_UNIT_ELEMENT(#27281,1.);
#27274=DERIVED_UNIT_ELEMENT(#55739,-3.);
#27275=DERIVED_UNIT_ELEMENT(#27281,1.);
#27276=DERIVED_UNIT_ELEMENT(#55739,-3.);
#27277=DERIVED_UNIT_ELEMENT(#27281,1.);
#27278=DERIVED_UNIT_ELEMENT(#55739,-3.);
#27279=DERIVED_UNIT_ELEMENT(#27281,1.);
#27280=DERIVED_UNIT_ELEMENT(#55739,-3.);
#27281=(
MASS_UNIT()
NAMED_UNIT(*)
SI_UNIT(.KILO.,.GRAM.)
);
#27282=DERIVED_UNIT((#27241,#27242));
#27283=DERIVED_UNIT((#27243,#27244));
#27284=DERIVED_UNIT((#27245,#27246));
#27285=DERIVED_UNIT((#27247,#27248));
#27286=DERIVED_UNIT((#27249,#27250));
#27287=DERIVED_UNIT((#27251,#27252));
#27288=DERIVED_UNIT((#27253,#27254));
#27289=DERIVED_UNIT((#27255,#27256));
#27290=DERIVED_UNIT((#27257,#27258));
#27291=DERIVED_UNIT((#27259,#27260));
#27292=DERIVED_UNIT((#27261,#27262));
#27293=DERIVED_UNIT((#27263,#27264));
#27294=DERIVED_UNIT((#27265,#27266));
#27295=DERIVED_UNIT((#27267,#27268));
#27296=DERIVED_UNIT((#27269,#27270));
#27297=DERIVED_UNIT((#27271,#27272));
#27298=DERIVED_UNIT((#27273,#27274));
#27299=DERIVED_UNIT((#27275,#27276));
#27300=DERIVED_UNIT((#27277,#27278));
#27301=DERIVED_UNIT((#27279,#27280));
#27302=MEASURE_REPRESENTATION_ITEM('density measure',
POSITIVE_RATIO_MEASURE(7850.),#27282);
#27303=MEASURE_REPRESENTATION_ITEM('density measure',
POSITIVE_RATIO_MEASURE(7850.),#27283);
#27304=MEASURE_REPRESENTATION_ITEM('density measure',
POSITIVE_RATIO_MEASURE(7850.),#27284);
#27305=MEASURE_REPRESENTATION_ITEM('density measure',
POSITIVE_RATIO_MEASURE(7850.),#27285);
#27306=MEASURE_REPRESENTATION_ITEM('density measure',
POSITIVE_RATIO_MEASURE(7850.),#27286);
#27307=MEASURE_REPRESENTATION_ITEM('density measure',
POSITIVE_RATIO_MEASURE(7850.),#27287);
#27308=MEASURE_REPRESENTATION_ITEM('density measure',
POSITIVE_RATIO_MEASURE(7850.),#27288);
#27309=MEASURE_REPRESENTATION_ITEM('density measure',
POSITIVE_RATIO_MEASURE(7850.),#27289);
#27310=MEASURE_REPRESENTATION_ITEM('density measure',
POSITIVE_RATIO_MEASURE(7850.),#27290);
#27311=MEASURE_REPRESENTATION_ITEM('density measure',
POSITIVE_RATIO_MEASURE(7850.),#27291);
#27312=MEASURE_REPRESENTATION_ITEM('density measure',
POSITIVE_RATIO_MEASURE(7850.),#27292);
#27313=MEASURE_REPRESENTATION_ITEM('density measure',
POSITIVE_RATIO_MEASURE(7850.),#27293);
#27314=MEASURE_REPRESENTATION_ITEM('density measure',
POSITIVE_RATIO_MEASURE(7850.),#27294);
#27315=MEASURE_REPRESENTATION_ITEM('density measure',
POSITIVE_RATIO_MEASURE(7850.),#27295);
#27316=MEASURE_REPRESENTATION_ITEM('density measure',
POSITIVE_RATIO_MEASURE(7850.),#27296);
#27317=MEASURE_REPRESENTATION_ITEM('density measure',
POSITIVE_RATIO_MEASURE(7850.),#27297);
#27318=MEASURE_REPRESENTATION_ITEM('density measure',
POSITIVE_RATIO_MEASURE(7850.),#27298);
#27319=MEASURE_REPRESENTATION_ITEM('density measure',
POSITIVE_RATIO_MEASURE(7850.),#27299);
#27320=MEASURE_REPRESENTATION_ITEM('density measure',
POSITIVE_RATIO_MEASURE(7850.),#27300);
#27321=MEASURE_REPRESENTATION_ITEM('density measure',
POSITIVE_RATIO_MEASURE(7850.),#27301);
#27322=PROPERTY_DEFINITION_REPRESENTATION(#27422,#27362);
#27323=PROPERTY_DEFINITION_REPRESENTATION(#27423,#27363);
#27324=PROPERTY_DEFINITION_REPRESENTATION(#27424,#27364);
#27325=PROPERTY_DEFINITION_REPRESENTATION(#27425,#27365);
#27326=PROPERTY_DEFINITION_REPRESENTATION(#27426,#27366);
#27327=PROPERTY_DEFINITION_REPRESENTATION(#27427,#27367);
#27328=PROPERTY_DEFINITION_REPRESENTATION(#27428,#27368);
#27329=PROPERTY_DEFINITION_REPRESENTATION(#27429,#27369);
#27330=PROPERTY_DEFINITION_REPRESENTATION(#27430,#27370);
#27331=PROPERTY_DEFINITION_REPRESENTATION(#27431,#27371);
#27332=PROPERTY_DEFINITION_REPRESENTATION(#27432,#27372);
#27333=PROPERTY_DEFINITION_REPRESENTATION(#27433,#27373);
#27334=PROPERTY_DEFINITION_REPRESENTATION(#27434,#27374);
#27335=PROPERTY_DEFINITION_REPRESENTATION(#27435,#27375);
#27336=PROPERTY_DEFINITION_REPRESENTATION(#27436,#27376);
#27337=PROPERTY_DEFINITION_REPRESENTATION(#27437,#27377);
#27338=PROPERTY_DEFINITION_REPRESENTATION(#27438,#27378);
#27339=PROPERTY_DEFINITION_REPRESENTATION(#27439,#27379);
#27340=PROPERTY_DEFINITION_REPRESENTATION(#27440,#27380);
#27341=PROPERTY_DEFINITION_REPRESENTATION(#27441,#27381);
#27342=PROPERTY_DEFINITION_REPRESENTATION(#27442,#27382);
#27343=PROPERTY_DEFINITION_REPRESENTATION(#27443,#27383);
#27344=PROPERTY_DEFINITION_REPRESENTATION(#27444,#27384);
#27345=PROPERTY_DEFINITION_REPRESENTATION(#27445,#27385);
#27346=PROPERTY_DEFINITION_REPRESENTATION(#27446,#27386);
#27347=PROPERTY_DEFINITION_REPRESENTATION(#27447,#27387);
#27348=PROPERTY_DEFINITION_REPRESENTATION(#27448,#27388);
#27349=PROPERTY_DEFINITION_REPRESENTATION(#27449,#27389);
#27350=PROPERTY_DEFINITION_REPRESENTATION(#27450,#27390);
#27351=PROPERTY_DEFINITION_REPRESENTATION(#27451,#27391);
#27352=PROPERTY_DEFINITION_REPRESENTATION(#27452,#27392);
#27353=PROPERTY_DEFINITION_REPRESENTATION(#27453,#27393);
#27354=PROPERTY_DEFINITION_REPRESENTATION(#27454,#27394);
#27355=PROPERTY_DEFINITION_REPRESENTATION(#27455,#27395);
#27356=PROPERTY_DEFINITION_REPRESENTATION(#27456,#27396);
#27357=PROPERTY_DEFINITION_REPRESENTATION(#27457,#27397);
#27358=PROPERTY_DEFINITION_REPRESENTATION(#27458,#27398);
#27359=PROPERTY_DEFINITION_REPRESENTATION(#27459,#27399);
#27360=PROPERTY_DEFINITION_REPRESENTATION(#27460,#27400);
#27361=PROPERTY_DEFINITION_REPRESENTATION(#27461,#27401);
#27362=REPRESENTATION('material name',(#27402),#55717);
#27363=REPRESENTATION('density',(#27302),#55717);
#27364=REPRESENTATION('material name',(#27403),#55718);
#27365=REPRESENTATION('density',(#27303),#55718);
#27366=REPRESENTATION('material name',(#27404),#55719);
#27367=REPRESENTATION('density',(#27304),#55719);
#27368=REPRESENTATION('material name',(#27405),#55720);
#27369=REPRESENTATION('density',(#27305),#55720);
#27370=REPRESENTATION('material name',(#27406),#55721);
#27371=REPRESENTATION('density',(#27306),#55721);
#27372=REPRESENTATION('material name',(#27407),#55722);
#27373=REPRESENTATION('density',(#27307),#55722);
#27374=REPRESENTATION('material name',(#27408),#55723);
#27375=REPRESENTATION('density',(#27308),#55723);
#27376=REPRESENTATION('material name',(#27409),#55724);
#27377=REPRESENTATION('density',(#27309),#55724);
#27378=REPRESENTATION('material name',(#27410),#55725);
#27379=REPRESENTATION('density',(#27310),#55725);
#27380=REPRESENTATION('material name',(#27411),#55726);
#27381=REPRESENTATION('density',(#27311),#55726);
#27382=REPRESENTATION('material name',(#27412),#55727);
#27383=REPRESENTATION('density',(#27312),#55727);
#27384=REPRESENTATION('material name',(#27413),#55728);
#27385=REPRESENTATION('density',(#27313),#55728);
#27386=REPRESENTATION('material name',(#27414),#55729);
#27387=REPRESENTATION('density',(#27314),#55729);
#27388=REPRESENTATION('material name',(#27415),#55730);
#27389=REPRESENTATION('density',(#27315),#55730);
#27390=REPRESENTATION('material name',(#27416),#55731);
#27391=REPRESENTATION('density',(#27316),#55731);
#27392=REPRESENTATION('material name',(#27417),#55732);
#27393=REPRESENTATION('density',(#27317),#55732);
#27394=REPRESENTATION('material name',(#27418),#55733);
#27395=REPRESENTATION('density',(#27318),#55733);
#27396=REPRESENTATION('material name',(#27419),#55734);
#27397=REPRESENTATION('density',(#27319),#55734);
#27398=REPRESENTATION('material name',(#27420),#55735);
#27399=REPRESENTATION('density',(#27320),#55735);
#27400=REPRESENTATION('material name',(#27421),#55736);
#27401=REPRESENTATION('density',(#27321),#55736);
#27402=DESCRIPTIVE_REPRESENTATION_ITEM('Steel','Steel');
#27403=DESCRIPTIVE_REPRESENTATION_ITEM('Steel','Steel');
#27404=DESCRIPTIVE_REPRESENTATION_ITEM('Steel','Steel');
#27405=DESCRIPTIVE_REPRESENTATION_ITEM('Steel','Steel');
#27406=DESCRIPTIVE_REPRESENTATION_ITEM('Steel','Steel');
#27407=DESCRIPTIVE_REPRESENTATION_ITEM('Steel','Steel');
#27408=DESCRIPTIVE_REPRESENTATION_ITEM('Steel','Steel');
#27409=DESCRIPTIVE_REPRESENTATION_ITEM('Steel','Steel');
#27410=DESCRIPTIVE_REPRESENTATION_ITEM('Steel','Steel');
#27411=DESCRIPTIVE_REPRESENTATION_ITEM('Steel','Steel');
#27412=DESCRIPTIVE_REPRESENTATION_ITEM('Steel','Steel');
#27413=DESCRIPTIVE_REPRESENTATION_ITEM('Steel','Steel');
#27414=DESCRIPTIVE_REPRESENTATION_ITEM('Steel','Steel');
#27415=DESCRIPTIVE_REPRESENTATION_ITEM('Steel','Steel');
#27416=DESCRIPTIVE_REPRESENTATION_ITEM('Steel','Steel');
#27417=DESCRIPTIVE_REPRESENTATION_ITEM('Steel','Steel');
#27418=DESCRIPTIVE_REPRESENTATION_ITEM('Steel','Steel');
#27419=DESCRIPTIVE_REPRESENTATION_ITEM('Steel','Steel');
#27420=DESCRIPTIVE_REPRESENTATION_ITEM('Steel','Steel');
#27421=DESCRIPTIVE_REPRESENTATION_ITEM('Steel','Steel');
#27422=PROPERTY_DEFINITION('material property','material name',#55843);
#27423=PROPERTY_DEFINITION('material property','density of part',#55843);
#27424=PROPERTY_DEFINITION('material property','material name',#55844);
#27425=PROPERTY_DEFINITION('material property','density of part',#55844);
#27426=PROPERTY_DEFINITION('material property','material name',#55845);
#27427=PROPERTY_DEFINITION('material property','density of part',#55845);
#27428=PROPERTY_DEFINITION('material property','material name',#55846);
#27429=PROPERTY_DEFINITION('material property','density of part',#55846);
#27430=PROPERTY_DEFINITION('material property','material name',#55847);
#27431=PROPERTY_DEFINITION('material property','density of part',#55847);
#27432=PROPERTY_DEFINITION('material property','material name',#55848);
#27433=PROPERTY_DEFINITION('material property','density of part',#55848);
#27434=PROPERTY_DEFINITION('material property','material name',#55849);
#27435=PROPERTY_DEFINITION('material property','density of part',#55849);
#27436=PROPERTY_DEFINITION('material property','material name',#55850);
#27437=PROPERTY_DEFINITION('material property','density of part',#55850);
#27438=PROPERTY_DEFINITION('material property','material name',#55851);
#27439=PROPERTY_DEFINITION('material property','density of part',#55851);
#27440=PROPERTY_DEFINITION('material property','material name',#55852);
#27441=PROPERTY_DEFINITION('material property','density of part',#55852);
#27442=PROPERTY_DEFINITION('material property','material name',#55853);
#27443=PROPERTY_DEFINITION('material property','density of part',#55853);
#27444=PROPERTY_DEFINITION('material property','material name',#55854);
#27445=PROPERTY_DEFINITION('material property','density of part',#55854);
#27446=PROPERTY_DEFINITION('material property','material name',#55855);
#27447=PROPERTY_DEFINITION('material property','density of part',#55855);
#27448=PROPERTY_DEFINITION('material property','material name',#55856);
#27449=PROPERTY_DEFINITION('material property','density of part',#55856);
#27450=PROPERTY_DEFINITION('material property','material name',#55857);
#27451=PROPERTY_DEFINITION('material property','density of part',#55857);
#27452=PROPERTY_DEFINITION('material property','material name',#55858);
#27453=PROPERTY_DEFINITION('material property','density of part',#55858);
#27454=PROPERTY_DEFINITION('material property','material name',#55859);
#27455=PROPERTY_DEFINITION('material property','density of part',#55859);
#27456=PROPERTY_DEFINITION('material property','material name',#55860);
#27457=PROPERTY_DEFINITION('material property','density of part',#55860);
#27458=PROPERTY_DEFINITION('material property','material name',#55861);
#27459=PROPERTY_DEFINITION('material property','density of part',#55861);
#27460=PROPERTY_DEFINITION('material property','material name',#55862);
#27461=PROPERTY_DEFINITION('material property','density of part',#55862);
#27462=AXIS2_PLACEMENT_3D('',#37375,#29976,#29977);
#27463=AXIS2_PLACEMENT_3D('',#37376,#29978,#29979);
#27464=AXIS2_PLACEMENT_3D('',#37377,#29980,#29981);
#27465=AXIS2_PLACEMENT_3D('',#37387,#29982,#29983);
#27466=AXIS2_PLACEMENT_3D('',#37389,#29984,#29985);
#27467=AXIS2_PLACEMENT_3D('',#37390,#29986,#29987);
#27468=AXIS2_PLACEMENT_3D('',#37392,#29988,#29989);
#27469=AXIS2_PLACEMENT_3D('',#37412,#29990,#29991);
#27470=AXIS2_PLACEMENT_3D('',#37413,#29992,#29993);
#27471=AXIS2_PLACEMENT_3D('',#37417,#29995,#29996);
#27472=AXIS2_PLACEMENT_3D('',#37419,#29997,#29998);
#27473=AXIS2_PLACEMENT_3D('',#37445,#30000,#30001);
#27474=AXIS2_PLACEMENT_3D('',#37471,#30003,#30004);
#27475=AXIS2_PLACEMENT_3D('',#37491,#30006,#30007);
#27476=AXIS2_PLACEMENT_3D('',#37493,#30008,#30009);
#27477=AXIS2_PLACEMENT_3D('',#37495,#30010,#30011);
#27478=AXIS2_PLACEMENT_3D('',#37497,#30012,#30013);
#27479=AXIS2_PLACEMENT_3D('',#37499,#30014,#30015);
#27480=AXIS2_PLACEMENT_3D('',#37501,#30016,#30017);
#27481=AXIS2_PLACEMENT_3D('',#37502,#30018,#30019);
#27482=AXIS2_PLACEMENT_3D('',#37504,#30020,#30021);
#27483=AXIS2_PLACEMENT_3D('',#37505,#30022,#30023);
#27484=AXIS2_PLACEMENT_3D('',#37506,#30024,#30025);
#27485=AXIS2_PLACEMENT_3D('',#37507,#30026,#30027);
#27486=AXIS2_PLACEMENT_3D('',#37508,#30028,#30029);
#27487=AXIS2_PLACEMENT_3D('',#37510,#30030,#30031);
#27488=AXIS2_PLACEMENT_3D('',#37512,#30032,#30033);
#27489=AXIS2_PLACEMENT_3D('',#37514,#30034,#30035);
#27490=AXIS2_PLACEMENT_3D('',#37516,#30036,#30037);
#27491=AXIS2_PLACEMENT_3D('',#37518,#30038,#30039);
#27492=AXIS2_PLACEMENT_3D('',#37520,#30040,#30041);
#27493=AXIS2_PLACEMENT_3D('',#37522,#30042,#30043);
#27494=AXIS2_PLACEMENT_3D('',#37524,#30044,#30045);
#27495=AXIS2_PLACEMENT_3D('',#37526,#30046,#30047);
#27496=AXIS2_PLACEMENT_3D('',#37527,#30048,#30049);
#27497=AXIS2_PLACEMENT_3D('',#37530,#30050,#30051);
#27498=AXIS2_PLACEMENT_3D('',#37534,#30053,#30054);
#27499=AXIS2_PLACEMENT_3D('',#37547,#30056,#30057);
#27500=AXIS2_PLACEMENT_3D('',#37548,#30058,#30059);
#27501=AXIS2_PLACEMENT_3D('',#37549,#30060,#30061);
#27502=AXIS2_PLACEMENT_3D('',#37550,#30062,#30063);
#27503=AXIS2_PLACEMENT_3D('',#37553,#30064,#30065);
#27504=AXIS2_PLACEMENT_3D('',#37567,#30068,#30069);
#27505=AXIS2_PLACEMENT_3D('',#37568,#30070,#30071);
#27506=AXIS2_PLACEMENT_3D('',#37569,#30072,#30073);
#27507=AXIS2_PLACEMENT_3D('',#37570,#30074,#30075);
#27508=AXIS2_PLACEMENT_3D('',#37573,#30076,#30077);
#27509=AXIS2_PLACEMENT_3D('',#37587,#30080,#30081);
#27510=AXIS2_PLACEMENT_3D('',#37588,#30082,#30083);
#27511=AXIS2_PLACEMENT_3D('',#37589,#30084,#30085);
#27512=AXIS2_PLACEMENT_3D('',#37590,#30086,#30087);
#27513=AXIS2_PLACEMENT_3D('',#37593,#30088,#30089);
#27514=AXIS2_PLACEMENT_3D('',#37605,#30092,#30093);
#27515=AXIS2_PLACEMENT_3D('',#37606,#30094,#30095);
#27516=AXIS2_PLACEMENT_3D('',#37607,#30096,#30097);
#27517=AXIS2_PLACEMENT_3D('',#37611,#30099,#30100);
#27518=AXIS2_PLACEMENT_3D('',#37613,#30102,#30103);
#27519=AXIS2_PLACEMENT_3D('',#37617,#30106,#30107);
#27520=AXIS2_PLACEMENT_3D('',#37620,#30109,#30110);
#27521=AXIS2_PLACEMENT_3D('',#37621,#30111,#30112);
#27522=AXIS2_PLACEMENT_3D('',#37625,#30115,#30116);
#27523=AXIS2_PLACEMENT_3D('',#37627,#30117,#30118);
#27524=AXIS2_PLACEMENT_3D('',#37629,#30119,#30120);
#27525=AXIS2_PLACEMENT_3D('',#37630,#30121,#30122);
#27526=AXIS2_PLACEMENT_3D('',#37633,#30123,#30124);
#27527=AXIS2_PLACEMENT_3D('',#37637,#30126,#30127);
#27528=AXIS2_PLACEMENT_3D('',#37650,#30129,#30130);
#27529=AXIS2_PLACEMENT_3D('',#37651,#30131,#30132);
#27530=AXIS2_PLACEMENT_3D('',#37652,#30133,#30134);
#27531=AXIS2_PLACEMENT_3D('',#37653,#30135,#30136);
#27532=AXIS2_PLACEMENT_3D('',#37655,#30137,#30138);
#27533=AXIS2_PLACEMENT_3D('',#37668,#30141,#30142);
#27534=AXIS2_PLACEMENT_3D('',#37669,#30143,#30144);
#27535=AXIS2_PLACEMENT_3D('',#37670,#30145,#30146);
#27536=AXIS2_PLACEMENT_3D('',#37672,#30147,#30148);
#27537=AXIS2_PLACEMENT_3D('',#37684,#30150,#30151);
#27538=AXIS2_PLACEMENT_3D('',#37685,#30152,#30153);
#27539=AXIS2_PLACEMENT_3D('',#37686,#30154,#30155);
#27540=AXIS2_PLACEMENT_3D('',#37688,#30156,#30157);
#27541=AXIS2_PLACEMENT_3D('',#37699,#30159,#30160);
#27542=AXIS2_PLACEMENT_3D('',#37700,#30161,#30162);
#27543=AXIS2_PLACEMENT_3D('',#37701,#30163,#30164);
#27544=AXIS2_PLACEMENT_3D('',#37703,#30166,#30167);
#27545=AXIS2_PLACEMENT_3D('',#37705,#30169,#30170);
#27546=AXIS2_PLACEMENT_3D('',#37707,#30172,#30173);
#27547=AXIS2_PLACEMENT_3D('',#37710,#30174,#30175);
#27548=AXIS2_PLACEMENT_3D('',#37714,#30177,#30178);
#27549=AXIS2_PLACEMENT_3D('',#37718,#30180,#30181);
#27550=AXIS2_PLACEMENT_3D('',#37722,#30183,#30184);
#27551=AXIS2_PLACEMENT_3D('',#37725,#30186,#30187);
#27552=AXIS2_PLACEMENT_3D('',#37727,#30188,#30189);
#27553=AXIS2_PLACEMENT_3D('',#37728,#30190,#30191);
#27554=AXIS2_PLACEMENT_3D('',#37731,#30192,#30193);
#27555=AXIS2_PLACEMENT_3D('',#37735,#30195,#30196);
#27556=AXIS2_PLACEMENT_3D('',#37748,#30198,#30199);
#27557=AXIS2_PLACEMENT_3D('',#37749,#30200,#30201);
#27558=AXIS2_PLACEMENT_3D('',#37750,#30202,#30203);
#27559=AXIS2_PLACEMENT_3D('',#37751,#30204,#30205);
#27560=AXIS2_PLACEMENT_3D('',#37754,#30206,#30207);
#27561=AXIS2_PLACEMENT_3D('',#37768,#30210,#30211);
#27562=AXIS2_PLACEMENT_3D('',#37769,#30212,#30213);
#27563=AXIS2_PLACEMENT_3D('',#37770,#30214,#30215);
#27564=AXIS2_PLACEMENT_3D('',#37771,#30216,#30217);
#27565=AXIS2_PLACEMENT_3D('',#37774,#30218,#30219);
#27566=AXIS2_PLACEMENT_3D('',#37788,#30222,#30223);
#27567=AXIS2_PLACEMENT_3D('',#37789,#30224,#30225);
#27568=AXIS2_PLACEMENT_3D('',#37790,#30226,#30227);
#27569=AXIS2_PLACEMENT_3D('',#37791,#30228,#30229);
#27570=AXIS2_PLACEMENT_3D('',#37794,#30230,#30231);
#27571=AXIS2_PLACEMENT_3D('',#37806,#30234,#30235);
#27572=AXIS2_PLACEMENT_3D('',#37807,#30236,#30237);
#27573=AXIS2_PLACEMENT_3D('',#37808,#30238,#30239);
#27574=AXIS2_PLACEMENT_3D('',#37812,#30241,#30242);
#27575=AXIS2_PLACEMENT_3D('',#37814,#30244,#30245);
#27576=AXIS2_PLACEMENT_3D('',#37818,#30248,#30249);
#27577=AXIS2_PLACEMENT_3D('',#37821,#30251,#30252);
#27578=AXIS2_PLACEMENT_3D('',#37822,#30253,#30254);
#27579=AXIS2_PLACEMENT_3D('',#37826,#30257,#30258);
#27580=AXIS2_PLACEMENT_3D('',#37828,#30259,#30260);
#27581=AXIS2_PLACEMENT_3D('',#37829,#30261,#30262);
#27582=AXIS2_PLACEMENT_3D('',#37832,#30263,#30264);
#27583=AXIS2_PLACEMENT_3D('',#37836,#30266,#30267);
#27584=AXIS2_PLACEMENT_3D('',#37849,#30269,#30270);
#27585=AXIS2_PLACEMENT_3D('',#37850,#30271,#30272);
#27586=AXIS2_PLACEMENT_3D('',#37851,#30273,#30274);
#27587=AXIS2_PLACEMENT_3D('',#37852,#30275,#30276);
#27588=AXIS2_PLACEMENT_3D('',#37855,#30277,#30278);
#27589=AXIS2_PLACEMENT_3D('',#37869,#30281,#30282);
#27590=AXIS2_PLACEMENT_3D('',#37870,#30283,#30284);
#27591=AXIS2_PLACEMENT_3D('',#37871,#30285,#30286);
#27592=AXIS2_PLACEMENT_3D('',#37872,#30287,#30288);
#27593=AXIS2_PLACEMENT_3D('',#37875,#30289,#30290);
#27594=AXIS2_PLACEMENT_3D('',#37889,#30293,#30294);
#27595=AXIS2_PLACEMENT_3D('',#37890,#30295,#30296);
#27596=AXIS2_PLACEMENT_3D('',#37891,#30297,#30298);
#27597=AXIS2_PLACEMENT_3D('',#37892,#30299,#30300);
#27598=AXIS2_PLACEMENT_3D('',#37895,#30301,#30302);
#27599=AXIS2_PLACEMENT_3D('',#37907,#30305,#30306);
#27600=AXIS2_PLACEMENT_3D('',#37908,#30307,#30308);
#27601=AXIS2_PLACEMENT_3D('',#37909,#30309,#30310);
#27602=AXIS2_PLACEMENT_3D('',#37913,#30312,#30313);
#27603=AXIS2_PLACEMENT_3D('',#37915,#30315,#30316);
#27604=AXIS2_PLACEMENT_3D('',#37919,#30319,#30320);
#27605=AXIS2_PLACEMENT_3D('',#37922,#30322,#30323);
#27606=AXIS2_PLACEMENT_3D('',#37923,#30324,#30325);
#27607=AXIS2_PLACEMENT_3D('',#37927,#30328,#30329);
#27608=AXIS2_PLACEMENT_3D('',#37929,#30330,#30331);
#27609=AXIS2_PLACEMENT_3D('',#37930,#30332,#30333);
#27610=AXIS2_PLACEMENT_3D('',#37932,#30334,#30335);
#27611=AXIS2_PLACEMENT_3D('',#37933,#30336,#30337);
#27612=AXIS2_PLACEMENT_3D('',#37934,#30338,#30339);
#27613=AXIS2_PLACEMENT_3D('',#37938,#30341,#30342);
#27614=AXIS2_PLACEMENT_3D('',#37953,#30344,#30345);
#27615=AXIS2_PLACEMENT_3D('',#37967,#30347,#30348);
#27616=AXIS2_PLACEMENT_3D('',#37968,#30349,#30350);
#27617=AXIS2_PLACEMENT_3D('',#37970,#30351,#30352);
#27618=AXIS2_PLACEMENT_3D('',#37972,#30353,#30354);
#27619=AXIS2_PLACEMENT_3D('',#37973,#30355,#30356);
#27620=AXIS2_PLACEMENT_3D('',#37974,#30357,#30358);
#27621=AXIS2_PLACEMENT_3D('',#37979,#30361,#30362);
#27622=AXIS2_PLACEMENT_3D('',#37980,#30363,#30364);
#27623=AXIS2_PLACEMENT_3D('',#37983,#30366,#30367);
#27624=AXIS2_PLACEMENT_3D('',#37984,#30368,#30369);
#27625=AXIS2_PLACEMENT_3D('',#38001,#30371,#30372);
#27626=AXIS2_PLACEMENT_3D('',#38003,#30373,#30374);
#27627=AXIS2_PLACEMENT_3D('',#38018,#30375,#30376);
#27628=AXIS2_PLACEMENT_3D('',#38020,#30378,#30379);
#27629=AXIS2_PLACEMENT_3D('',#38024,#30382,#30383);
#27630=AXIS2_PLACEMENT_3D('',#38027,#30385,#30386);
#27631=AXIS2_PLACEMENT_3D('',#38028,#30387,#30388);
#27632=AXIS2_PLACEMENT_3D('',#38030,#30390,#30391);
#27633=AXIS2_PLACEMENT_3D('',#38033,#30392,#30393);
#27634=AXIS2_PLACEMENT_3D('',#38035,#30394,#30395);
#27635=AXIS2_PLACEMENT_3D('',#38037,#30396,#30397);
#27636=AXIS2_PLACEMENT_3D('',#38039,#30398,#30399);
#27637=AXIS2_PLACEMENT_3D('',#38040,#30400,#30401);
#27638=AXIS2_PLACEMENT_3D('',#38091,#30402,#30403);
#27639=AXIS2_PLACEMENT_3D('',#38108,#30404,#30405);
#27640=AXIS2_PLACEMENT_3D('',#38111,#30406,#30407);
#27641=AXIS2_PLACEMENT_3D('',#38112,#30408,#30409);
#27642=AXIS2_PLACEMENT_3D('',#38113,#30410,#30411);
#27643=AXIS2_PLACEMENT_3D('',#38178,#30412,#30413);
#27644=AXIS2_PLACEMENT_3D('',#38182,#30415,#30416);
#27645=AXIS2_PLACEMENT_3D('',#38186,#30418,#30419);
#27646=AXIS2_PLACEMENT_3D('',#38188,#30421,#30422);
#27647=AXIS2_PLACEMENT_3D('',#38192,#30425,#30426);
#27648=AXIS2_PLACEMENT_3D('',#38195,#30428,#30429);
#27649=AXIS2_PLACEMENT_3D('',#38196,#30430,#30431);
#27650=AXIS2_PLACEMENT_3D('',#38200,#30433,#30434);
#27651=AXIS2_PLACEMENT_3D('',#38202,#30436,#30437);
#27652=AXIS2_PLACEMENT_3D('',#38205,#30438,#30439);
#27653=AXIS2_PLACEMENT_3D('',#38209,#30441,#30442);
#27654=AXIS2_PLACEMENT_3D('',#38211,#30444,#30445);
#27655=AXIS2_PLACEMENT_3D('',#38214,#30446,#30447);
#27656=AXIS2_PLACEMENT_3D('',#38215,#30448,#30449);
#27657=AXIS2_PLACEMENT_3D('',#38216,#30450,#30451);
#27658=AXIS2_PLACEMENT_3D('',#38217,#30452,#30453);
#27659=AXIS2_PLACEMENT_3D('',#38220,#30456,#30457);
#27660=AXIS2_PLACEMENT_3D('',#38221,#30458,#30459);
#27661=AXIS2_PLACEMENT_3D('',#38222,#30460,#30461);
#27662=AXIS2_PLACEMENT_3D('',#38223,#30462,#30463);
#27663=AXIS2_PLACEMENT_3D('',#38227,#30465,#30466);
#27664=AXIS2_PLACEMENT_3D('',#38241,#30469,#30470);
#27665=AXIS2_PLACEMENT_3D('',#38244,#30473,#30474);
#27666=AXIS2_PLACEMENT_3D('',#38245,#30475,#30476);
#27667=AXIS2_PLACEMENT_3D('',#38248,#30477,#30478);
#27668=AXIS2_PLACEMENT_3D('',#38251,#30480,#30481);
#27669=AXIS2_PLACEMENT_3D('',#38253,#30483,#30484);
#27670=AXIS2_PLACEMENT_3D('',#38255,#30485,#30486);
#27671=AXIS2_PLACEMENT_3D('',#38256,#30487,#30488);
#27672=AXIS2_PLACEMENT_3D('',#38257,#30489,#30490);
#27673=AXIS2_PLACEMENT_3D('',#38259,#30491,#30492);
#27674=AXIS2_PLACEMENT_3D('',#38261,#30494,#30495);
#27675=AXIS2_PLACEMENT_3D('',#38263,#30496,#30497);
#27676=AXIS2_PLACEMENT_3D('',#38264,#30498,#30499);
#27677=AXIS2_PLACEMENT_3D('',#38265,#30500,#30501);
#27678=AXIS2_PLACEMENT_3D('',#38267,#30502,#30503);
#27679=AXIS2_PLACEMENT_3D('',#38269,#30505,#30506);
#27680=AXIS2_PLACEMENT_3D('',#38272,#30507,#30508);
#27681=AXIS2_PLACEMENT_3D('',#38273,#30509,#30510);
#27682=AXIS2_PLACEMENT_3D('',#38274,#30511,#30512);
#27683=AXIS2_PLACEMENT_3D('',#38275,#30513,#30514);
#27684=AXIS2_PLACEMENT_3D('',#38278,#30515,#30516);
#27685=AXIS2_PLACEMENT_3D('',#38281,#30519,#30520);
#27686=AXIS2_PLACEMENT_3D('',#38282,#30521,#30522);
#27687=AXIS2_PLACEMENT_3D('',#38283,#30523,#30524);
#27688=AXIS2_PLACEMENT_3D('',#38284,#30525,#30526);
#27689=AXIS2_PLACEMENT_3D('',#38287,#30528,#30529);
#27690=AXIS2_PLACEMENT_3D('',#38288,#30530,#30531);
#27691=AXIS2_PLACEMENT_3D('',#38290,#30532,#30533);
#27692=AXIS2_PLACEMENT_3D('',#38294,#30535,#30536);
#27693=AXIS2_PLACEMENT_3D('',#38297,#30538,#30539);
#27694=AXIS2_PLACEMENT_3D('',#38301,#30541,#30542);
#27695=AXIS2_PLACEMENT_3D('',#38304,#30544,#30545);
#27696=AXIS2_PLACEMENT_3D('',#38305,#30546,#30547);
#27697=AXIS2_PLACEMENT_3D('',#38307,#30548,#30549);
#27698=AXIS2_PLACEMENT_3D('',#38309,#30550,#30551);
#27699=AXIS2_PLACEMENT_3D('',#38311,#30552,#30553);
#27700=AXIS2_PLACEMENT_3D('',#38312,#30554,#30555);
#27701=AXIS2_PLACEMENT_3D('',#38368,#30556,#30557);
#27702=AXIS2_PLACEMENT_3D('',#38378,#30558,#30559);
#27703=AXIS2_PLACEMENT_3D('',#38381,#30560,#30561);
#27704=AXIS2_PLACEMENT_3D('',#38382,#30562,#30563);
#27705=AXIS2_PLACEMENT_3D('',#38383,#30564,#30565);
#27706=AXIS2_PLACEMENT_3D('',#38448,#30566,#30567);
#27707=AXIS2_PLACEMENT_3D('',#38451,#30570,#30571);
#27708=AXIS2_PLACEMENT_3D('',#38454,#30573,#30574);
#27709=AXIS2_PLACEMENT_3D('',#38455,#30575,#30576);
#27710=AXIS2_PLACEMENT_3D('',#38457,#30578,#30579);
#27711=AXIS2_PLACEMENT_3D('',#38459,#30581,#30582);
#27712=AXIS2_PLACEMENT_3D('',#38462,#30584,#30585);
#27713=AXIS2_PLACEMENT_3D('',#38463,#30586,#30587);
#27714=AXIS2_PLACEMENT_3D('',#38464,#30588,#30589);
#27715=AXIS2_PLACEMENT_3D('',#38467,#30591,#30592);
#27716=AXIS2_PLACEMENT_3D('',#38468,#30593,#30594);
#27717=AXIS2_PLACEMENT_3D('',#38469,#30595,#30596);
#27718=AXIS2_PLACEMENT_3D('',#38472,#30598,#30599);
#27719=AXIS2_PLACEMENT_3D('',#38473,#30600,#30601);
#27720=AXIS2_PLACEMENT_3D('',#38474,#30602,#30603);
#27721=AXIS2_PLACEMENT_3D('',#38475,#30604,#30605);
#27722=AXIS2_PLACEMENT_3D('',#38476,#30606,#30607);
#27723=AXIS2_PLACEMENT_3D('',#38477,#30608,#30609);
#27724=AXIS2_PLACEMENT_3D('',#38481,#30612,#30613);
#27725=AXIS2_PLACEMENT_3D('',#38484,#30615,#30616);
#27726=AXIS2_PLACEMENT_3D('',#38485,#30617,#30618);
#27727=AXIS2_PLACEMENT_3D('',#38486,#30619,#30620);
#27728=AXIS2_PLACEMENT_3D('',#38489,#30622,#30623);
#27729=AXIS2_PLACEMENT_3D('',#38490,#30624,#30625);
#27730=AXIS2_PLACEMENT_3D('',#38491,#30626,#30627);
#27731=AXIS2_PLACEMENT_3D('',#38494,#30629,#30630);
#27732=AXIS2_PLACEMENT_3D('',#38495,#30631,#30632);
#27733=AXIS2_PLACEMENT_3D('',#38496,#30633,#30634);
#27734=AXIS2_PLACEMENT_3D('',#38499,#30636,#30637);
#27735=AXIS2_PLACEMENT_3D('',#38500,#30638,#30639);
#27736=AXIS2_PLACEMENT_3D('',#38501,#30640,#30641);
#27737=AXIS2_PLACEMENT_3D('',#38504,#30643,#30644);
#27738=AXIS2_PLACEMENT_3D('',#38505,#30645,#30646);
#27739=AXIS2_PLACEMENT_3D('',#38506,#30647,#30648);
#27740=AXIS2_PLACEMENT_3D('',#38509,#30650,#30651);
#27741=AXIS2_PLACEMENT_3D('',#38510,#30652,#30653);
#27742=AXIS2_PLACEMENT_3D('',#38511,#30654,#30655);
#27743=AXIS2_PLACEMENT_3D('',#38514,#30657,#30658);
#27744=AXIS2_PLACEMENT_3D('',#38515,#30659,#30660);
#27745=AXIS2_PLACEMENT_3D('',#38516,#30661,#30662);
#27746=AXIS2_PLACEMENT_3D('',#38519,#30664,#30665);
#27747=AXIS2_PLACEMENT_3D('',#38520,#30666,#30667);
#27748=AXIS2_PLACEMENT_3D('',#38521,#30668,#30669);
#27749=AXIS2_PLACEMENT_3D('',#38524,#30671,#30672);
#27750=AXIS2_PLACEMENT_3D('',#38525,#30673,#30674);
#27751=AXIS2_PLACEMENT_3D('',#38526,#30675,#30676);
#27752=AXIS2_PLACEMENT_3D('',#38529,#30678,#30679);
#27753=AXIS2_PLACEMENT_3D('',#38530,#30680,#30681);
#27754=AXIS2_PLACEMENT_3D('',#38531,#30682,#30683);
#27755=AXIS2_PLACEMENT_3D('',#38534,#30685,#30686);
#27756=AXIS2_PLACEMENT_3D('',#38535,#30687,#30688);
#27757=AXIS2_PLACEMENT_3D('',#38536,#30689,#30690);
#27758=AXIS2_PLACEMENT_3D('',#38539,#30692,#30693);
#27759=AXIS2_PLACEMENT_3D('',#38540,#30694,#30695);
#27760=AXIS2_PLACEMENT_3D('',#38541,#30696,#30697);
#27761=AXIS2_PLACEMENT_3D('',#38542,#30698,#30699);
#27762=AXIS2_PLACEMENT_3D('',#38544,#30700,#30701);
#27763=AXIS2_PLACEMENT_3D('',#38545,#30702,#30703);
#27764=AXIS2_PLACEMENT_3D('',#38547,#30705,#30706);
#27765=AXIS2_PLACEMENT_3D('',#38549,#30708,#30709);
#27766=AXIS2_PLACEMENT_3D('',#38551,#30711,#30712);
#27767=AXIS2_PLACEMENT_3D('',#38553,#30714,#30715);
#27768=AXIS2_PLACEMENT_3D('',#38554,#30716,#30717);
#27769=AXIS2_PLACEMENT_3D('',#38556,#30719,#30720);
#27770=AXIS2_PLACEMENT_3D('',#38558,#30722,#30723);
#27771=AXIS2_PLACEMENT_3D('',#38560,#30725,#30726);
#27772=AXIS2_PLACEMENT_3D('',#38561,#30727,#30728);
#27773=AXIS2_PLACEMENT_3D('',#38562,#30729,#30730);
#27774=AXIS2_PLACEMENT_3D('',#38565,#30733,#30734);
#27775=AXIS2_PLACEMENT_3D('',#38567,#30736,#30737);
#27776=AXIS2_PLACEMENT_3D('',#38569,#30739,#30740);
#27777=AXIS2_PLACEMENT_3D('',#38571,#30742,#30743);
#27778=AXIS2_PLACEMENT_3D('',#38573,#30745,#30746);
#27779=AXIS2_PLACEMENT_3D('',#38575,#30748,#30749);
#27780=AXIS2_PLACEMENT_3D('',#38577,#30751,#30752);
#27781=AXIS2_PLACEMENT_3D('',#38578,#30753,#30754);
#27782=AXIS2_PLACEMENT_3D('',#38581,#30756,#30757);
#27783=AXIS2_PLACEMENT_3D('',#38582,#30758,#30759);
#27784=AXIS2_PLACEMENT_3D('',#38584,#30761,#30762);
#27785=AXIS2_PLACEMENT_3D('',#38585,#30763,#30764);
#27786=AXIS2_PLACEMENT_3D('',#38768,#30767,#30768);
#27787=AXIS2_PLACEMENT_3D('',#38774,#30772,#30773);
#27788=AXIS2_PLACEMENT_3D('',#38782,#30777,#30778);
#27789=AXIS2_PLACEMENT_3D('',#38784,#30779,#30780);
#27790=AXIS2_PLACEMENT_3D('',#38786,#30782,#30783);
#27791=AXIS2_PLACEMENT_3D('',#38852,#30785,#30786);
#27792=AXIS2_PLACEMENT_3D('',#38977,#30790,#30791);
#27793=AXIS2_PLACEMENT_3D('',#38981,#30794,#30795);
#27794=AXIS2_PLACEMENT_3D('',#38994,#30797,#30798);
#27795=AXIS2_PLACEMENT_3D('',#39180,#30803,#30804);
#27796=AXIS2_PLACEMENT_3D('',#39186,#30808,#30809);
#27797=AXIS2_PLACEMENT_3D('',#39192,#30812,#30813);
#27798=AXIS2_PLACEMENT_3D('',#39194,#30815,#30816);
#27799=AXIS2_PLACEMENT_3D('',#39197,#30818,#30819);
#27800=AXIS2_PLACEMENT_3D('',#39198,#30820,#30821);
#27801=AXIS2_PLACEMENT_3D('',#39384,#30826,#30827);
#27802=AXIS2_PLACEMENT_3D('',#39390,#30831,#30832);
#27803=AXIS2_PLACEMENT_3D('',#39398,#30836,#30837);
#27804=AXIS2_PLACEMENT_3D('',#39400,#30839,#30840);
#27805=AXIS2_PLACEMENT_3D('',#39465,#30842,#30843);
#27806=AXIS2_PLACEMENT_3D('',#39585,#30847,#30848);
#27807=AXIS2_PLACEMENT_3D('',#39589,#30851,#30852);
#27808=AXIS2_PLACEMENT_3D('',#39602,#30854,#30855);
#27809=AXIS2_PLACEMENT_3D('',#39794,#30860,#30861);
#27810=AXIS2_PLACEMENT_3D('',#39800,#30865,#30866);
#27811=AXIS2_PLACEMENT_3D('',#39808,#30870,#30871);
#27812=AXIS2_PLACEMENT_3D('',#39810,#30873,#30874);
#27813=AXIS2_PLACEMENT_3D('',#39876,#30876,#30877);
#27814=AXIS2_PLACEMENT_3D('',#40001,#30881,#30882);
#27815=AXIS2_PLACEMENT_3D('',#40005,#30885,#30886);
#27816=AXIS2_PLACEMENT_3D('',#40018,#30888,#30889);
#27817=AXIS2_PLACEMENT_3D('',#40022,#30892,#30893);
#27818=AXIS2_PLACEMENT_3D('',#40024,#30894,#30895);
#27819=AXIS2_PLACEMENT_3D('',#40026,#30896,#30897);
#27820=AXIS2_PLACEMENT_3D('',#40027,#30898,#30899);
#27821=AXIS2_PLACEMENT_3D('',#40028,#30900,#30901);
#27822=AXIS2_PLACEMENT_3D('',#40031,#30903,#30904);
#27823=AXIS2_PLACEMENT_3D('',#40032,#30905,#30906);
#27824=AXIS2_PLACEMENT_3D('',#40034,#30907,#30908);
#27825=AXIS2_PLACEMENT_3D('',#40036,#30910,#30911);
#27826=AXIS2_PLACEMENT_3D('',#40038,#30912,#30913);
#27827=AXIS2_PLACEMENT_3D('',#40039,#30914,#30915);
#27828=AXIS2_PLACEMENT_3D('',#40040,#30916,#30917);
#27829=AXIS2_PLACEMENT_3D('',#40042,#30918,#30919);
#27830=AXIS2_PLACEMENT_3D('',#40044,#30920,#30921);
#27831=AXIS2_PLACEMENT_3D('',#40046,#30922,#30923);
#27832=AXIS2_PLACEMENT_3D('',#40048,#30924,#30925);
#27833=AXIS2_PLACEMENT_3D('',#40050,#30926,#30927);
#27834=AXIS2_PLACEMENT_3D('',#40052,#30928,#30929);
#27835=AXIS2_PLACEMENT_3D('',#40054,#30930,#30931);
#27836=AXIS2_PLACEMENT_3D('',#40056,#30932,#30933);
#27837=AXIS2_PLACEMENT_3D('',#40060,#30935,#30936);
#27838=AXIS2_PLACEMENT_3D('',#40063,#30938,#30939);
#27839=AXIS2_PLACEMENT_3D('',#40066,#30941,#30942);
#27840=AXIS2_PLACEMENT_3D('',#40069,#30944,#30945);
#27841=AXIS2_PLACEMENT_3D('',#40072,#30947,#30948);
#27842=AXIS2_PLACEMENT_3D('',#40073,#30949,#30950);
#27843=AXIS2_PLACEMENT_3D('',#40086,#30952,#30953);
#27844=AXIS2_PLACEMENT_3D('',#40088,#30955,#30956);
#27845=AXIS2_PLACEMENT_3D('',#40101,#30958,#30959);
#27846=AXIS2_PLACEMENT_3D('',#40103,#30961,#30962);
#27847=AXIS2_PLACEMENT_3D('',#40105,#30963,#30964);
#27848=AXIS2_PLACEMENT_3D('',#40106,#30965,#30966);
#27849=AXIS2_PLACEMENT_3D('',#40107,#30967,#30968);
#27850=AXIS2_PLACEMENT_3D('',#40110,#30969,#30970);
#27851=AXIS2_PLACEMENT_3D('',#40112,#30971,#30972);
#27852=AXIS2_PLACEMENT_3D('',#40114,#30973,#30974);
#27853=AXIS2_PLACEMENT_3D('',#40116,#30975,#30976);
#27854=AXIS2_PLACEMENT_3D('',#40118,#30977,#30978);
#27855=AXIS2_PLACEMENT_3D('',#40120,#30979,#30980);
#27856=AXIS2_PLACEMENT_3D('',#40122,#30981,#30982);
#27857=AXIS2_PLACEMENT_3D('',#40124,#30983,#30984);
#27858=AXIS2_PLACEMENT_3D('',#40126,#30985,#30986);
#27859=AXIS2_PLACEMENT_3D('',#40128,#30987,#30988);
#27860=AXIS2_PLACEMENT_3D('',#40130,#30989,#30990);
#27861=AXIS2_PLACEMENT_3D('',#40132,#30991,#30992);
#27862=AXIS2_PLACEMENT_3D('',#40134,#30993,#30994);
#27863=AXIS2_PLACEMENT_3D('',#40136,#30995,#30996);
#27864=AXIS2_PLACEMENT_3D('',#40138,#30997,#30998);
#27865=AXIS2_PLACEMENT_3D('',#40140,#30999,#31000);
#27866=AXIS2_PLACEMENT_3D('',#40142,#31001,#31002);
#27867=AXIS2_PLACEMENT_3D('',#40144,#31003,#31004);
#27868=AXIS2_PLACEMENT_3D('',#40146,#31005,#31006);
#27869=AXIS2_PLACEMENT_3D('',#40148,#31007,#31008);
#27870=AXIS2_PLACEMENT_3D('',#40150,#31009,#31010);
#27871=AXIS2_PLACEMENT_3D('',#40152,#31011,#31012);
#27872=AXIS2_PLACEMENT_3D('',#40154,#31013,#31014);
#27873=AXIS2_PLACEMENT_3D('',#40156,#31015,#31016);
#27874=AXIS2_PLACEMENT_3D('',#40157,#31017,#31018);
#27875=AXIS2_PLACEMENT_3D('',#40158,#31019,#31020);
#27876=AXIS2_PLACEMENT_3D('',#40160,#31021,#31022);
#27877=AXIS2_PLACEMENT_3D('',#40162,#31023,#31024);
#27878=AXIS2_PLACEMENT_3D('',#40163,#31025,#31026);
#27879=AXIS2_PLACEMENT_3D('',#40164,#31027,#31028);
#27880=AXIS2_PLACEMENT_3D('',#40166,#31029,#31030);
#27881=AXIS2_PLACEMENT_3D('',#40168,#31032,#31033);
#27882=AXIS2_PLACEMENT_3D('',#40479,#31075,#31076);
#27883=AXIS2_PLACEMENT_3D('',#40492,#31078,#31079);
#27884=AXIS2_PLACEMENT_3D('',#40494,#31080,#31081);
#27885=AXIS2_PLACEMENT_3D('',#40496,#31083,#31084);
#27886=AXIS2_PLACEMENT_3D('',#40497,#31085,#31086);
#27887=AXIS2_PLACEMENT_3D('',#40498,#31087,#31088);
#27888=AXIS2_PLACEMENT_3D('',#40511,#31090,#31091);
#27889=AXIS2_PLACEMENT_3D('',#40513,#31093,#31094);
#27890=AXIS2_PLACEMENT_3D('',#40515,#31095,#31096);
#27891=AXIS2_PLACEMENT_3D('',#40516,#31097,#31098);
#27892=AXIS2_PLACEMENT_3D('',#40517,#31099,#31100);
#27893=AXIS2_PLACEMENT_3D('',#40532,#31104,#31105);
#27894=AXIS2_PLACEMENT_3D('',#40534,#31107,#31108);
#27895=AXIS2_PLACEMENT_3D('',#40535,#31109,#31110);
#27896=AXIS2_PLACEMENT_3D('',#40538,#31111,#31112);
#27897=AXIS2_PLACEMENT_3D('',#40555,#31113,#31114);
#27898=AXIS2_PLACEMENT_3D('',#40570,#31115,#31116);
#27899=AXIS2_PLACEMENT_3D('',#40585,#31119,#31120);
#27900=AXIS2_PLACEMENT_3D('',#40600,#31123,#31124);
#27901=AXIS2_PLACEMENT_3D('',#40601,#31125,#31126);
#27902=AXIS2_PLACEMENT_3D('',#40602,#31127,#31128);
#27903=AXIS2_PLACEMENT_3D('',#40605,#31129,#31130);
#27904=AXIS2_PLACEMENT_3D('',#40606,#31131,#31132);
#27905=AXIS2_PLACEMENT_3D('',#40608,#31133,#31134);
#27906=AXIS2_PLACEMENT_3D('',#40609,#31135,#31136);
#27907=AXIS2_PLACEMENT_3D('',#40610,#31137,#31138);
#27908=AXIS2_PLACEMENT_3D('',#40614,#31140,#31141);
#27909=AXIS2_PLACEMENT_3D('',#40617,#31143,#31144);
#27910=AXIS2_PLACEMENT_3D('',#40619,#31146,#31147);
#27911=AXIS2_PLACEMENT_3D('',#40641,#31148,#31149);
#27912=AXIS2_PLACEMENT_3D('',#40643,#31150,#31151);
#27913=AXIS2_PLACEMENT_3D('',#40644,#31152,#31153);
#27914=AXIS2_PLACEMENT_3D('',#40657,#31154,#31155);
#27915=AXIS2_PLACEMENT_3D('',#40659,#31157,#31158);
#27916=AXIS2_PLACEMENT_3D('',#40661,#31160,#31161);
#27917=AXIS2_PLACEMENT_3D('',#40663,#31163,#31164);
#27918=AXIS2_PLACEMENT_3D('',#40665,#31166,#31167);
#27919=AXIS2_PLACEMENT_3D('',#40667,#31168,#31169);
#27920=AXIS2_PLACEMENT_3D('',#40669,#31171,#31172);
#27921=AXIS2_PLACEMENT_3D('',#40671,#31173,#31174);
#27922=AXIS2_PLACEMENT_3D('',#40673,#31175,#31176);
#27923=AXIS2_PLACEMENT_3D('',#40675,#31178,#31179);
#27924=AXIS2_PLACEMENT_3D('',#40677,#31180,#31181);
#27925=AXIS2_PLACEMENT_3D('',#40679,#31182,#31183);
#27926=AXIS2_PLACEMENT_3D('',#40681,#31185,#31186);
#27927=AXIS2_PLACEMENT_3D('',#40683,#31187,#31188);
#27928=AXIS2_PLACEMENT_3D('',#40685,#31189,#31190);
#27929=AXIS2_PLACEMENT_3D('',#40687,#31192,#31193);
#27930=AXIS2_PLACEMENT_3D('',#40689,#31194,#31195);
#27931=AXIS2_PLACEMENT_3D('',#40691,#31196,#31197);
#27932=AXIS2_PLACEMENT_3D('',#40693,#31198,#31199);
#27933=AXIS2_PLACEMENT_3D('',#40695,#31201,#31202);
#27934=AXIS2_PLACEMENT_3D('',#40697,#31203,#31204);
#27935=AXIS2_PLACEMENT_3D('',#40699,#31205,#31206);
#27936=AXIS2_PLACEMENT_3D('',#40701,#31208,#31209);
#27937=AXIS2_PLACEMENT_3D('',#40707,#31213,#31214);
#27938=AXIS2_PLACEMENT_3D('',#40711,#31217,#31218);
#27939=AXIS2_PLACEMENT_3D('',#40713,#31220,#31221);
#27940=AXIS2_PLACEMENT_3D('',#40715,#31223,#31224);
#27941=AXIS2_PLACEMENT_3D('',#40724,#31230,#31231);
#27942=AXIS2_PLACEMENT_3D('',#40726,#31233,#31234);
#27943=AXIS2_PLACEMENT_3D('',#40727,#31235,#31236);
#27944=AXIS2_PLACEMENT_3D('',#40733,#31240,#31241);
#27945=AXIS2_PLACEMENT_3D('',#40737,#31244,#31245);
#27946=AXIS2_PLACEMENT_3D('',#40741,#31248,#31249);
#27947=AXIS2_PLACEMENT_3D('',#40745,#31252,#31253);
#27948=AXIS2_PLACEMENT_3D('',#40749,#31256,#31257);
#27949=AXIS2_PLACEMENT_3D('',#40753,#31260,#31261);
#27950=AXIS2_PLACEMENT_3D('',#40757,#31264,#31265);
#27951=AXIS2_PLACEMENT_3D('',#40761,#31268,#31269);
#27952=AXIS2_PLACEMENT_3D('',#40763,#31271,#31272);
#27953=AXIS2_PLACEMENT_3D('',#40767,#31275,#31276);
#27954=AXIS2_PLACEMENT_3D('',#40769,#31278,#31279);
#27955=AXIS2_PLACEMENT_3D('',#40882,#31291,#31292);
#27956=AXIS2_PLACEMENT_3D('',#40884,#31294,#31295);
#27957=AXIS2_PLACEMENT_3D('',#40897,#31298,#31299);
#27958=AXIS2_PLACEMENT_3D('',#41043,#31314,#31315);
#27959=AXIS2_PLACEMENT_3D('',#41245,#31336,#31337);
#27960=AXIS2_PLACEMENT_3D('',#41269,#31341,#31342);
#27961=AXIS2_PLACEMENT_3D('',#41270,#31343,#31344);
#27962=AXIS2_PLACEMENT_3D('',#41320,#31352,#31353);
#27963=AXIS2_PLACEMENT_3D('',#41322,#31355,#31356);
#27964=AXIS2_PLACEMENT_3D('',#41403,#31366,#31367);
#27965=AXIS2_PLACEMENT_3D('',#41405,#31369,#31370);
#27966=AXIS2_PLACEMENT_3D('',#41409,#31373,#31374);
#27967=AXIS2_PLACEMENT_3D('',#41411,#31376,#31377);
#27968=AXIS2_PLACEMENT_3D('',#41412,#31378,#31379);
#27969=AXIS2_PLACEMENT_3D('',#41418,#31383,#31384);
#27970=AXIS2_PLACEMENT_3D('',#41422,#31387,#31388);
#27971=AXIS2_PLACEMENT_3D('',#41448,#31393,#31394);
#27972=AXIS2_PLACEMENT_3D('',#41452,#31397,#31398);
#27973=AXIS2_PLACEMENT_3D('',#41456,#31401,#31402);
#27974=AXIS2_PLACEMENT_3D('',#41460,#31405,#31406);
#27975=AXIS2_PLACEMENT_3D('',#41464,#31409,#31410);
#27976=AXIS2_PLACEMENT_3D('',#41468,#31413,#31414);
#27977=AXIS2_PLACEMENT_3D('',#41470,#31416,#31417);
#27978=AXIS2_PLACEMENT_3D('',#41471,#31418,#31419);
#27979=AXIS2_PLACEMENT_3D('',#41473,#31421,#31422);
#27980=AXIS2_PLACEMENT_3D('',#41475,#31424,#31425);
#27981=AXIS2_PLACEMENT_3D('',#41477,#31427,#31428);
#27982=AXIS2_PLACEMENT_3D('',#41479,#31430,#31431);
#27983=AXIS2_PLACEMENT_3D('',#41480,#31432,#31433);
#27984=AXIS2_PLACEMENT_3D('',#41484,#31435,#31436);
#27985=AXIS2_PLACEMENT_3D('',#41486,#31438,#31439);
#27986=AXIS2_PLACEMENT_3D('',#41488,#31441,#31442);
#27987=AXIS2_PLACEMENT_3D('',#41490,#31444,#31445);
#27988=AXIS2_PLACEMENT_3D('',#41491,#31446,#31447);
#27989=AXIS2_PLACEMENT_3D('',#41492,#31448,#31449);
#27990=AXIS2_PLACEMENT_3D('',#41493,#31450,#31451);
#27991=AXIS2_PLACEMENT_3D('',#41495,#31452,#31453);
#27992=AXIS2_PLACEMENT_3D('',#41498,#31455,#31456);
#27993=AXIS2_PLACEMENT_3D('',#41499,#31457,#31458);
#27994=AXIS2_PLACEMENT_3D('',#41501,#31459,#31460);
#27995=AXIS2_PLACEMENT_3D('',#41503,#31462,#31463);
#27996=AXIS2_PLACEMENT_3D('',#41506,#31464,#31465);
#27997=AXIS2_PLACEMENT_3D('',#41510,#31467,#31468);
#27998=AXIS2_PLACEMENT_3D('',#41514,#31470,#31471);
#27999=AXIS2_PLACEMENT_3D('',#41518,#31473,#31474);
#28000=AXIS2_PLACEMENT_3D('',#41520,#31476,#31477);
#28001=AXIS2_PLACEMENT_3D('',#41523,#31479,#31480);
#28002=AXIS2_PLACEMENT_3D('',#41524,#31481,#31482);
#28003=AXIS2_PLACEMENT_3D('',#41526,#31483,#31484);
#28004=AXIS2_PLACEMENT_3D('',#41527,#31485,#31486);
#28005=AXIS2_PLACEMENT_3D('',#41529,#31487,#31488);
#28006=AXIS2_PLACEMENT_3D('',#41532,#31490,#31491);
#28007=AXIS2_PLACEMENT_3D('',#41533,#31492,#31493);
#28008=AXIS2_PLACEMENT_3D('',#41536,#31494,#31495);
#28009=AXIS2_PLACEMENT_3D('',#41540,#31497,#31498);
#28010=AXIS2_PLACEMENT_3D('',#41544,#31500,#31501);
#28011=AXIS2_PLACEMENT_3D('',#41552,#31505,#31506);
#28012=AXIS2_PLACEMENT_3D('',#41555,#31508,#31509);
#28013=AXIS2_PLACEMENT_3D('',#41560,#31511,#31512);
#28014=AXIS2_PLACEMENT_3D('',#41564,#31514,#31515);
#28015=AXIS2_PLACEMENT_3D('',#41568,#31517,#31518);
#28016=AXIS2_PLACEMENT_3D('',#41571,#31520,#31521);
#28017=AXIS2_PLACEMENT_3D('',#41572,#31522,#31523);
#28018=AXIS2_PLACEMENT_3D('',#41575,#31525,#31526);
#28019=AXIS2_PLACEMENT_3D('',#41576,#31527,#31528);
#28020=AXIS2_PLACEMENT_3D('',#41579,#31530,#31531);
#28021=AXIS2_PLACEMENT_3D('',#41580,#31532,#31533);
#28022=AXIS2_PLACEMENT_3D('',#41583,#31535,#31536);
#28023=AXIS2_PLACEMENT_3D('',#41584,#31537,#31538);
#28024=AXIS2_PLACEMENT_3D('',#41589,#31540,#31541);
#28025=AXIS2_PLACEMENT_3D('',#41592,#31543,#31544);
#28026=AXIS2_PLACEMENT_3D('',#41622,#31545,#31546);
#28027=AXIS2_PLACEMENT_3D('',#41626,#31548,#31549);
#28028=AXIS2_PLACEMENT_3D('',#41631,#31552,#31553);
#28029=AXIS2_PLACEMENT_3D('',#41635,#31555,#31556);
#28030=AXIS2_PLACEMENT_3D('',#41647,#31562,#31563);
#28031=AXIS2_PLACEMENT_3D('',#41651,#31565,#31566);
#28032=AXIS2_PLACEMENT_3D('',#41655,#31568,#31569);
#28033=AXIS2_PLACEMENT_3D('',#41658,#31571,#31572);
#28034=AXIS2_PLACEMENT_3D('',#41659,#31573,#31574);
#28035=AXIS2_PLACEMENT_3D('',#41661,#31575,#31576);
#28036=AXIS2_PLACEMENT_3D('',#41663,#31578,#31579);
#28037=AXIS2_PLACEMENT_3D('',#41667,#31581,#31582);
#28038=AXIS2_PLACEMENT_3D('',#41669,#31583,#31584);
#28039=AXIS2_PLACEMENT_3D('',#41695,#31586,#31587);
#28040=AXIS2_PLACEMENT_3D('',#41698,#31589,#31590);
#28041=AXIS2_PLACEMENT_3D('',#41703,#31591,#31592);
#28042=AXIS2_PLACEMENT_3D('',#41705,#31593,#31594);
#28043=AXIS2_PLACEMENT_3D('',#41707,#31596,#31597);
#28044=AXIS2_PLACEMENT_3D('',#41711,#31599,#31600);
#28045=AXIS2_PLACEMENT_3D('',#41742,#31602,#31603);
#28046=AXIS2_PLACEMENT_3D('',#41744,#31604,#31605);
#28047=AXIS2_PLACEMENT_3D('',#41746,#31607,#31608);
#28048=AXIS2_PLACEMENT_3D('',#41750,#31610,#31611);
#28049=AXIS2_PLACEMENT_3D('',#41752,#31612,#31613);
#28050=AXIS2_PLACEMENT_3D('',#41774,#31615,#31616);
#28051=AXIS2_PLACEMENT_3D('',#41776,#31617,#31618);
#28052=AXIS2_PLACEMENT_3D('',#41778,#31620,#31621);
#28053=AXIS2_PLACEMENT_3D('',#41780,#31622,#31623);
#28054=AXIS2_PLACEMENT_3D('',#41782,#31625,#31626);
#28055=AXIS2_PLACEMENT_3D('',#41810,#31631,#31632);
#28056=AXIS2_PLACEMENT_3D('',#41812,#31633,#31634);
#28057=AXIS2_PLACEMENT_3D('',#41817,#31636,#31637);
#28058=AXIS2_PLACEMENT_3D('',#41821,#31639,#31640);
#28059=AXIS2_PLACEMENT_3D('',#41825,#31642,#31643);
#28060=AXIS2_PLACEMENT_3D('',#41828,#31645,#31646);
#28061=AXIS2_PLACEMENT_3D('',#41830,#31647,#31648);
#28062=AXIS2_PLACEMENT_3D('',#41831,#31649,#31650);
#28063=AXIS2_PLACEMENT_3D('',#41833,#31652,#31653);
#28064=AXIS2_PLACEMENT_3D('',#41835,#31655,#31656);
#28065=AXIS2_PLACEMENT_3D('',#41837,#31658,#31659);
#28066=AXIS2_PLACEMENT_3D('',#41839,#31660,#31661);
#28067=AXIS2_PLACEMENT_3D('',#41842,#31663,#31664);
#28068=AXIS2_PLACEMENT_3D('',#41843,#31665,#31666);
#28069=AXIS2_PLACEMENT_3D('',#41845,#31667,#31668);
#28070=AXIS2_PLACEMENT_3D('',#41847,#31669,#31670);
#28071=AXIS2_PLACEMENT_3D('',#41849,#31671,#31672);
#28072=AXIS2_PLACEMENT_3D('',#41851,#31673,#31674);
#28073=AXIS2_PLACEMENT_3D('',#41853,#31675,#31676);
#28074=AXIS2_PLACEMENT_3D('',#41854,#31677,#31678);
#28075=AXIS2_PLACEMENT_3D('',#41856,#31679,#31680);
#28076=AXIS2_PLACEMENT_3D('',#41858,#31682,#31683);
#28077=AXIS2_PLACEMENT_3D('',#41861,#31685,#31686);
#28078=AXIS2_PLACEMENT_3D('',#41862,#31687,#31688);
#28079=AXIS2_PLACEMENT_3D('',#41864,#31689,#31690);
#28080=AXIS2_PLACEMENT_3D('',#41866,#31692,#31693);
#28081=AXIS2_PLACEMENT_3D('',#41869,#31695,#31696);
#28082=AXIS2_PLACEMENT_3D('',#41870,#31697,#31698);
#28083=AXIS2_PLACEMENT_3D('',#41872,#31699,#31700);
#28084=AXIS2_PLACEMENT_3D('',#41874,#31702,#31703);
#28085=AXIS2_PLACEMENT_3D('',#41877,#31705,#31706);
#28086=AXIS2_PLACEMENT_3D('',#41878,#31707,#31708);
#28087=AXIS2_PLACEMENT_3D('',#41880,#31709,#31710);
#28088=AXIS2_PLACEMENT_3D('',#41882,#31712,#31713);
#28089=AXIS2_PLACEMENT_3D('',#41884,#31714,#31715);
#28090=AXIS2_PLACEMENT_3D('',#41886,#31717,#31718);
#28091=AXIS2_PLACEMENT_3D('',#41891,#31720,#31721);
#28092=AXIS2_PLACEMENT_3D('',#41895,#31723,#31724);
#28093=AXIS2_PLACEMENT_3D('',#41899,#31726,#31727);
#28094=AXIS2_PLACEMENT_3D('',#41902,#31729,#31730);
#28095=AXIS2_PLACEMENT_3D('',#41904,#31731,#31732);
#28096=AXIS2_PLACEMENT_3D('',#41905,#31733,#31734);
#28097=AXIS2_PLACEMENT_3D('',#41907,#31736,#31737);
#28098=AXIS2_PLACEMENT_3D('',#41909,#31738,#31739);
#28099=AXIS2_PLACEMENT_3D('',#41911,#31740,#31741);
#28100=AXIS2_PLACEMENT_3D('',#41912,#31742,#31743);
#28101=AXIS2_PLACEMENT_3D('',#41913,#31744,#31745);
#28102=AXIS2_PLACEMENT_3D('',#41916,#31747,#31748);
#28103=AXIS2_PLACEMENT_3D('',#41917,#31749,#31750);
#28104=AXIS2_PLACEMENT_3D('',#41919,#31751,#31752);
#28105=AXIS2_PLACEMENT_3D('',#41921,#31753,#31754);
#28106=AXIS2_PLACEMENT_3D('',#41923,#31755,#31756);
#28107=AXIS2_PLACEMENT_3D('',#41925,#31757,#31758);
#28108=AXIS2_PLACEMENT_3D('',#41927,#31759,#31760);
#28109=AXIS2_PLACEMENT_3D('',#41928,#31761,#31762);
#28110=AXIS2_PLACEMENT_3D('',#41930,#31763,#31764);
#28111=AXIS2_PLACEMENT_3D('',#41931,#31765,#31766);
#28112=AXIS2_PLACEMENT_3D('',#41932,#31767,#31768);
#28113=AXIS2_PLACEMENT_3D('',#41934,#31769,#31770);
#28114=AXIS2_PLACEMENT_3D('',#41936,#31771,#31772);
#28115=AXIS2_PLACEMENT_3D('',#41938,#31773,#31774);
#28116=AXIS2_PLACEMENT_3D('',#41940,#31775,#31776);
#28117=AXIS2_PLACEMENT_3D('',#41942,#31777,#31778);
#28118=AXIS2_PLACEMENT_3D('',#41943,#31779,#31780);
#28119=AXIS2_PLACEMENT_3D('',#41945,#31781,#31782);
#28120=AXIS2_PLACEMENT_3D('',#41947,#31783,#31784);
#28121=AXIS2_PLACEMENT_3D('',#41948,#31785,#31786);
#28122=AXIS2_PLACEMENT_3D('',#41949,#31787,#31788);
#28123=AXIS2_PLACEMENT_3D('',#41952,#31790,#31791);
#28124=AXIS2_PLACEMENT_3D('',#41953,#31792,#31793);
#28125=AXIS2_PLACEMENT_3D('',#41954,#31794,#31795);
#28126=AXIS2_PLACEMENT_3D('',#41956,#31797,#31798);
#28127=AXIS2_PLACEMENT_3D('',#41958,#31799,#31800);
#28128=AXIS2_PLACEMENT_3D('',#41959,#31801,#31802);
#28129=AXIS2_PLACEMENT_3D('',#41960,#31803,#31804);
#28130=AXIS2_PLACEMENT_3D('',#41964,#31806,#31807);
#28131=AXIS2_PLACEMENT_3D('',#41998,#31808,#31809);
#28132=AXIS2_PLACEMENT_3D('',#42015,#31810,#31811);
#28133=AXIS2_PLACEMENT_3D('',#42036,#31812,#31813);
#28134=AXIS2_PLACEMENT_3D('',#42075,#31814,#31815);
#28135=AXIS2_PLACEMENT_3D('',#42076,#31816,#31817);
#28136=AXIS2_PLACEMENT_3D('',#42083,#31818,#31819);
#28137=AXIS2_PLACEMENT_3D('',#42088,#31820,#31821);
#28138=AXIS2_PLACEMENT_3D('',#42090,#31823,#31824);
#28139=AXIS2_PLACEMENT_3D('',#42097,#31825,#31826);
#28140=AXIS2_PLACEMENT_3D('',#42102,#31827,#31828);
#28141=AXIS2_PLACEMENT_3D('',#42104,#31830,#31831);
#28142=AXIS2_PLACEMENT_3D('',#42105,#31832,#31833);
#28143=AXIS2_PLACEMENT_3D('',#42106,#31834,#31835);
#28144=AXIS2_PLACEMENT_3D('',#42107,#31836,#31837);
#28145=AXIS2_PLACEMENT_3D('',#42109,#31838,#31839);
#28146=AXIS2_PLACEMENT_3D('',#42111,#31840,#31841);
#28147=AXIS2_PLACEMENT_3D('',#42123,#31843,#31844);
#28148=AXIS2_PLACEMENT_3D('',#42124,#31845,#31846);
#28149=AXIS2_PLACEMENT_3D('',#42125,#31847,#31848);
#28150=AXIS2_PLACEMENT_3D('',#42127,#31849,#31850);
#28151=AXIS2_PLACEMENT_3D('',#42139,#31852,#31853);
#28152=AXIS2_PLACEMENT_3D('',#42140,#31854,#31855);
#28153=AXIS2_PLACEMENT_3D('',#42141,#31856,#31857);
#28154=AXIS2_PLACEMENT_3D('',#42143,#31858,#31859);
#28155=AXIS2_PLACEMENT_3D('',#42155,#31861,#31862);
#28156=AXIS2_PLACEMENT_3D('',#42156,#31863,#31864);
#28157=AXIS2_PLACEMENT_3D('',#42157,#31865,#31866);
#28158=AXIS2_PLACEMENT_3D('',#42159,#31867,#31868);
#28159=AXIS2_PLACEMENT_3D('',#42170,#31870,#31871);
#28160=AXIS2_PLACEMENT_3D('',#42171,#31872,#31873);
#28161=AXIS2_PLACEMENT_3D('',#42174,#31876,#31877);
#28162=AXIS2_PLACEMENT_3D('',#42176,#31879,#31880);
#28163=AXIS2_PLACEMENT_3D('',#42178,#31882,#31883);
#28164=AXIS2_PLACEMENT_3D('',#42180,#31885,#31886);
#28165=AXIS2_PLACEMENT_3D('',#42182,#31887,#31888);
#28166=AXIS2_PLACEMENT_3D('',#42183,#31889,#31890);
#28167=AXIS2_PLACEMENT_3D('',#42184,#31891,#31892);
#28168=AXIS2_PLACEMENT_3D('',#42187,#31895,#31896);
#28169=AXIS2_PLACEMENT_3D('',#42189,#31897,#31898);
#28170=AXIS2_PLACEMENT_3D('',#42191,#31899,#31900);
#28171=AXIS2_PLACEMENT_3D('',#42192,#31901,#31902);
#28172=AXIS2_PLACEMENT_3D('',#42194,#31903,#31904);
#28173=AXIS2_PLACEMENT_3D('',#42196,#31905,#31906);
#28174=AXIS2_PLACEMENT_3D('',#42197,#31907,#31908);
#28175=AXIS2_PLACEMENT_3D('',#42198,#31909,#31910);
#28176=AXIS2_PLACEMENT_3D('',#42202,#31912,#31913);
#28177=AXIS2_PLACEMENT_3D('',#42204,#31915,#31916);
#28178=AXIS2_PLACEMENT_3D('',#42208,#31918,#31919);
#28179=AXIS2_PLACEMENT_3D('',#42210,#31921,#31922);
#28180=AXIS2_PLACEMENT_3D('',#42212,#31924,#31925);
#28181=AXIS2_PLACEMENT_3D('',#42215,#31927,#31928);
#28182=AXIS2_PLACEMENT_3D('',#42216,#31929,#31930);
#28183=AXIS2_PLACEMENT_3D('',#42218,#31931,#31932);
#28184=AXIS2_PLACEMENT_3D('',#42220,#31934,#31935);
#28185=AXIS2_PLACEMENT_3D('',#42222,#31936,#31937);
#28186=AXIS2_PLACEMENT_3D('',#42224,#31938,#31939);
#28187=AXIS2_PLACEMENT_3D('',#42225,#31940,#31941);
#28188=AXIS2_PLACEMENT_3D('',#42226,#31942,#31943);
#28189=AXIS2_PLACEMENT_3D('',#42228,#31944,#31945);
#28190=AXIS2_PLACEMENT_3D('',#42230,#31947,#31948);
#28191=AXIS2_PLACEMENT_3D('',#42232,#31949,#31950);
#28192=AXIS2_PLACEMENT_3D('',#42233,#31951,#31952);
#28193=AXIS2_PLACEMENT_3D('',#42234,#31953,#31954);
#28194=AXIS2_PLACEMENT_3D('',#42235,#31955,#31956);
#28195=AXIS2_PLACEMENT_3D('',#42238,#31957,#31958);
#28196=AXIS2_PLACEMENT_3D('',#42242,#31960,#31961);
#28197=AXIS2_PLACEMENT_3D('',#42244,#31963,#31964);
#28198=AXIS2_PLACEMENT_3D('',#42247,#31965,#31966);
#28199=AXIS2_PLACEMENT_3D('',#42248,#31967,#31968);
#28200=AXIS2_PLACEMENT_3D('',#42249,#31969,#31970);
#28201=AXIS2_PLACEMENT_3D('',#42250,#31971,#31972);
#28202=AXIS2_PLACEMENT_3D('',#42253,#31973,#31974);
#28203=AXIS2_PLACEMENT_3D('',#42256,#31977,#31978);
#28204=AXIS2_PLACEMENT_3D('',#42259,#31979,#31980);
#28205=AXIS2_PLACEMENT_3D('',#42260,#31981,#31982);
#28206=AXIS2_PLACEMENT_3D('',#42261,#31983,#31984);
#28207=AXIS2_PLACEMENT_3D('',#42262,#31985,#31986);
#28208=AXIS2_PLACEMENT_3D('',#42265,#31987,#31988);
#28209=AXIS2_PLACEMENT_3D('',#42268,#31991,#31992);
#28210=AXIS2_PLACEMENT_3D('',#42271,#31993,#31994);
#28211=AXIS2_PLACEMENT_3D('',#42272,#31995,#31996);
#28212=AXIS2_PLACEMENT_3D('',#42273,#31997,#31998);
#28213=AXIS2_PLACEMENT_3D('',#42274,#31999,#32000);
#28214=AXIS2_PLACEMENT_3D('',#42277,#32001,#32002);
#28215=AXIS2_PLACEMENT_3D('',#42280,#32005,#32006);
#28216=AXIS2_PLACEMENT_3D('',#42281,#32007,#32008);
#28217=AXIS2_PLACEMENT_3D('',#42282,#32009,#32010);
#28218=AXIS2_PLACEMENT_3D('',#42283,#32011,#32012);
#28219=AXIS2_PLACEMENT_3D('',#42287,#32014,#32015);
#28220=AXIS2_PLACEMENT_3D('',#42289,#32017,#32018);
#28221=AXIS2_PLACEMENT_3D('',#42293,#32021,#32022);
#28222=AXIS2_PLACEMENT_3D('',#42296,#32024,#32025);
#28223=AXIS2_PLACEMENT_3D('',#42297,#32026,#32027);
#28224=AXIS2_PLACEMENT_3D('',#42301,#32030,#32031);
#28225=AXIS2_PLACEMENT_3D('',#42307,#32035,#32036);
#28226=AXIS2_PLACEMENT_3D('',#42309,#32037,#32038);
#28227=AXIS2_PLACEMENT_3D('',#42311,#32039,#32040);
#28228=AXIS2_PLACEMENT_3D('',#42313,#32042,#32043);
#28229=AXIS2_PLACEMENT_3D('',#42316,#32044,#32045);
#28230=AXIS2_PLACEMENT_3D('',#42317,#32046,#32047);
#28231=AXIS2_PLACEMENT_3D('',#42318,#32048,#32049);
#28232=AXIS2_PLACEMENT_3D('',#42319,#32050,#32051);
#28233=AXIS2_PLACEMENT_3D('',#42322,#32052,#32053);
#28234=AXIS2_PLACEMENT_3D('',#42325,#32056,#32057);
#28235=AXIS2_PLACEMENT_3D('',#42328,#32058,#32059);
#28236=AXIS2_PLACEMENT_3D('',#42329,#32060,#32061);
#28237=AXIS2_PLACEMENT_3D('',#42330,#32062,#32063);
#28238=AXIS2_PLACEMENT_3D('',#42331,#32064,#32065);
#28239=AXIS2_PLACEMENT_3D('',#42333,#32066,#32067);
#28240=AXIS2_PLACEMENT_3D('',#42336,#32070,#32071);
#28241=AXIS2_PLACEMENT_3D('',#42338,#32072,#32073);
#28242=AXIS2_PLACEMENT_3D('',#42339,#32074,#32075);
#28243=AXIS2_PLACEMENT_3D('',#42340,#32076,#32077);
#28244=AXIS2_PLACEMENT_3D('',#42342,#32078,#32079);
#28245=AXIS2_PLACEMENT_3D('',#42344,#32081,#32082);
#28246=AXIS2_PLACEMENT_3D('',#42345,#32083,#32084);
#28247=AXIS2_PLACEMENT_3D('',#42346,#32085,#32086);
#28248=AXIS2_PLACEMENT_3D('',#42349,#32089,#32090);
#28249=AXIS2_PLACEMENT_3D('',#42351,#32092,#32093);
#28250=AXIS2_PLACEMENT_3D('',#42352,#32094,#32095);
#28251=AXIS2_PLACEMENT_3D('',#42355,#32098,#32099);
#28252=AXIS2_PLACEMENT_3D('',#42357,#32100,#32101);
#28253=AXIS2_PLACEMENT_3D('',#42359,#32102,#32103);
#28254=AXIS2_PLACEMENT_3D('',#42361,#32105,#32106);
#28255=AXIS2_PLACEMENT_3D('',#42364,#32107,#32108);
#28256=AXIS2_PLACEMENT_3D('',#42365,#32109,#32110);
#28257=AXIS2_PLACEMENT_3D('',#42366,#32111,#32112);
#28258=AXIS2_PLACEMENT_3D('',#42367,#32113,#32114);
#28259=AXIS2_PLACEMENT_3D('',#42370,#32115,#32116);
#28260=AXIS2_PLACEMENT_3D('',#42373,#32119,#32120);
#28261=AXIS2_PLACEMENT_3D('',#42375,#32121,#32122);
#28262=AXIS2_PLACEMENT_3D('',#42376,#32123,#32124);
#28263=AXIS2_PLACEMENT_3D('',#42377,#32125,#32126);
#28264=AXIS2_PLACEMENT_3D('',#42378,#32127,#32128);
#28265=AXIS2_PLACEMENT_3D('',#42380,#32129,#32130);
#28266=AXIS2_PLACEMENT_3D('',#42382,#32132,#32133);
#28267=AXIS2_PLACEMENT_3D('',#42385,#32134,#32135);
#28268=AXIS2_PLACEMENT_3D('',#42386,#32136,#32137);
#28269=AXIS2_PLACEMENT_3D('',#42387,#32138,#32139);
#28270=AXIS2_PLACEMENT_3D('',#42388,#32140,#32141);
#28271=AXIS2_PLACEMENT_3D('',#42391,#32142,#32143);
#28272=AXIS2_PLACEMENT_3D('',#42394,#32146,#32147);
#28273=AXIS2_PLACEMENT_3D('',#42395,#32148,#32149);
#28274=AXIS2_PLACEMENT_3D('',#42396,#32150,#32151);
#28275=AXIS2_PLACEMENT_3D('',#42397,#32152,#32153);
#28276=AXIS2_PLACEMENT_3D('',#42399,#32155,#32156);
#28277=AXIS2_PLACEMENT_3D('',#42402,#32158,#32159);
#28278=AXIS2_PLACEMENT_3D('',#42406,#32161,#32162);
#28279=AXIS2_PLACEMENT_3D('',#42410,#32164,#32165);
#28280=AXIS2_PLACEMENT_3D('',#42413,#32167,#32168);
#28281=AXIS2_PLACEMENT_3D('',#42414,#32169,#32170);
#28282=AXIS2_PLACEMENT_3D('',#42415,#32171,#32172);
#28283=AXIS2_PLACEMENT_3D('',#42417,#32173,#32174);
#28284=AXIS2_PLACEMENT_3D('',#42418,#32175,#32176);
#28285=AXIS2_PLACEMENT_3D('',#42420,#32177,#32178);
#28286=AXIS2_PLACEMENT_3D('',#42423,#32180,#32181);
#28287=AXIS2_PLACEMENT_3D('',#42424,#32182,#32183);
#28288=AXIS2_PLACEMENT_3D('',#42426,#32184,#32185);
#28289=AXIS2_PLACEMENT_3D('',#42427,#32186,#32187);
#28290=AXIS2_PLACEMENT_3D('',#42428,#32188,#32189);
#28291=AXIS2_PLACEMENT_3D('',#42430,#32190,#32191);
#28292=AXIS2_PLACEMENT_3D('',#42432,#32193,#32194);
#28293=AXIS2_PLACEMENT_3D('',#42434,#32195,#32196);
#28294=AXIS2_PLACEMENT_3D('',#42435,#32197,#32198);
#28295=AXIS2_PLACEMENT_3D('',#42436,#32199,#32200);
#28296=AXIS2_PLACEMENT_3D('',#42438,#32201,#32202);
#28297=AXIS2_PLACEMENT_3D('',#42440,#32204,#32205);
#28298=AXIS2_PLACEMENT_3D('',#42442,#32206,#32207);
#28299=AXIS2_PLACEMENT_3D('',#42443,#32208,#32209);
#28300=AXIS2_PLACEMENT_3D('',#42444,#32210,#32211);
#28301=AXIS2_PLACEMENT_3D('',#42446,#32212,#32213);
#28302=AXIS2_PLACEMENT_3D('',#42448,#32215,#32216);
#28303=AXIS2_PLACEMENT_3D('',#42449,#32217,#32218);
#28304=AXIS2_PLACEMENT_3D('',#42450,#32219,#32220);
#28305=AXIS2_PLACEMENT_3D('',#42454,#32222,#32223);
#28306=AXIS2_PLACEMENT_3D('',#42456,#32225,#32226);
#28307=AXIS2_PLACEMENT_3D('',#42460,#32229,#32230);
#28308=AXIS2_PLACEMENT_3D('',#42463,#32232,#32233);
#28309=AXIS2_PLACEMENT_3D('',#42464,#32234,#32235);
#28310=AXIS2_PLACEMENT_3D('',#42468,#32238,#32239);
#28311=AXIS2_PLACEMENT_3D('',#42469,#32240,#32241);
#28312=AXIS2_PLACEMENT_3D('',#42470,#32242,#32243);
#28313=AXIS2_PLACEMENT_3D('',#42471,#32244,#32245);
#28314=AXIS2_PLACEMENT_3D('',#42473,#32246,#32247);
#28315=AXIS2_PLACEMENT_3D('',#42474,#32248,#32249);
#28316=AXIS2_PLACEMENT_3D('',#42475,#32250,#32251);
#28317=AXIS2_PLACEMENT_3D('',#42477,#32252,#32253);
#28318=AXIS2_PLACEMENT_3D('',#42479,#32255,#32256);
#28319=AXIS2_PLACEMENT_3D('',#42481,#32257,#32258);
#28320=AXIS2_PLACEMENT_3D('',#42482,#32259,#32260);
#28321=AXIS2_PLACEMENT_3D('',#42483,#32261,#32262);
#28322=AXIS2_PLACEMENT_3D('',#42484,#32263,#32264);
#28323=AXIS2_PLACEMENT_3D('',#42486,#32266,#32267);
#28324=AXIS2_PLACEMENT_3D('',#42487,#32268,#32269);
#28325=AXIS2_PLACEMENT_3D('',#42488,#32270,#32271);
#28326=AXIS2_PLACEMENT_3D('',#42489,#32272,#32273);
#28327=AXIS2_PLACEMENT_3D('',#42490,#32274,#32275);
#28328=AXIS2_PLACEMENT_3D('',#42491,#32276,#32277);
#28329=AXIS2_PLACEMENT_3D('',#42494,#32280,#32281);
#28330=AXIS2_PLACEMENT_3D('',#42496,#32283,#32284);
#28331=AXIS2_PLACEMENT_3D('',#42497,#32285,#32286);
#28332=AXIS2_PLACEMENT_3D('',#42498,#32287,#32288);
#28333=AXIS2_PLACEMENT_3D('',#42499,#32289,#32290);
#28334=AXIS2_PLACEMENT_3D('',#42500,#32291,#32292);
#28335=AXIS2_PLACEMENT_3D('',#42501,#32293,#32294);
#28336=AXIS2_PLACEMENT_3D('',#42503,#32296,#32297);
#28337=AXIS2_PLACEMENT_3D('',#42505,#32299,#32300);
#28338=AXIS2_PLACEMENT_3D('',#42507,#32302,#32303);
#28339=AXIS2_PLACEMENT_3D('',#42509,#32305,#32306);
#28340=AXIS2_PLACEMENT_3D('',#42510,#32307,#32308);
#28341=AXIS2_PLACEMENT_3D('',#42511,#32309,#32310);
#28342=AXIS2_PLACEMENT_3D('',#42513,#32311,#32312);
#28343=AXIS2_PLACEMENT_3D('',#42515,#32313,#32314);
#28344=AXIS2_PLACEMENT_3D('',#42516,#32315,#32316);
#28345=AXIS2_PLACEMENT_3D('',#42518,#32318,#32319);
#28346=AXIS2_PLACEMENT_3D('',#42520,#32320,#32321);
#28347=AXIS2_PLACEMENT_3D('',#42522,#32322,#32323);
#28348=AXIS2_PLACEMENT_3D('',#42523,#32324,#32325);
#28349=AXIS2_PLACEMENT_3D('',#42525,#32327,#32328);
#28350=AXIS2_PLACEMENT_3D('',#42527,#32330,#32331);
#28351=AXIS2_PLACEMENT_3D('',#42529,#32333,#32334);
#28352=AXIS2_PLACEMENT_3D('',#42530,#32335,#32336);
#28353=AXIS2_PLACEMENT_3D('',#42532,#32338,#32339);
#28354=AXIS2_PLACEMENT_3D('',#42533,#32340,#32341);
#28355=AXIS2_PLACEMENT_3D('',#42535,#32343,#32344);
#28356=AXIS2_PLACEMENT_3D('',#42537,#32346,#32347);
#28357=AXIS2_PLACEMENT_3D('',#42539,#32349,#32350);
#28358=AXIS2_PLACEMENT_3D('',#42540,#32351,#32352);
#28359=AXIS2_PLACEMENT_3D('',#42543,#32355,#32356);
#28360=AXIS2_PLACEMENT_3D('',#42545,#32358,#32359);
#28361=AXIS2_PLACEMENT_3D('',#42547,#32361,#32362);
#28362=AXIS2_PLACEMENT_3D('',#42549,#32364,#32365);
#28363=AXIS2_PLACEMENT_3D('',#42551,#32367,#32368);
#28364=AXIS2_PLACEMENT_3D('',#42553,#32370,#32371);
#28365=AXIS2_PLACEMENT_3D('',#42555,#32373,#32374);
#28366=AXIS2_PLACEMENT_3D('',#42556,#32375,#32376);
#28367=AXIS2_PLACEMENT_3D('',#42559,#32379,#32380);
#28368=AXIS2_PLACEMENT_3D('',#42560,#32381,#32382);
#28369=AXIS2_PLACEMENT_3D('',#42561,#32383,#32384);
#28370=AXIS2_PLACEMENT_3D('',#42563,#32386,#32387);
#28371=AXIS2_PLACEMENT_3D('',#42565,#32389,#32390);
#28372=AXIS2_PLACEMENT_3D('',#42566,#32391,#32392);
#28373=AXIS2_PLACEMENT_3D('',#42569,#32393,#32394);
#28374=AXIS2_PLACEMENT_3D('',#42575,#32398,#32399);
#28375=AXIS2_PLACEMENT_3D('',#42581,#32403,#32404);
#28376=AXIS2_PLACEMENT_3D('',#42583,#32405,#32406);
#28377=AXIS2_PLACEMENT_3D('',#42585,#32407,#32408);
#28378=AXIS2_PLACEMENT_3D('',#42589,#32410,#32411);
#28379=AXIS2_PLACEMENT_3D('',#42593,#32413,#32414);
#28380=AXIS2_PLACEMENT_3D('',#42595,#32415,#32416);
#28381=AXIS2_PLACEMENT_3D('',#42597,#32417,#32418);
#28382=AXIS2_PLACEMENT_3D('',#42601,#32420,#32421);
#28383=AXIS2_PLACEMENT_3D('',#42605,#32423,#32424);
#28384=AXIS2_PLACEMENT_3D('',#42607,#32425,#32426);
#28385=AXIS2_PLACEMENT_3D('',#42611,#32428,#32429);
#28386=AXIS2_PLACEMENT_3D('',#42613,#32430,#32431);
#28387=AXIS2_PLACEMENT_3D('',#42617,#32433,#32434);
#28388=AXIS2_PLACEMENT_3D('',#42621,#32436,#32437);
#28389=AXIS2_PLACEMENT_3D('',#42623,#32438,#32439);
#28390=AXIS2_PLACEMENT_3D('',#42625,#32440,#32441);
#28391=AXIS2_PLACEMENT_3D('',#42629,#32443,#32444);
#28392=AXIS2_PLACEMENT_3D('',#42633,#32446,#32447);
#28393=AXIS2_PLACEMENT_3D('',#42635,#32448,#32449);
#28394=AXIS2_PLACEMENT_3D('',#42637,#32450,#32451);
#28395=AXIS2_PLACEMENT_3D('',#42641,#32453,#32454);
#28396=AXIS2_PLACEMENT_3D('',#42645,#32456,#32457);
#28397=AXIS2_PLACEMENT_3D('',#42647,#32458,#32459);
#28398=AXIS2_PLACEMENT_3D('',#42649,#32460,#32461);
#28399=AXIS2_PLACEMENT_3D('',#42653,#32463,#32464);
#28400=AXIS2_PLACEMENT_3D('',#42657,#32466,#32467);
#28401=AXIS2_PLACEMENT_3D('',#42659,#32468,#32469);
#28402=AXIS2_PLACEMENT_3D('',#42661,#32470,#32471);
#28403=AXIS2_PLACEMENT_3D('',#42665,#32473,#32474);
#28404=AXIS2_PLACEMENT_3D('',#42669,#32476,#32477);
#28405=AXIS2_PLACEMENT_3D('',#42671,#32478,#32479);
#28406=AXIS2_PLACEMENT_3D('',#42673,#32480,#32481);
#28407=AXIS2_PLACEMENT_3D('',#42677,#32483,#32484);
#28408=AXIS2_PLACEMENT_3D('',#42681,#32486,#32487);
#28409=AXIS2_PLACEMENT_3D('',#42683,#32488,#32489);
#28410=AXIS2_PLACEMENT_3D('',#42685,#32490,#32491);
#28411=AXIS2_PLACEMENT_3D('',#42689,#32493,#32494);
#28412=AXIS2_PLACEMENT_3D('',#42693,#32496,#32497);
#28413=AXIS2_PLACEMENT_3D('',#42695,#32498,#32499);
#28414=AXIS2_PLACEMENT_3D('',#42697,#32500,#32501);
#28415=AXIS2_PLACEMENT_3D('',#42701,#32503,#32504);
#28416=AXIS2_PLACEMENT_3D('',#42705,#32506,#32507);
#28417=AXIS2_PLACEMENT_3D('',#42707,#32508,#32509);
#28418=AXIS2_PLACEMENT_3D('',#42709,#32510,#32511);
#28419=AXIS2_PLACEMENT_3D('',#42713,#32513,#32514);
#28420=AXIS2_PLACEMENT_3D('',#42717,#32516,#32517);
#28421=AXIS2_PLACEMENT_3D('',#42719,#32518,#32519);
#28422=AXIS2_PLACEMENT_3D('',#42721,#32520,#32521);
#28423=AXIS2_PLACEMENT_3D('',#42725,#32523,#32524);
#28424=AXIS2_PLACEMENT_3D('',#42729,#32526,#32527);
#28425=AXIS2_PLACEMENT_3D('',#42731,#32528,#32529);
#28426=AXIS2_PLACEMENT_3D('',#42733,#32530,#32531);
#28427=AXIS2_PLACEMENT_3D('',#42737,#32533,#32534);
#28428=AXIS2_PLACEMENT_3D('',#42741,#32536,#32537);
#28429=AXIS2_PLACEMENT_3D('',#42743,#32538,#32539);
#28430=AXIS2_PLACEMENT_3D('',#42745,#32540,#32541);
#28431=AXIS2_PLACEMENT_3D('',#42749,#32543,#32544);
#28432=AXIS2_PLACEMENT_3D('',#42753,#32546,#32547);
#28433=AXIS2_PLACEMENT_3D('',#42755,#32548,#32549);
#28434=AXIS2_PLACEMENT_3D('',#42757,#32550,#32551);
#28435=AXIS2_PLACEMENT_3D('',#42761,#32553,#32554);
#28436=AXIS2_PLACEMENT_3D('',#42765,#32556,#32557);
#28437=AXIS2_PLACEMENT_3D('',#42767,#32558,#32559);
#28438=AXIS2_PLACEMENT_3D('',#42769,#32560,#32561);
#28439=AXIS2_PLACEMENT_3D('',#42773,#32563,#32564);
#28440=AXIS2_PLACEMENT_3D('',#42777,#32566,#32567);
#28441=AXIS2_PLACEMENT_3D('',#42779,#32568,#32569);
#28442=AXIS2_PLACEMENT_3D('',#42781,#32570,#32571);
#28443=AXIS2_PLACEMENT_3D('',#42785,#32573,#32574);
#28444=AXIS2_PLACEMENT_3D('',#42789,#32576,#32577);
#28445=AXIS2_PLACEMENT_3D('',#42791,#32578,#32579);
#28446=AXIS2_PLACEMENT_3D('',#42793,#32580,#32581);
#28447=AXIS2_PLACEMENT_3D('',#42797,#32583,#32584);
#28448=AXIS2_PLACEMENT_3D('',#42801,#32586,#32587);
#28449=AXIS2_PLACEMENT_3D('',#42803,#32588,#32589);
#28450=AXIS2_PLACEMENT_3D('',#42805,#32590,#32591);
#28451=AXIS2_PLACEMENT_3D('',#42809,#32593,#32594);
#28452=AXIS2_PLACEMENT_3D('',#42813,#32596,#32597);
#28453=AXIS2_PLACEMENT_3D('',#42815,#32598,#32599);
#28454=AXIS2_PLACEMENT_3D('',#42817,#32600,#32601);
#28455=AXIS2_PLACEMENT_3D('',#42821,#32603,#32604);
#28456=AXIS2_PLACEMENT_3D('',#42825,#32606,#32607);
#28457=AXIS2_PLACEMENT_3D('',#42827,#32608,#32609);
#28458=AXIS2_PLACEMENT_3D('',#42829,#32610,#32611);
#28459=AXIS2_PLACEMENT_3D('',#42833,#32613,#32614);
#28460=AXIS2_PLACEMENT_3D('',#42837,#32616,#32617);
#28461=AXIS2_PLACEMENT_3D('',#42839,#32618,#32619);
#28462=AXIS2_PLACEMENT_3D('',#42841,#32620,#32621);
#28463=AXIS2_PLACEMENT_3D('',#42845,#32623,#32624);
#28464=AXIS2_PLACEMENT_3D('',#42849,#32626,#32627);
#28465=AXIS2_PLACEMENT_3D('',#42851,#32628,#32629);
#28466=AXIS2_PLACEMENT_3D('',#42853,#32630,#32631);
#28467=AXIS2_PLACEMENT_3D('',#42857,#32633,#32634);
#28468=AXIS2_PLACEMENT_3D('',#42861,#32636,#32637);
#28469=AXIS2_PLACEMENT_3D('',#42863,#32638,#32639);
#28470=AXIS2_PLACEMENT_3D('',#42865,#32640,#32641);
#28471=AXIS2_PLACEMENT_3D('',#42869,#32643,#32644);
#28472=AXIS2_PLACEMENT_3D('',#42873,#32646,#32647);
#28473=AXIS2_PLACEMENT_3D('',#42875,#32648,#32649);
#28474=AXIS2_PLACEMENT_3D('',#42877,#32650,#32651);
#28475=AXIS2_PLACEMENT_3D('',#42881,#32653,#32654);
#28476=AXIS2_PLACEMENT_3D('',#42885,#32656,#32657);
#28477=AXIS2_PLACEMENT_3D('',#42887,#32658,#32659);
#28478=AXIS2_PLACEMENT_3D('',#42889,#32660,#32661);
#28479=AXIS2_PLACEMENT_3D('',#42893,#32663,#32664);
#28480=AXIS2_PLACEMENT_3D('',#42897,#32666,#32667);
#28481=AXIS2_PLACEMENT_3D('',#42899,#32668,#32669);
#28482=AXIS2_PLACEMENT_3D('',#42901,#32670,#32671);
#28483=AXIS2_PLACEMENT_3D('',#42905,#32673,#32674);
#28484=AXIS2_PLACEMENT_3D('',#42909,#32676,#32677);
#28485=AXIS2_PLACEMENT_3D('',#42911,#32678,#32679);
#28486=AXIS2_PLACEMENT_3D('',#42913,#32680,#32681);
#28487=AXIS2_PLACEMENT_3D('',#42917,#32683,#32684);
#28488=AXIS2_PLACEMENT_3D('',#42921,#32686,#32687);
#28489=AXIS2_PLACEMENT_3D('',#42923,#32688,#32689);
#28490=AXIS2_PLACEMENT_3D('',#42925,#32690,#32691);
#28491=AXIS2_PLACEMENT_3D('',#42929,#32693,#32694);
#28492=AXIS2_PLACEMENT_3D('',#42933,#32696,#32697);
#28493=AXIS2_PLACEMENT_3D('',#42935,#32698,#32699);
#28494=AXIS2_PLACEMENT_3D('',#42937,#32700,#32701);
#28495=AXIS2_PLACEMENT_3D('',#42941,#32703,#32704);
#28496=AXIS2_PLACEMENT_3D('',#42945,#32706,#32707);
#28497=AXIS2_PLACEMENT_3D('',#42947,#32708,#32709);
#28498=AXIS2_PLACEMENT_3D('',#42949,#32710,#32711);
#28499=AXIS2_PLACEMENT_3D('',#42953,#32713,#32714);
#28500=AXIS2_PLACEMENT_3D('',#42957,#32716,#32717);
#28501=AXIS2_PLACEMENT_3D('',#42959,#32718,#32719);
#28502=AXIS2_PLACEMENT_3D('',#42961,#32720,#32721);
#28503=AXIS2_PLACEMENT_3D('',#42965,#32723,#32724);
#28504=AXIS2_PLACEMENT_3D('',#42969,#32726,#32727);
#28505=AXIS2_PLACEMENT_3D('',#42970,#32728,#32729);
#28506=AXIS2_PLACEMENT_3D('',#42972,#32730,#32731);
#28507=AXIS2_PLACEMENT_3D('',#42974,#32732,#32733);
#28508=AXIS2_PLACEMENT_3D('',#42978,#32735,#32736);
#28509=AXIS2_PLACEMENT_3D('',#42982,#32738,#32739);
#28510=AXIS2_PLACEMENT_3D('',#42984,#32740,#32741);
#28511=AXIS2_PLACEMENT_3D('',#42986,#32742,#32743);
#28512=AXIS2_PLACEMENT_3D('',#42990,#32745,#32746);
#28513=AXIS2_PLACEMENT_3D('',#42994,#32748,#32749);
#28514=AXIS2_PLACEMENT_3D('',#42996,#32750,#32751);
#28515=AXIS2_PLACEMENT_3D('',#42998,#32752,#32753);
#28516=AXIS2_PLACEMENT_3D('',#43002,#32755,#32756);
#28517=AXIS2_PLACEMENT_3D('',#43006,#32758,#32759);
#28518=AXIS2_PLACEMENT_3D('',#43008,#32760,#32761);
#28519=AXIS2_PLACEMENT_3D('',#43010,#32762,#32763);
#28520=AXIS2_PLACEMENT_3D('',#43014,#32765,#32766);
#28521=AXIS2_PLACEMENT_3D('',#43018,#32768,#32769);
#28522=AXIS2_PLACEMENT_3D('',#43020,#32770,#32771);
#28523=AXIS2_PLACEMENT_3D('',#43022,#32772,#32773);
#28524=AXIS2_PLACEMENT_3D('',#43026,#32775,#32776);
#28525=AXIS2_PLACEMENT_3D('',#43030,#32778,#32779);
#28526=AXIS2_PLACEMENT_3D('',#43032,#32780,#32781);
#28527=AXIS2_PLACEMENT_3D('',#43034,#32782,#32783);
#28528=AXIS2_PLACEMENT_3D('',#43038,#32785,#32786);
#28529=AXIS2_PLACEMENT_3D('',#43042,#32788,#32789);
#28530=AXIS2_PLACEMENT_3D('',#43044,#32790,#32791);
#28531=AXIS2_PLACEMENT_3D('',#43046,#32792,#32793);
#28532=AXIS2_PLACEMENT_3D('',#43050,#32795,#32796);
#28533=AXIS2_PLACEMENT_3D('',#43054,#32798,#32799);
#28534=AXIS2_PLACEMENT_3D('',#43056,#32800,#32801);
#28535=AXIS2_PLACEMENT_3D('',#43058,#32802,#32803);
#28536=AXIS2_PLACEMENT_3D('',#43062,#32805,#32806);
#28537=AXIS2_PLACEMENT_3D('',#43066,#32808,#32809);
#28538=AXIS2_PLACEMENT_3D('',#43068,#32810,#32811);
#28539=AXIS2_PLACEMENT_3D('',#43070,#32812,#32813);
#28540=AXIS2_PLACEMENT_3D('',#43074,#32815,#32816);
#28541=AXIS2_PLACEMENT_3D('',#43078,#32818,#32819);
#28542=AXIS2_PLACEMENT_3D('',#43080,#32820,#32821);
#28543=AXIS2_PLACEMENT_3D('',#43082,#32822,#32823);
#28544=AXIS2_PLACEMENT_3D('',#43086,#32825,#32826);
#28545=AXIS2_PLACEMENT_3D('',#43090,#32828,#32829);
#28546=AXIS2_PLACEMENT_3D('',#43092,#32830,#32831);
#28547=AXIS2_PLACEMENT_3D('',#43094,#32832,#32833);
#28548=AXIS2_PLACEMENT_3D('',#43098,#32835,#32836);
#28549=AXIS2_PLACEMENT_3D('',#43102,#32838,#32839);
#28550=AXIS2_PLACEMENT_3D('',#43104,#32840,#32841);
#28551=AXIS2_PLACEMENT_3D('',#43106,#32842,#32843);
#28552=AXIS2_PLACEMENT_3D('',#43110,#32845,#32846);
#28553=AXIS2_PLACEMENT_3D('',#43114,#32848,#32849);
#28554=AXIS2_PLACEMENT_3D('',#43116,#32850,#32851);
#28555=AXIS2_PLACEMENT_3D('',#43118,#32852,#32853);
#28556=AXIS2_PLACEMENT_3D('',#43122,#32855,#32856);
#28557=AXIS2_PLACEMENT_3D('',#43126,#32858,#32859);
#28558=AXIS2_PLACEMENT_3D('',#43128,#32860,#32861);
#28559=AXIS2_PLACEMENT_3D('',#43130,#32862,#32863);
#28560=AXIS2_PLACEMENT_3D('',#43134,#32865,#32866);
#28561=AXIS2_PLACEMENT_3D('',#43138,#32868,#32869);
#28562=AXIS2_PLACEMENT_3D('',#43140,#32870,#32871);
#28563=AXIS2_PLACEMENT_3D('',#43142,#32872,#32873);
#28564=AXIS2_PLACEMENT_3D('',#43146,#32875,#32876);
#28565=AXIS2_PLACEMENT_3D('',#43150,#32878,#32879);
#28566=AXIS2_PLACEMENT_3D('',#43152,#32880,#32881);
#28567=AXIS2_PLACEMENT_3D('',#43154,#32882,#32883);
#28568=AXIS2_PLACEMENT_3D('',#43158,#32885,#32886);
#28569=AXIS2_PLACEMENT_3D('',#43162,#32888,#32889);
#28570=AXIS2_PLACEMENT_3D('',#43164,#32890,#32891);
#28571=AXIS2_PLACEMENT_3D('',#43166,#32892,#32893);
#28572=AXIS2_PLACEMENT_3D('',#43170,#32895,#32896);
#28573=AXIS2_PLACEMENT_3D('',#43174,#32898,#32899);
#28574=AXIS2_PLACEMENT_3D('',#43176,#32900,#32901);
#28575=AXIS2_PLACEMENT_3D('',#43178,#32902,#32903);
#28576=AXIS2_PLACEMENT_3D('',#43182,#32905,#32906);
#28577=AXIS2_PLACEMENT_3D('',#43186,#32908,#32909);
#28578=AXIS2_PLACEMENT_3D('',#43188,#32910,#32911);
#28579=AXIS2_PLACEMENT_3D('',#43190,#32912,#32913);
#28580=AXIS2_PLACEMENT_3D('',#43194,#32915,#32916);
#28581=AXIS2_PLACEMENT_3D('',#43198,#32918,#32919);
#28582=AXIS2_PLACEMENT_3D('',#43200,#32920,#32921);
#28583=AXIS2_PLACEMENT_3D('',#43202,#32922,#32923);
#28584=AXIS2_PLACEMENT_3D('',#43206,#32925,#32926);
#28585=AXIS2_PLACEMENT_3D('',#43210,#32928,#32929);
#28586=AXIS2_PLACEMENT_3D('',#43212,#32930,#32931);
#28587=AXIS2_PLACEMENT_3D('',#43214,#32932,#32933);
#28588=AXIS2_PLACEMENT_3D('',#43218,#32935,#32936);
#28589=AXIS2_PLACEMENT_3D('',#43222,#32938,#32939);
#28590=AXIS2_PLACEMENT_3D('',#43224,#32940,#32941);
#28591=AXIS2_PLACEMENT_3D('',#43226,#32942,#32943);
#28592=AXIS2_PLACEMENT_3D('',#43230,#32945,#32946);
#28593=AXIS2_PLACEMENT_3D('',#43234,#32948,#32949);
#28594=AXIS2_PLACEMENT_3D('',#43236,#32950,#32951);
#28595=AXIS2_PLACEMENT_3D('',#43238,#32952,#32953);
#28596=AXIS2_PLACEMENT_3D('',#43242,#32955,#32956);
#28597=AXIS2_PLACEMENT_3D('',#43246,#32958,#32959);
#28598=AXIS2_PLACEMENT_3D('',#43248,#32960,#32961);
#28599=AXIS2_PLACEMENT_3D('',#43250,#32962,#32963);
#28600=AXIS2_PLACEMENT_3D('',#43254,#32965,#32966);
#28601=AXIS2_PLACEMENT_3D('',#43258,#32968,#32969);
#28602=AXIS2_PLACEMENT_3D('',#43260,#32970,#32971);
#28603=AXIS2_PLACEMENT_3D('',#43262,#32972,#32973);
#28604=AXIS2_PLACEMENT_3D('',#43266,#32975,#32976);
#28605=AXIS2_PLACEMENT_3D('',#43270,#32978,#32979);
#28606=AXIS2_PLACEMENT_3D('',#43272,#32980,#32981);
#28607=AXIS2_PLACEMENT_3D('',#43274,#32982,#32983);
#28608=AXIS2_PLACEMENT_3D('',#43278,#32985,#32986);
#28609=AXIS2_PLACEMENT_3D('',#43282,#32988,#32989);
#28610=AXIS2_PLACEMENT_3D('',#43284,#32990,#32991);
#28611=AXIS2_PLACEMENT_3D('',#43286,#32992,#32993);
#28612=AXIS2_PLACEMENT_3D('',#43290,#32995,#32996);
#28613=AXIS2_PLACEMENT_3D('',#43294,#32998,#32999);
#28614=AXIS2_PLACEMENT_3D('',#43296,#33000,#33001);
#28615=AXIS2_PLACEMENT_3D('',#43298,#33002,#33003);
#28616=AXIS2_PLACEMENT_3D('',#43301,#33005,#33006);
#28617=AXIS2_PLACEMENT_3D('',#43302,#33007,#33008);
#28618=AXIS2_PLACEMENT_3D('',#43308,#33012,#33013);
#28619=AXIS2_PLACEMENT_3D('',#43314,#33017,#33018);
#28620=AXIS2_PLACEMENT_3D('',#43317,#33021,#33022);
#28621=AXIS2_PLACEMENT_3D('',#43321,#33025,#33026);
#28622=AXIS2_PLACEMENT_3D('',#43325,#33029,#33030);
#28623=AXIS2_PLACEMENT_3D('',#43327,#33032,#33033);
#28624=AXIS2_PLACEMENT_3D('',#43333,#33037,#33038);
#28625=AXIS2_PLACEMENT_3D('',#43339,#33042,#33043);
#28626=AXIS2_PLACEMENT_3D('',#43342,#33046,#33047);
#28627=AXIS2_PLACEMENT_3D('',#43346,#33050,#33051);
#28628=AXIS2_PLACEMENT_3D('',#43350,#33054,#33055);
#28629=AXIS2_PLACEMENT_3D('',#43352,#33057,#33058);
#28630=AXIS2_PLACEMENT_3D('',#43358,#33062,#33063);
#28631=AXIS2_PLACEMENT_3D('',#43364,#33067,#33068);
#28632=AXIS2_PLACEMENT_3D('',#43367,#33071,#33072);
#28633=AXIS2_PLACEMENT_3D('',#43371,#33075,#33076);
#28634=AXIS2_PLACEMENT_3D('',#43375,#33079,#33080);
#28635=AXIS2_PLACEMENT_3D('',#43377,#33082,#33083);
#28636=AXIS2_PLACEMENT_3D('',#43383,#33087,#33088);
#28637=AXIS2_PLACEMENT_3D('',#43389,#33092,#33093);
#28638=AXIS2_PLACEMENT_3D('',#43393,#33096,#33097);
#28639=AXIS2_PLACEMENT_3D('',#43397,#33100,#33101);
#28640=AXIS2_PLACEMENT_3D('',#43400,#33104,#33105);
#28641=AXIS2_PLACEMENT_3D('',#43533,#33184,#33185);
#28642=AXIS2_PLACEMENT_3D('',#43541,#33189,#33190);
#28643=AXIS2_PLACEMENT_3D('',#43545,#33193,#33194);
#28644=AXIS2_PLACEMENT_3D('',#43549,#33197,#33198);
#28645=AXIS2_PLACEMENT_3D('',#43553,#33201,#33202);
#28646=AXIS2_PLACEMENT_3D('',#43555,#33204,#33205);
#28647=AXIS2_PLACEMENT_3D('',#43559,#33208,#33209);
#28648=AXIS2_PLACEMENT_3D('',#43563,#33212,#33213);
#28649=AXIS2_PLACEMENT_3D('',#43565,#33215,#33216);
#28650=AXIS2_PLACEMENT_3D('',#43569,#33219,#33220);
#28651=AXIS2_PLACEMENT_3D('',#43573,#33223,#33224);
#28652=AXIS2_PLACEMENT_3D('',#43575,#33226,#33227);
#28653=AXIS2_PLACEMENT_3D('',#43579,#33230,#33231);
#28654=AXIS2_PLACEMENT_3D('',#43583,#33234,#33235);
#28655=AXIS2_PLACEMENT_3D('',#43585,#33237,#33238);
#28656=AXIS2_PLACEMENT_3D('',#43589,#33241,#33242);
#28657=AXIS2_PLACEMENT_3D('',#43593,#33245,#33246);
#28658=AXIS2_PLACEMENT_3D('',#43595,#33248,#33249);
#28659=AXIS2_PLACEMENT_3D('',#43599,#33252,#33253);
#28660=AXIS2_PLACEMENT_3D('',#43603,#33256,#33257);
#28661=AXIS2_PLACEMENT_3D('',#43605,#33259,#33260);
#28662=AXIS2_PLACEMENT_3D('',#43609,#33263,#33264);
#28663=AXIS2_PLACEMENT_3D('',#43613,#33267,#33268);
#28664=AXIS2_PLACEMENT_3D('',#43615,#33270,#33271);
#28665=AXIS2_PLACEMENT_3D('',#43619,#33274,#33275);
#28666=AXIS2_PLACEMENT_3D('',#43623,#33278,#33279);
#28667=AXIS2_PLACEMENT_3D('',#43625,#33281,#33282);
#28668=AXIS2_PLACEMENT_3D('',#43629,#33285,#33286);
#28669=AXIS2_PLACEMENT_3D('',#43633,#33289,#33290);
#28670=AXIS2_PLACEMENT_3D('',#43635,#33292,#33293);
#28671=AXIS2_PLACEMENT_3D('',#43639,#33296,#33297);
#28672=AXIS2_PLACEMENT_3D('',#43643,#33300,#33301);
#28673=AXIS2_PLACEMENT_3D('',#43645,#33303,#33304);
#28674=AXIS2_PLACEMENT_3D('',#43649,#33307,#33308);
#28675=AXIS2_PLACEMENT_3D('',#43653,#33311,#33312);
#28676=AXIS2_PLACEMENT_3D('',#43655,#33314,#33315);
#28677=AXIS2_PLACEMENT_3D('',#43659,#33318,#33319);
#28678=AXIS2_PLACEMENT_3D('',#43663,#33322,#33323);
#28679=AXIS2_PLACEMENT_3D('',#43665,#33325,#33326);
#28680=AXIS2_PLACEMENT_3D('',#43669,#33329,#33330);
#28681=AXIS2_PLACEMENT_3D('',#43673,#33333,#33334);
#28682=AXIS2_PLACEMENT_3D('',#43675,#33336,#33337);
#28683=AXIS2_PLACEMENT_3D('',#43679,#33340,#33341);
#28684=AXIS2_PLACEMENT_3D('',#43683,#33344,#33345);
#28685=AXIS2_PLACEMENT_3D('',#43685,#33347,#33348);
#28686=AXIS2_PLACEMENT_3D('',#43689,#33351,#33352);
#28687=AXIS2_PLACEMENT_3D('',#43693,#33355,#33356);
#28688=AXIS2_PLACEMENT_3D('',#43695,#33358,#33359);
#28689=AXIS2_PLACEMENT_3D('',#43699,#33362,#33363);
#28690=AXIS2_PLACEMENT_3D('',#43703,#33366,#33367);
#28691=AXIS2_PLACEMENT_3D('',#43705,#33369,#33370);
#28692=AXIS2_PLACEMENT_3D('',#43709,#33373,#33374);
#28693=AXIS2_PLACEMENT_3D('',#43713,#33377,#33378);
#28694=AXIS2_PLACEMENT_3D('',#43715,#33380,#33381);
#28695=AXIS2_PLACEMENT_3D('',#43719,#33384,#33385);
#28696=AXIS2_PLACEMENT_3D('',#43723,#33388,#33389);
#28697=AXIS2_PLACEMENT_3D('',#43725,#33391,#33392);
#28698=AXIS2_PLACEMENT_3D('',#43729,#33395,#33396);
#28699=AXIS2_PLACEMENT_3D('',#43733,#33399,#33400);
#28700=AXIS2_PLACEMENT_3D('',#43735,#33402,#33403);
#28701=AXIS2_PLACEMENT_3D('',#43739,#33406,#33407);
#28702=AXIS2_PLACEMENT_3D('',#43743,#33410,#33411);
#28703=AXIS2_PLACEMENT_3D('',#43747,#33414,#33415);
#28704=AXIS2_PLACEMENT_3D('',#43749,#33417,#33418);
#28705=AXIS2_PLACEMENT_3D('',#43753,#33421,#33422);
#28706=AXIS2_PLACEMENT_3D('',#43755,#33424,#33425);
#28707=AXIS2_PLACEMENT_3D('',#43759,#33428,#33429);
#28708=AXIS2_PLACEMENT_3D('',#43763,#33432,#33433);
#28709=AXIS2_PLACEMENT_3D('',#43765,#33435,#33436);
#28710=AXIS2_PLACEMENT_3D('',#43769,#33439,#33440);
#28711=AXIS2_PLACEMENT_3D('',#43773,#33443,#33444);
#28712=AXIS2_PLACEMENT_3D('',#43775,#33446,#33447);
#28713=AXIS2_PLACEMENT_3D('',#43779,#33450,#33451);
#28714=AXIS2_PLACEMENT_3D('',#43783,#33454,#33455);
#28715=AXIS2_PLACEMENT_3D('',#43785,#33457,#33458);
#28716=AXIS2_PLACEMENT_3D('',#43789,#33461,#33462);
#28717=AXIS2_PLACEMENT_3D('',#43793,#33465,#33466);
#28718=AXIS2_PLACEMENT_3D('',#43795,#33468,#33469);
#28719=AXIS2_PLACEMENT_3D('',#43799,#33472,#33473);
#28720=AXIS2_PLACEMENT_3D('',#43803,#33476,#33477);
#28721=AXIS2_PLACEMENT_3D('',#43805,#33479,#33480);
#28722=AXIS2_PLACEMENT_3D('',#43809,#33483,#33484);
#28723=AXIS2_PLACEMENT_3D('',#43813,#33487,#33488);
#28724=AXIS2_PLACEMENT_3D('',#43815,#33490,#33491);
#28725=AXIS2_PLACEMENT_3D('',#43819,#33494,#33495);
#28726=AXIS2_PLACEMENT_3D('',#43823,#33498,#33499);
#28727=AXIS2_PLACEMENT_3D('',#43825,#33501,#33502);
#28728=AXIS2_PLACEMENT_3D('',#43829,#33505,#33506);
#28729=AXIS2_PLACEMENT_3D('',#43833,#33509,#33510);
#28730=AXIS2_PLACEMENT_3D('',#43835,#33512,#33513);
#28731=AXIS2_PLACEMENT_3D('',#43839,#33516,#33517);
#28732=AXIS2_PLACEMENT_3D('',#43843,#33520,#33521);
#28733=AXIS2_PLACEMENT_3D('',#43845,#33523,#33524);
#28734=AXIS2_PLACEMENT_3D('',#43849,#33527,#33528);
#28735=AXIS2_PLACEMENT_3D('',#43853,#33531,#33532);
#28736=AXIS2_PLACEMENT_3D('',#43855,#33534,#33535);
#28737=AXIS2_PLACEMENT_3D('',#43859,#33538,#33539);
#28738=AXIS2_PLACEMENT_3D('',#43863,#33542,#33543);
#28739=AXIS2_PLACEMENT_3D('',#43865,#33545,#33546);
#28740=AXIS2_PLACEMENT_3D('',#43869,#33549,#33550);
#28741=AXIS2_PLACEMENT_3D('',#43873,#33553,#33554);
#28742=AXIS2_PLACEMENT_3D('',#43875,#33556,#33557);
#28743=AXIS2_PLACEMENT_3D('',#43879,#33560,#33561);
#28744=AXIS2_PLACEMENT_3D('',#43883,#33564,#33565);
#28745=AXIS2_PLACEMENT_3D('',#43885,#33567,#33568);
#28746=AXIS2_PLACEMENT_3D('',#43889,#33571,#33572);
#28747=AXIS2_PLACEMENT_3D('',#43893,#33575,#33576);
#28748=AXIS2_PLACEMENT_3D('',#43895,#33578,#33579);
#28749=AXIS2_PLACEMENT_3D('',#43899,#33582,#33583);
#28750=AXIS2_PLACEMENT_3D('',#43903,#33586,#33587);
#28751=AXIS2_PLACEMENT_3D('',#43905,#33589,#33590);
#28752=AXIS2_PLACEMENT_3D('',#43909,#33593,#33594);
#28753=AXIS2_PLACEMENT_3D('',#43913,#33597,#33598);
#28754=AXIS2_PLACEMENT_3D('',#43915,#33600,#33601);
#28755=AXIS2_PLACEMENT_3D('',#43919,#33604,#33605);
#28756=AXIS2_PLACEMENT_3D('',#43923,#33608,#33609);
#28757=AXIS2_PLACEMENT_3D('',#43925,#33611,#33612);
#28758=AXIS2_PLACEMENT_3D('',#43929,#33615,#33616);
#28759=AXIS2_PLACEMENT_3D('',#43933,#33619,#33620);
#28760=AXIS2_PLACEMENT_3D('',#43935,#33622,#33623);
#28761=AXIS2_PLACEMENT_3D('',#43939,#33626,#33627);
#28762=AXIS2_PLACEMENT_3D('',#43943,#33630,#33631);
#28763=AXIS2_PLACEMENT_3D('',#43945,#33633,#33634);
#28764=AXIS2_PLACEMENT_3D('',#43949,#33637,#33638);
#28765=AXIS2_PLACEMENT_3D('',#43953,#33641,#33642);
#28766=AXIS2_PLACEMENT_3D('',#43955,#33644,#33645);
#28767=AXIS2_PLACEMENT_3D('',#43959,#33648,#33649);
#28768=AXIS2_PLACEMENT_3D('',#43963,#33652,#33653);
#28769=AXIS2_PLACEMENT_3D('',#43965,#33655,#33656);
#28770=AXIS2_PLACEMENT_3D('',#43969,#33659,#33660);
#28771=AXIS2_PLACEMENT_3D('',#43973,#33663,#33664);
#28772=AXIS2_PLACEMENT_3D('',#43975,#33666,#33667);
#28773=AXIS2_PLACEMENT_3D('',#43979,#33670,#33671);
#28774=AXIS2_PLACEMENT_3D('',#43983,#33674,#33675);
#28775=AXIS2_PLACEMENT_3D('',#43985,#33677,#33678);
#28776=AXIS2_PLACEMENT_3D('',#43989,#33681,#33682);
#28777=AXIS2_PLACEMENT_3D('',#43993,#33685,#33686);
#28778=AXIS2_PLACEMENT_3D('',#43995,#33688,#33689);
#28779=AXIS2_PLACEMENT_3D('',#44004,#33694,#33695);
#28780=AXIS2_PLACEMENT_3D('',#44007,#33698,#33699);
#28781=AXIS2_PLACEMENT_3D('',#44162,#33791,#33792);
#28782=AXIS2_PLACEMENT_3D('',#44169,#33796,#33797);
#28783=AXIS2_PLACEMENT_3D('',#44170,#33798,#33799);
#28784=AXIS2_PLACEMENT_3D('',#44172,#33801,#33802);
#28785=AXIS2_PLACEMENT_3D('',#44178,#33806,#33807);
#28786=AXIS2_PLACEMENT_3D('',#44180,#33809,#33810);
#28787=AXIS2_PLACEMENT_3D('',#44182,#33812,#33813);
#28788=AXIS2_PLACEMENT_3D('',#44188,#33817,#33818);
#28789=AXIS2_PLACEMENT_3D('',#44190,#33820,#33821);
#28790=AXIS2_PLACEMENT_3D('',#44192,#33823,#33824);
#28791=AXIS2_PLACEMENT_3D('',#44196,#33827,#33828);
#28792=AXIS2_PLACEMENT_3D('',#44200,#33831,#33832);
#28793=AXIS2_PLACEMENT_3D('',#44206,#33836,#33837);
#28794=AXIS2_PLACEMENT_3D('',#44208,#33839,#33840);
#28795=AXIS2_PLACEMENT_3D('',#44210,#33842,#33843);
#28796=AXIS2_PLACEMENT_3D('',#44216,#33847,#33848);
#28797=AXIS2_PLACEMENT_3D('',#44218,#33850,#33851);
#28798=AXIS2_PLACEMENT_3D('',#44220,#33853,#33854);
#28799=AXIS2_PLACEMENT_3D('',#44224,#33857,#33858);
#28800=AXIS2_PLACEMENT_3D('',#44228,#33861,#33862);
#28801=AXIS2_PLACEMENT_3D('',#44234,#33866,#33867);
#28802=AXIS2_PLACEMENT_3D('',#44236,#33869,#33870);
#28803=AXIS2_PLACEMENT_3D('',#44238,#33872,#33873);
#28804=AXIS2_PLACEMENT_3D('',#44244,#33877,#33878);
#28805=AXIS2_PLACEMENT_3D('',#44246,#33880,#33881);
#28806=AXIS2_PLACEMENT_3D('',#44248,#33883,#33884);
#28807=AXIS2_PLACEMENT_3D('',#44252,#33887,#33888);
#28808=AXIS2_PLACEMENT_3D('',#44256,#33891,#33892);
#28809=AXIS2_PLACEMENT_3D('',#44260,#33895,#33896);
#28810=AXIS2_PLACEMENT_3D('',#44264,#33899,#33900);
#28811=AXIS2_PLACEMENT_3D('',#44266,#33902,#33903);
#28812=AXIS2_PLACEMENT_3D('',#44272,#33907,#33908);
#28813=AXIS2_PLACEMENT_3D('',#44274,#33910,#33911);
#28814=AXIS2_PLACEMENT_3D('',#44276,#33913,#33914);
#28815=AXIS2_PLACEMENT_3D('',#44282,#33918,#33919);
#28816=AXIS2_PLACEMENT_3D('',#44284,#33921,#33922);
#28817=AXIS2_PLACEMENT_3D('',#44286,#33924,#33925);
#28818=AXIS2_PLACEMENT_3D('',#44290,#33928,#33929);
#28819=AXIS2_PLACEMENT_3D('',#44294,#33932,#33933);
#28820=AXIS2_PLACEMENT_3D('',#44300,#33937,#33938);
#28821=AXIS2_PLACEMENT_3D('',#44302,#33940,#33941);
#28822=AXIS2_PLACEMENT_3D('',#44304,#33943,#33944);
#28823=AXIS2_PLACEMENT_3D('',#44310,#33948,#33949);
#28824=AXIS2_PLACEMENT_3D('',#44312,#33951,#33952);
#28825=AXIS2_PLACEMENT_3D('',#44314,#33954,#33955);
#28826=AXIS2_PLACEMENT_3D('',#44318,#33958,#33959);
#28827=AXIS2_PLACEMENT_3D('',#44322,#33962,#33963);
#28828=AXIS2_PLACEMENT_3D('',#44328,#33967,#33968);
#28829=AXIS2_PLACEMENT_3D('',#44330,#33970,#33971);
#28830=AXIS2_PLACEMENT_3D('',#44332,#33973,#33974);
#28831=AXIS2_PLACEMENT_3D('',#44338,#33978,#33979);
#28832=AXIS2_PLACEMENT_3D('',#44340,#33981,#33982);
#28833=AXIS2_PLACEMENT_3D('',#44342,#33984,#33985);
#28834=AXIS2_PLACEMENT_3D('',#44346,#33988,#33989);
#28835=AXIS2_PLACEMENT_3D('',#44350,#33992,#33993);
#28836=AXIS2_PLACEMENT_3D('',#44356,#33997,#33998);
#28837=AXIS2_PLACEMENT_3D('',#44358,#34000,#34001);
#28838=AXIS2_PLACEMENT_3D('',#44360,#34003,#34004);
#28839=AXIS2_PLACEMENT_3D('',#44366,#34008,#34009);
#28840=AXIS2_PLACEMENT_3D('',#44368,#34011,#34012);
#28841=AXIS2_PLACEMENT_3D('',#44370,#34014,#34015);
#28842=AXIS2_PLACEMENT_3D('',#44374,#34018,#34019);
#28843=AXIS2_PLACEMENT_3D('',#44378,#34022,#34023);
#28844=AXIS2_PLACEMENT_3D('',#44384,#34027,#34028);
#28845=AXIS2_PLACEMENT_3D('',#44386,#34030,#34031);
#28846=AXIS2_PLACEMENT_3D('',#44388,#34033,#34034);
#28847=AXIS2_PLACEMENT_3D('',#44394,#34038,#34039);
#28848=AXIS2_PLACEMENT_3D('',#44396,#34041,#34042);
#28849=AXIS2_PLACEMENT_3D('',#44398,#34044,#34045);
#28850=AXIS2_PLACEMENT_3D('',#44402,#34048,#34049);
#28851=AXIS2_PLACEMENT_3D('',#44406,#34052,#34053);
#28852=AXIS2_PLACEMENT_3D('',#44412,#34057,#34058);
#28853=AXIS2_PLACEMENT_3D('',#44414,#34060,#34061);
#28854=AXIS2_PLACEMENT_3D('',#44416,#34063,#34064);
#28855=AXIS2_PLACEMENT_3D('',#44422,#34068,#34069);
#28856=AXIS2_PLACEMENT_3D('',#44424,#34071,#34072);
#28857=AXIS2_PLACEMENT_3D('',#44426,#34074,#34075);
#28858=AXIS2_PLACEMENT_3D('',#44430,#34078,#34079);
#28859=AXIS2_PLACEMENT_3D('',#44434,#34082,#34083);
#28860=AXIS2_PLACEMENT_3D('',#44440,#34087,#34088);
#28861=AXIS2_PLACEMENT_3D('',#44442,#34090,#34091);
#28862=AXIS2_PLACEMENT_3D('',#44444,#34093,#34094);
#28863=AXIS2_PLACEMENT_3D('',#44450,#34098,#34099);
#28864=AXIS2_PLACEMENT_3D('',#44452,#34101,#34102);
#28865=AXIS2_PLACEMENT_3D('',#44454,#34104,#34105);
#28866=AXIS2_PLACEMENT_3D('',#44460,#34109,#34110);
#28867=AXIS2_PLACEMENT_3D('',#44462,#34112,#34113);
#28868=AXIS2_PLACEMENT_3D('',#44464,#34115,#34116);
#28869=AXIS2_PLACEMENT_3D('',#44468,#34119,#34120);
#28870=AXIS2_PLACEMENT_3D('',#44472,#34123,#34124);
#28871=AXIS2_PLACEMENT_3D('',#44478,#34128,#34129);
#28872=AXIS2_PLACEMENT_3D('',#44480,#34131,#34132);
#28873=AXIS2_PLACEMENT_3D('',#44482,#34134,#34135);
#28874=AXIS2_PLACEMENT_3D('',#44488,#34139,#34140);
#28875=AXIS2_PLACEMENT_3D('',#44490,#34142,#34143);
#28876=AXIS2_PLACEMENT_3D('',#44492,#34145,#34146);
#28877=AXIS2_PLACEMENT_3D('',#44496,#34149,#34150);
#28878=AXIS2_PLACEMENT_3D('',#44500,#34153,#34154);
#28879=AXIS2_PLACEMENT_3D('',#44506,#34158,#34159);
#28880=AXIS2_PLACEMENT_3D('',#44508,#34161,#34162);
#28881=AXIS2_PLACEMENT_3D('',#44510,#34164,#34165);
#28882=AXIS2_PLACEMENT_3D('',#44516,#34169,#34170);
#28883=AXIS2_PLACEMENT_3D('',#44518,#34172,#34173);
#28884=AXIS2_PLACEMENT_3D('',#44520,#34175,#34176);
#28885=AXIS2_PLACEMENT_3D('',#44524,#34179,#34180);
#28886=AXIS2_PLACEMENT_3D('',#44528,#34183,#34184);
#28887=AXIS2_PLACEMENT_3D('',#44532,#34187,#34188);
#28888=AXIS2_PLACEMENT_3D('',#44536,#34191,#34192);
#28889=AXIS2_PLACEMENT_3D('',#44538,#34194,#34195);
#28890=AXIS2_PLACEMENT_3D('',#44544,#34199,#34200);
#28891=AXIS2_PLACEMENT_3D('',#44546,#34202,#34203);
#28892=AXIS2_PLACEMENT_3D('',#44548,#34205,#34206);
#28893=AXIS2_PLACEMENT_3D('',#44554,#34210,#34211);
#28894=AXIS2_PLACEMENT_3D('',#44556,#34213,#34214);
#28895=AXIS2_PLACEMENT_3D('',#44558,#34216,#34217);
#28896=AXIS2_PLACEMENT_3D('',#44562,#34220,#34221);
#28897=AXIS2_PLACEMENT_3D('',#44566,#34224,#34225);
#28898=AXIS2_PLACEMENT_3D('',#44572,#34229,#34230);
#28899=AXIS2_PLACEMENT_3D('',#44574,#34231,#34232);
#28900=AXIS2_PLACEMENT_3D('',#44576,#34234,#34235);
#28901=AXIS2_PLACEMENT_3D('',#44579,#34237,#34238);
#28902=AXIS2_PLACEMENT_3D('',#44580,#34239,#34240);
#28903=AXIS2_PLACEMENT_3D('',#44586,#34244,#34245);
#28904=AXIS2_PLACEMENT_3D('',#44590,#34248,#34249);
#28905=AXIS2_PLACEMENT_3D('',#44594,#34252,#34253);
#28906=AXIS2_PLACEMENT_3D('',#44596,#34254,#34255);
#28907=AXIS2_PLACEMENT_3D('',#44599,#34257,#34258);
#28908=AXIS2_PLACEMENT_3D('',#44600,#34259,#34260);
#28909=AXIS2_PLACEMENT_3D('',#44601,#34261,#34262);
#28910=AXIS2_PLACEMENT_3D('',#44604,#34265,#34266);
#28911=AXIS2_PLACEMENT_3D('',#44605,#34267,#34268);
#28912=AXIS2_PLACEMENT_3D('',#44606,#34269,#34270);
#28913=AXIS2_PLACEMENT_3D('',#44607,#34271,#34272);
#28914=AXIS2_PLACEMENT_3D('',#44611,#34274,#34275);
#28915=AXIS2_PLACEMENT_3D('',#44613,#34277,#34278);
#28916=AXIS2_PLACEMENT_3D('',#44617,#34281,#34282);
#28917=AXIS2_PLACEMENT_3D('',#44619,#34284,#34285);
#28918=AXIS2_PLACEMENT_3D('',#44625,#34289,#34290);
#28919=AXIS2_PLACEMENT_3D('',#44629,#34293,#34294);
#28920=AXIS2_PLACEMENT_3D('',#44631,#34296,#34297);
#28921=AXIS2_PLACEMENT_3D('',#44632,#34298,#34299);
#28922=AXIS2_PLACEMENT_3D('',#44634,#34301,#34302);
#28923=AXIS2_PLACEMENT_3D('',#44636,#34304,#34305);
#28924=AXIS2_PLACEMENT_3D('',#44637,#34306,#34307);
#28925=AXIS2_PLACEMENT_3D('',#44638,#34308,#34309);
#28926=AXIS2_PLACEMENT_3D('',#44640,#34311,#34312);
#28927=AXIS2_PLACEMENT_3D('',#44641,#34313,#34314);
#28928=AXIS2_PLACEMENT_3D('',#44642,#34315,#34316);
#28929=AXIS2_PLACEMENT_3D('',#44648,#34320,#34321);
#28930=AXIS2_PLACEMENT_3D('',#44650,#34323,#34324);
#28931=AXIS2_PLACEMENT_3D('',#44652,#34326,#34327);
#28932=AXIS2_PLACEMENT_3D('',#44653,#34328,#34329);
#28933=AXIS2_PLACEMENT_3D('',#44654,#34330,#34331);
#28934=AXIS2_PLACEMENT_3D('',#44660,#34335,#34336);
#28935=AXIS2_PLACEMENT_3D('',#44662,#34338,#34339);
#28936=AXIS2_PLACEMENT_3D('',#44664,#34341,#34342);
#28937=AXIS2_PLACEMENT_3D('',#44665,#34343,#34344);
#28938=AXIS2_PLACEMENT_3D('',#44666,#34345,#34346);
#28939=AXIS2_PLACEMENT_3D('',#44668,#34348,#34349);
#28940=AXIS2_PLACEMENT_3D('',#44669,#34350,#34351);
#28941=AXIS2_PLACEMENT_3D('',#44670,#34352,#34353);
#28942=AXIS2_PLACEMENT_3D('',#44676,#34357,#34358);
#28943=AXIS2_PLACEMENT_3D('',#44678,#34360,#34361);
#28944=AXIS2_PLACEMENT_3D('',#44680,#34363,#34364);
#28945=AXIS2_PLACEMENT_3D('',#44681,#34365,#34366);
#28946=AXIS2_PLACEMENT_3D('',#44682,#34367,#34368);
#28947=AXIS2_PLACEMENT_3D('',#44684,#34370,#34371);
#28948=AXIS2_PLACEMENT_3D('',#44685,#34372,#34373);
#28949=AXIS2_PLACEMENT_3D('',#44686,#34374,#34375);
#28950=AXIS2_PLACEMENT_3D('',#44692,#34379,#34380);
#28951=AXIS2_PLACEMENT_3D('',#44694,#34382,#34383);
#28952=AXIS2_PLACEMENT_3D('',#44696,#34385,#34386);
#28953=AXIS2_PLACEMENT_3D('',#44697,#34387,#34388);
#28954=AXIS2_PLACEMENT_3D('',#44698,#34389,#34390);
#28955=AXIS2_PLACEMENT_3D('',#44700,#34392,#34393);
#28956=AXIS2_PLACEMENT_3D('',#44701,#34394,#34395);
#28957=AXIS2_PLACEMENT_3D('',#44702,#34396,#34397);
#28958=AXIS2_PLACEMENT_3D('',#44708,#34401,#34402);
#28959=AXIS2_PLACEMENT_3D('',#44710,#34404,#34405);
#28960=AXIS2_PLACEMENT_3D('',#44712,#34407,#34408);
#28961=AXIS2_PLACEMENT_3D('',#44713,#34409,#34410);
#28962=AXIS2_PLACEMENT_3D('',#44714,#34411,#34412);
#28963=AXIS2_PLACEMENT_3D('',#44720,#34416,#34417);
#28964=AXIS2_PLACEMENT_3D('',#44722,#34419,#34420);
#28965=AXIS2_PLACEMENT_3D('',#44724,#34422,#34423);
#28966=AXIS2_PLACEMENT_3D('',#44725,#34424,#34425);
#28967=AXIS2_PLACEMENT_3D('',#44726,#34426,#34427);
#28968=AXIS2_PLACEMENT_3D('',#44728,#34429,#34430);
#28969=AXIS2_PLACEMENT_3D('',#44729,#34431,#34432);
#28970=AXIS2_PLACEMENT_3D('',#44730,#34433,#34434);
#28971=AXIS2_PLACEMENT_3D('',#44736,#34438,#34439);
#28972=AXIS2_PLACEMENT_3D('',#44738,#34441,#34442);
#28973=AXIS2_PLACEMENT_3D('',#44740,#34444,#34445);
#28974=AXIS2_PLACEMENT_3D('',#44741,#34446,#34447);
#28975=AXIS2_PLACEMENT_3D('',#44742,#34448,#34449);
#28976=AXIS2_PLACEMENT_3D('',#44744,#34451,#34452);
#28977=AXIS2_PLACEMENT_3D('',#44745,#34453,#34454);
#28978=AXIS2_PLACEMENT_3D('',#44746,#34455,#34456);
#28979=AXIS2_PLACEMENT_3D('',#44752,#34460,#34461);
#28980=AXIS2_PLACEMENT_3D('',#44754,#34463,#34464);
#28981=AXIS2_PLACEMENT_3D('',#44756,#34466,#34467);
#28982=AXIS2_PLACEMENT_3D('',#44757,#34468,#34469);
#28983=AXIS2_PLACEMENT_3D('',#44758,#34470,#34471);
#28984=AXIS2_PLACEMENT_3D('',#44760,#34473,#34474);
#28985=AXIS2_PLACEMENT_3D('',#44761,#34475,#34476);
#28986=AXIS2_PLACEMENT_3D('',#44762,#34477,#34478);
#28987=AXIS2_PLACEMENT_3D('',#44768,#34482,#34483);
#28988=AXIS2_PLACEMENT_3D('',#44770,#34485,#34486);
#28989=AXIS2_PLACEMENT_3D('',#44772,#34488,#34489);
#28990=AXIS2_PLACEMENT_3D('',#44773,#34490,#34491);
#28991=AXIS2_PLACEMENT_3D('',#44774,#34492,#34493);
#28992=AXIS2_PLACEMENT_3D('',#44776,#34495,#34496);
#28993=AXIS2_PLACEMENT_3D('',#44777,#34497,#34498);
#28994=AXIS2_PLACEMENT_3D('',#44778,#34499,#34500);
#28995=AXIS2_PLACEMENT_3D('',#44784,#34504,#34505);
#28996=AXIS2_PLACEMENT_3D('',#44786,#34507,#34508);
#28997=AXIS2_PLACEMENT_3D('',#44788,#34510,#34511);
#28998=AXIS2_PLACEMENT_3D('',#44789,#34512,#34513);
#28999=AXIS2_PLACEMENT_3D('',#44790,#34514,#34515);
#29000=AXIS2_PLACEMENT_3D('',#44792,#34517,#34518);
#29001=AXIS2_PLACEMENT_3D('',#44793,#34519,#34520);
#29002=AXIS2_PLACEMENT_3D('',#44795,#34522,#34523);
#29003=AXIS2_PLACEMENT_3D('',#44796,#34524,#34525);
#29004=AXIS2_PLACEMENT_3D('',#44802,#34529,#34530);
#29005=AXIS2_PLACEMENT_3D('',#44804,#34532,#34533);
#29006=AXIS2_PLACEMENT_3D('',#44806,#34535,#34536);
#29007=AXIS2_PLACEMENT_3D('',#44807,#34537,#34538);
#29008=AXIS2_PLACEMENT_3D('',#44808,#34539,#34540);
#29009=AXIS2_PLACEMENT_3D('',#44810,#34542,#34543);
#29010=AXIS2_PLACEMENT_3D('',#44811,#34544,#34545);
#29011=AXIS2_PLACEMENT_3D('',#44812,#34546,#34547);
#29012=AXIS2_PLACEMENT_3D('',#44818,#34551,#34552);
#29013=AXIS2_PLACEMENT_3D('',#44820,#34554,#34555);
#29014=AXIS2_PLACEMENT_3D('',#44822,#34557,#34558);
#29015=AXIS2_PLACEMENT_3D('',#44823,#34559,#34560);
#29016=AXIS2_PLACEMENT_3D('',#44824,#34561,#34562);
#29017=AXIS2_PLACEMENT_3D('',#44830,#34566,#34567);
#29018=AXIS2_PLACEMENT_3D('',#44832,#34569,#34570);
#29019=AXIS2_PLACEMENT_3D('',#44834,#34572,#34573);
#29020=AXIS2_PLACEMENT_3D('',#44835,#34574,#34575);
#29021=AXIS2_PLACEMENT_3D('',#44837,#34577,#34578);
#29022=AXIS2_PLACEMENT_3D('',#44838,#34579,#34580);
#29023=AXIS2_PLACEMENT_3D('',#44840,#34582,#34583);
#29024=AXIS2_PLACEMENT_3D('',#44841,#34584,#34585);
#29025=AXIS2_PLACEMENT_3D('',#44845,#34588,#34589);
#29026=AXIS2_PLACEMENT_3D('',#44849,#34592,#34593);
#29027=AXIS2_PLACEMENT_3D('',#44851,#34595,#34596);
#29028=AXIS2_PLACEMENT_3D('',#44852,#34597,#34598);
#29029=AXIS2_PLACEMENT_3D('',#44858,#34602,#34603);
#29030=AXIS2_PLACEMENT_3D('',#44860,#34605,#34606);
#29031=AXIS2_PLACEMENT_3D('',#44862,#34608,#34609);
#29032=AXIS2_PLACEMENT_3D('',#44863,#34610,#34611);
#29033=AXIS2_PLACEMENT_3D('',#44867,#34614,#34615);
#29034=AXIS2_PLACEMENT_3D('',#44871,#34618,#34619);
#29035=AXIS2_PLACEMENT_3D('',#44873,#34621,#34622);
#29036=AXIS2_PLACEMENT_3D('',#44874,#34623,#34624);
#29037=AXIS2_PLACEMENT_3D('',#44876,#34626,#34627);
#29038=AXIS2_PLACEMENT_3D('',#44877,#34628,#34629);
#29039=AXIS2_PLACEMENT_3D('',#44881,#34632,#34633);
#29040=AXIS2_PLACEMENT_3D('',#44885,#34636,#34637);
#29041=AXIS2_PLACEMENT_3D('',#44887,#34639,#34640);
#29042=AXIS2_PLACEMENT_3D('',#44888,#34641,#34642);
#29043=AXIS2_PLACEMENT_3D('',#44894,#34646,#34647);
#29044=AXIS2_PLACEMENT_3D('',#44896,#34649,#34650);
#29045=AXIS2_PLACEMENT_3D('',#44898,#34652,#34653);
#29046=AXIS2_PLACEMENT_3D('',#44899,#34654,#34655);
#29047=AXIS2_PLACEMENT_3D('',#44903,#34658,#34659);
#29048=AXIS2_PLACEMENT_3D('',#44907,#34662,#34663);
#29049=AXIS2_PLACEMENT_3D('',#44909,#34665,#34666);
#29050=AXIS2_PLACEMENT_3D('',#44910,#34667,#34668);
#29051=AXIS2_PLACEMENT_3D('',#44912,#34670,#34671);
#29052=AXIS2_PLACEMENT_3D('',#44913,#34672,#34673);
#29053=AXIS2_PLACEMENT_3D('',#44917,#34676,#34677);
#29054=AXIS2_PLACEMENT_3D('',#44921,#34680,#34681);
#29055=AXIS2_PLACEMENT_3D('',#44923,#34683,#34684);
#29056=AXIS2_PLACEMENT_3D('',#44924,#34685,#34686);
#29057=AXIS2_PLACEMENT_3D('',#44930,#34690,#34691);
#29058=AXIS2_PLACEMENT_3D('',#44932,#34693,#34694);
#29059=AXIS2_PLACEMENT_3D('',#44934,#34696,#34697);
#29060=AXIS2_PLACEMENT_3D('',#44935,#34698,#34699);
#29061=AXIS2_PLACEMENT_3D('',#44939,#34702,#34703);
#29062=AXIS2_PLACEMENT_3D('',#44943,#34706,#34707);
#29063=AXIS2_PLACEMENT_3D('',#44945,#34709,#34710);
#29064=AXIS2_PLACEMENT_3D('',#44946,#34711,#34712);
#29065=AXIS2_PLACEMENT_3D('',#44952,#34716,#34717);
#29066=AXIS2_PLACEMENT_3D('',#44954,#34719,#34720);
#29067=AXIS2_PLACEMENT_3D('',#44956,#34722,#34723);
#29068=AXIS2_PLACEMENT_3D('',#44957,#34724,#34725);
#29069=AXIS2_PLACEMENT_3D('',#44958,#34726,#34727);
#29070=AXIS2_PLACEMENT_3D('',#44959,#34728,#34729);
#29071=AXIS2_PLACEMENT_3D('',#44962,#34730,#34731);
#29072=AXIS2_PLACEMENT_3D('',#44968,#34735,#34736);
#29073=AXIS2_PLACEMENT_3D('',#44974,#34740,#34741);
#29074=AXIS2_PLACEMENT_3D('',#44980,#34745,#34746);
#29075=AXIS2_PLACEMENT_3D('',#44981,#34747,#34748);
#29076=AXIS2_PLACEMENT_3D('',#44983,#34750,#34751);
#29077=AXIS2_PLACEMENT_3D('',#44984,#34752,#34753);
#29078=AXIS2_PLACEMENT_3D('',#45065,#34755,#34756);
#29079=AXIS2_PLACEMENT_3D('',#45067,#34757,#34758);
#29080=AXIS2_PLACEMENT_3D('',#45068,#34759,#34760);
#29081=AXIS2_PLACEMENT_3D('',#45070,#34761,#34762);
#29082=AXIS2_PLACEMENT_3D('',#45072,#34764,#34765);
#29083=AXIS2_PLACEMENT_3D('',#45074,#34766,#34767);
#29084=AXIS2_PLACEMENT_3D('',#45077,#34770,#34771);
#29085=AXIS2_PLACEMENT_3D('',#45079,#34772,#34773);
#29086=AXIS2_PLACEMENT_3D('',#45081,#34775,#34776);
#29087=AXIS2_PLACEMENT_3D('',#45083,#34777,#34778);
#29088=AXIS2_PLACEMENT_3D('',#45085,#34780,#34781);
#29089=AXIS2_PLACEMENT_3D('',#45087,#34782,#34783);
#29090=AXIS2_PLACEMENT_3D('',#45088,#34784,#34785);
#29091=AXIS2_PLACEMENT_3D('',#45090,#34786,#34787);
#29092=AXIS2_PLACEMENT_3D('',#45092,#34789,#34790);
#29093=AXIS2_PLACEMENT_3D('',#45094,#34791,#34792);
#29094=AXIS2_PLACEMENT_3D('',#45095,#34793,#34794);
#29095=AXIS2_PLACEMENT_3D('',#45097,#34795,#34796);
#29096=AXIS2_PLACEMENT_3D('',#45099,#34798,#34799);
#29097=AXIS2_PLACEMENT_3D('',#45101,#34800,#34801);
#29098=AXIS2_PLACEMENT_3D('',#45102,#34802,#34803);
#29099=AXIS2_PLACEMENT_3D('',#45104,#34804,#34805);
#29100=AXIS2_PLACEMENT_3D('',#45106,#34807,#34808);
#29101=AXIS2_PLACEMENT_3D('',#45108,#34809,#34810);
#29102=AXIS2_PLACEMENT_3D('',#45109,#34811,#34812);
#29103=AXIS2_PLACEMENT_3D('',#45111,#34813,#34814);
#29104=AXIS2_PLACEMENT_3D('',#45113,#34816,#34817);
#29105=AXIS2_PLACEMENT_3D('',#45115,#34818,#34819);
#29106=AXIS2_PLACEMENT_3D('',#45116,#34820,#34821);
#29107=AXIS2_PLACEMENT_3D('',#45118,#34822,#34823);
#29108=AXIS2_PLACEMENT_3D('',#45120,#34825,#34826);
#29109=AXIS2_PLACEMENT_3D('',#45122,#34827,#34828);
#29110=AXIS2_PLACEMENT_3D('',#45124,#34830,#34831);
#29111=AXIS2_PLACEMENT_3D('',#45125,#34832,#34833);
#29112=AXIS2_PLACEMENT_3D('',#45126,#34834,#34835);
#29113=AXIS2_PLACEMENT_3D('',#45128,#34836,#34837);
#29114=AXIS2_PLACEMENT_3D('',#45131,#34839,#34840);
#29115=AXIS2_PLACEMENT_3D('',#45132,#34841,#34842);
#29116=AXIS2_PLACEMENT_3D('',#45134,#34843,#34844);
#29117=AXIS2_PLACEMENT_3D('',#45135,#34845,#34846);
#29118=AXIS2_PLACEMENT_3D('',#45138,#34848,#34849);
#29119=AXIS2_PLACEMENT_3D('',#45139,#34850,#34851);
#29120=AXIS2_PLACEMENT_3D('',#45141,#34852,#34853);
#29121=AXIS2_PLACEMENT_3D('',#45142,#34854,#34855);
#29122=AXIS2_PLACEMENT_3D('',#45144,#34856,#34857);
#29123=AXIS2_PLACEMENT_3D('',#45146,#34859,#34860);
#29124=AXIS2_PLACEMENT_3D('',#45148,#34861,#34862);
#29125=AXIS2_PLACEMENT_3D('',#45150,#34864,#34865);
#29126=AXIS2_PLACEMENT_3D('',#45152,#34866,#34867);
#29127=AXIS2_PLACEMENT_3D('',#45154,#34869,#34870);
#29128=AXIS2_PLACEMENT_3D('',#45156,#34871,#34872);
#29129=AXIS2_PLACEMENT_3D('',#45157,#34873,#34874);
#29130=AXIS2_PLACEMENT_3D('',#45160,#34876,#34877);
#29131=AXIS2_PLACEMENT_3D('',#45161,#34878,#34879);
#29132=AXIS2_PLACEMENT_3D('',#45163,#34880,#34881);
#29133=AXIS2_PLACEMENT_3D('',#45164,#34882,#34883);
#29134=AXIS2_PLACEMENT_3D('',#45166,#34884,#34885);
#29135=AXIS2_PLACEMENT_3D('',#45168,#34887,#34888);
#29136=AXIS2_PLACEMENT_3D('',#45170,#34889,#34890);
#29137=AXIS2_PLACEMENT_3D('',#45171,#34891,#34892);
#29138=AXIS2_PLACEMENT_3D('',#45174,#34894,#34895);
#29139=AXIS2_PLACEMENT_3D('',#45175,#34896,#34897);
#29140=AXIS2_PLACEMENT_3D('',#45178,#34899,#34900);
#29141=AXIS2_PLACEMENT_3D('',#45179,#34901,#34902);
#29142=AXIS2_PLACEMENT_3D('',#45182,#34904,#34905);
#29143=AXIS2_PLACEMENT_3D('',#45183,#34906,#34907);
#29144=AXIS2_PLACEMENT_3D('',#45184,#34908,#34909);
#29145=AXIS2_PLACEMENT_3D('',#45185,#34910,#34911);
#29146=AXIS2_PLACEMENT_3D('',#45187,#34912,#34913);
#29147=AXIS2_PLACEMENT_3D('',#45191,#34915,#34916);
#29148=AXIS2_PLACEMENT_3D('',#45192,#34917,#34918);
#29149=AXIS2_PLACEMENT_3D('',#45193,#34919,#34920);
#29150=AXIS2_PLACEMENT_3D('',#45196,#34922,#34923);
#29151=AXIS2_PLACEMENT_3D('',#45197,#34924,#34925);
#29152=AXIS2_PLACEMENT_3D('',#45199,#34926,#34927);
#29153=AXIS2_PLACEMENT_3D('',#45200,#34928,#34929);
#29154=AXIS2_PLACEMENT_3D('',#45202,#34930,#34931);
#29155=AXIS2_PLACEMENT_3D('',#45205,#34933,#34934);
#29156=AXIS2_PLACEMENT_3D('',#45206,#34935,#34936);
#29157=AXIS2_PLACEMENT_3D('',#45208,#34937,#34938);
#29158=AXIS2_PLACEMENT_3D('',#45209,#34939,#34940);
#29159=AXIS2_PLACEMENT_3D('',#45211,#34942,#34943);
#29160=AXIS2_PLACEMENT_3D('',#45213,#34944,#34945);
#29161=AXIS2_PLACEMENT_3D('',#45215,#34947,#34948);
#29162=AXIS2_PLACEMENT_3D('',#45217,#34949,#34950);
#29163=AXIS2_PLACEMENT_3D('',#45218,#34951,#34952);
#29164=AXIS2_PLACEMENT_3D('',#45221,#34954,#34955);
#29165=AXIS2_PLACEMENT_3D('',#45222,#34956,#34957);
#29166=AXIS2_PLACEMENT_3D('',#45223,#34958,#34959);
#29167=AXIS2_PLACEMENT_3D('',#45224,#34960,#34961);
#29168=AXIS2_PLACEMENT_3D('',#45226,#34962,#34963);
#29169=AXIS2_PLACEMENT_3D('',#45229,#34965,#34966);
#29170=AXIS2_PLACEMENT_3D('',#45230,#34967,#34968);
#29171=AXIS2_PLACEMENT_3D('',#45232,#34969,#34970);
#29172=AXIS2_PLACEMENT_3D('',#45233,#34971,#34972);
#29173=AXIS2_PLACEMENT_3D('',#45235,#34973,#34974);
#29174=AXIS2_PLACEMENT_3D('',#45237,#34976,#34977);
#29175=AXIS2_PLACEMENT_3D('',#45239,#34978,#34979);
#29176=AXIS2_PLACEMENT_3D('',#45241,#34981,#34982);
#29177=AXIS2_PLACEMENT_3D('',#45242,#34983,#34984);
#29178=AXIS2_PLACEMENT_3D('',#45243,#34985,#34986);
#29179=AXIS2_PLACEMENT_3D('',#45245,#34987,#34988);
#29180=AXIS2_PLACEMENT_3D('',#45246,#34989,#34990);
#29181=AXIS2_PLACEMENT_3D('',#45248,#34991,#34992);
#29182=AXIS2_PLACEMENT_3D('',#45250,#34994,#34995);
#29183=AXIS2_PLACEMENT_3D('',#45252,#34996,#34997);
#29184=AXIS2_PLACEMENT_3D('',#45254,#34999,#35000);
#29185=AXIS2_PLACEMENT_3D('',#45256,#35001,#35002);
#29186=AXIS2_PLACEMENT_3D('',#45258,#35004,#35005);
#29187=AXIS2_PLACEMENT_3D('',#45259,#35006,#35007);
#29188=AXIS2_PLACEMENT_3D('',#45260,#35008,#35009);
#29189=AXIS2_PLACEMENT_3D('',#45262,#35010,#35011);
#29190=AXIS2_PLACEMENT_3D('',#45265,#35013,#35014);
#29191=AXIS2_PLACEMENT_3D('',#45266,#35015,#35016);
#29192=AXIS2_PLACEMENT_3D('',#45268,#35017,#35018);
#29193=AXIS2_PLACEMENT_3D('',#45269,#35019,#35020);
#29194=AXIS2_PLACEMENT_3D('',#45271,#35021,#35022);
#29195=AXIS2_PLACEMENT_3D('',#45273,#35024,#35025);
#29196=AXIS2_PLACEMENT_3D('',#45274,#35026,#35027);
#29197=AXIS2_PLACEMENT_3D('',#45275,#35028,#35029);
#29198=AXIS2_PLACEMENT_3D('',#45277,#35030,#35031);
#29199=AXIS2_PLACEMENT_3D('',#45278,#35032,#35033);
#29200=AXIS2_PLACEMENT_3D('',#45279,#35034,#35035);
#29201=AXIS2_PLACEMENT_3D('',#45280,#35036,#35037);
#29202=AXIS2_PLACEMENT_3D('',#45285,#35039,#35040);
#29203=AXIS2_PLACEMENT_3D('',#45292,#35042,#35043);
#29204=AXIS2_PLACEMENT_3D('',#45294,#35044,#35045);
#29205=AXIS2_PLACEMENT_3D('',#45300,#35046,#35047);
#29206=AXIS2_PLACEMENT_3D('',#45301,#35048,#35049);
#29207=AXIS2_PLACEMENT_3D('',#45305,#35051,#35052);
#29208=AXIS2_PLACEMENT_3D('',#45307,#35054,#35055);
#29209=AXIS2_PLACEMENT_3D('',#45308,#35056,#35057);
#29210=AXIS2_PLACEMENT_3D('',#45309,#35058,#35059);
#29211=AXIS2_PLACEMENT_3D('',#45314,#35061,#35062);
#29212=AXIS2_PLACEMENT_3D('',#45321,#35064,#35065);
#29213=AXIS2_PLACEMENT_3D('',#45326,#35067,#35068);
#29214=AXIS2_PLACEMENT_3D('',#45333,#35070,#35071);
#29215=AXIS2_PLACEMENT_3D('',#45334,#35072,#35073);
#29216=AXIS2_PLACEMENT_3D('',#45335,#35074,#35075);
#29217=AXIS2_PLACEMENT_3D('',#45336,#35076,#35077);
#29218=AXIS2_PLACEMENT_3D('',#45337,#35078,#35079);
#29219=AXIS2_PLACEMENT_3D('',#45338,#35080,#35081);
#29220=AXIS2_PLACEMENT_3D('',#45341,#35084,#35085);
#29221=AXIS2_PLACEMENT_3D('',#45343,#35087,#35088);
#29222=AXIS2_PLACEMENT_3D('',#45345,#35090,#35091);
#29223=AXIS2_PLACEMENT_3D('',#45346,#35092,#35093);
#29224=AXIS2_PLACEMENT_3D('',#45347,#35094,#35095);
#29225=AXIS2_PLACEMENT_3D('',#45356,#35098,#35099);
#29226=AXIS2_PLACEMENT_3D('',#45365,#35102,#35103);
#29227=AXIS2_PLACEMENT_3D('',#45368,#35104,#35105);
#29228=AXIS2_PLACEMENT_3D('',#45371,#35108,#35109);
#29229=AXIS2_PLACEMENT_3D('',#45380,#35112,#35113);
#29230=AXIS2_PLACEMENT_3D('',#45389,#35116,#35117);
#29231=AXIS2_PLACEMENT_3D('',#45390,#35118,#35119);
#29232=AXIS2_PLACEMENT_3D('',#45391,#35120,#35121);
#29233=AXIS2_PLACEMENT_3D('',#45392,#35122,#35123);
#29234=AXIS2_PLACEMENT_3D('',#45395,#35124,#35125);
#29235=AXIS2_PLACEMENT_3D('',#45398,#35128,#35129);
#29236=AXIS2_PLACEMENT_3D('',#45401,#35132,#35133);
#29237=AXIS2_PLACEMENT_3D('',#45404,#35134,#35135);
#29238=AXIS2_PLACEMENT_3D('',#45407,#35138,#35139);
#29239=AXIS2_PLACEMENT_3D('',#45408,#35140,#35141);
#29240=AXIS2_PLACEMENT_3D('',#45409,#35142,#35143);
#29241=AXIS2_PLACEMENT_3D('',#45410,#35144,#35145);
#29242=AXIS2_PLACEMENT_3D('',#45413,#35148,#35149);
#29243=AXIS2_PLACEMENT_3D('',#45416,#35150,#35151);
#29244=AXIS2_PLACEMENT_3D('',#45419,#35154,#35155);
#29245=AXIS2_PLACEMENT_3D('',#45420,#35156,#35157);
#29246=AXIS2_PLACEMENT_3D('',#45421,#35158,#35159);
#29247=AXIS2_PLACEMENT_3D('',#45423,#35161,#35162);
#29248=AXIS2_PLACEMENT_3D('',#45424,#35163,#35164);
#29249=AXIS2_PLACEMENT_3D('',#45425,#35165,#35166);
#29250=AXIS2_PLACEMENT_3D('',#45427,#35168,#35169);
#29251=AXIS2_PLACEMENT_3D('',#45428,#35170,#35171);
#29252=AXIS2_PLACEMENT_3D('',#45429,#35172,#35173);
#29253=AXIS2_PLACEMENT_3D('',#45430,#35174,#35175);
#29254=AXIS2_PLACEMENT_3D('',#45432,#35176,#35177);
#29255=AXIS2_PLACEMENT_3D('',#45435,#35179,#35180);
#29256=AXIS2_PLACEMENT_3D('',#45436,#35181,#35182);
#29257=AXIS2_PLACEMENT_3D('',#45485,#35184,#35185);
#29258=AXIS2_PLACEMENT_3D('',#45486,#35186,#35187);
#29259=AXIS2_PLACEMENT_3D('',#45502,#35189,#35190);
#29260=AXIS2_PLACEMENT_3D('',#45518,#35192,#35193);
#29261=AXIS2_PLACEMENT_3D('',#45534,#35195,#35196);
#29262=AXIS2_PLACEMENT_3D('',#45550,#35198,#35199);
#29263=AXIS2_PLACEMENT_3D('',#45566,#35201,#35202);
#29264=AXIS2_PLACEMENT_3D('',#45612,#35204,#35205);
#29265=AXIS2_PLACEMENT_3D('',#45678,#35209,#35210);
#29266=AXIS2_PLACEMENT_3D('',#45684,#35214,#35215);
#29267=AXIS2_PLACEMENT_3D('',#45750,#35219,#35220);
#29268=AXIS2_PLACEMENT_3D('',#45756,#35224,#35225);
#29269=AXIS2_PLACEMENT_3D('',#45792,#35229,#35230);
#29270=AXIS2_PLACEMENT_3D('',#45798,#35234,#35235);
#29271=AXIS2_PLACEMENT_3D('',#45802,#35237,#35238);
#29272=AXIS2_PLACEMENT_3D('',#45804,#35240,#35241);
#29273=AXIS2_PLACEMENT_3D('',#45808,#35244,#35245);
#29274=AXIS2_PLACEMENT_3D('',#45811,#35247,#35248);
#29275=AXIS2_PLACEMENT_3D('',#45812,#35249,#35250);
#29276=AXIS2_PLACEMENT_3D('',#45816,#35253,#35254);
#29277=AXIS2_PLACEMENT_3D('',#45819,#35256,#35257);
#29278=AXIS2_PLACEMENT_3D('',#45820,#35258,#35259);
#29279=AXIS2_PLACEMENT_3D('',#45824,#35262,#35263);
#29280=AXIS2_PLACEMENT_3D('',#45830,#35267,#35268);
#29281=AXIS2_PLACEMENT_3D('',#45836,#35272,#35273);
#29282=AXIS2_PLACEMENT_3D('',#45839,#35275,#35276);
#29283=AXIS2_PLACEMENT_3D('',#45840,#35277,#35278);
#29284=AXIS2_PLACEMENT_3D('',#45841,#35279,#35280);
#29285=AXIS2_PLACEMENT_3D('',#45842,#35281,#35282);
#29286=AXIS2_PLACEMENT_3D('',#45843,#35283,#35284);
#29287=AXIS2_PLACEMENT_3D('',#45844,#35285,#35286);
#29288=AXIS2_PLACEMENT_3D('',#45846,#35288,#35289);
#29289=AXIS2_PLACEMENT_3D('',#45847,#35290,#35291);
#29290=AXIS2_PLACEMENT_3D('',#45848,#35292,#35293);
#29291=AXIS2_PLACEMENT_3D('',#45849,#35294,#35295);
#29292=AXIS2_PLACEMENT_3D('',#45850,#35296,#35297);
#29293=AXIS2_PLACEMENT_3D('',#45851,#35298,#35299);
#29294=AXIS2_PLACEMENT_3D('',#45852,#35300,#35301);
#29295=AXIS2_PLACEMENT_3D('',#45853,#35302,#35303);
#29296=AXIS2_PLACEMENT_3D('',#45854,#35304,#35305);
#29297=AXIS2_PLACEMENT_3D('',#45855,#35306,#35307);
#29298=AXIS2_PLACEMENT_3D('',#45856,#35308,#35309);
#29299=AXIS2_PLACEMENT_3D('',#45858,#35310,#35311);
#29300=AXIS2_PLACEMENT_3D('',#45859,#35312,#35313);
#29301=AXIS2_PLACEMENT_3D('',#45860,#35314,#35315);
#29302=AXIS2_PLACEMENT_3D('',#45862,#35316,#35317);
#29303=AXIS2_PLACEMENT_3D('',#45863,#35318,#35319);
#29304=AXIS2_PLACEMENT_3D('',#45865,#35320,#35321);
#29305=AXIS2_PLACEMENT_3D('',#45867,#35323,#35324);
#29306=AXIS2_PLACEMENT_3D('',#45869,#35326,#35327);
#29307=AXIS2_PLACEMENT_3D('',#45870,#35328,#35329);
#29308=AXIS2_PLACEMENT_3D('',#45879,#35334,#35335);
#29309=AXIS2_PLACEMENT_3D('',#45883,#35337,#35338);
#29310=AXIS2_PLACEMENT_3D('',#45884,#35339,#35340);
#29311=AXIS2_PLACEMENT_3D('',#45885,#35341,#35342);
#29312=AXIS2_PLACEMENT_3D('',#45891,#35346,#35347);
#29313=AXIS2_PLACEMENT_3D('',#45895,#35349,#35350);
#29314=AXIS2_PLACEMENT_3D('',#45896,#35351,#35352);
#29315=AXIS2_PLACEMENT_3D('',#45897,#35353,#35354);
#29316=AXIS2_PLACEMENT_3D('',#45903,#35358,#35359);
#29317=AXIS2_PLACEMENT_3D('',#45907,#35361,#35362);
#29318=AXIS2_PLACEMENT_3D('',#45908,#35363,#35364);
#29319=AXIS2_PLACEMENT_3D('',#45909,#35365,#35366);
#29320=AXIS2_PLACEMENT_3D('',#45915,#35370,#35371);
#29321=AXIS2_PLACEMENT_3D('',#45916,#35372,#35373);
#29322=AXIS2_PLACEMENT_3D('',#45917,#35374,#35375);
#29323=AXIS2_PLACEMENT_3D('',#45918,#35376,#35377);
#29324=AXIS2_PLACEMENT_3D('',#45922,#35379,#35380);
#29325=AXIS2_PLACEMENT_3D('',#45924,#35382,#35383);
#29326=AXIS2_PLACEMENT_3D('',#45928,#35386,#35387);
#29327=AXIS2_PLACEMENT_3D('',#45931,#35389,#35390);
#29328=AXIS2_PLACEMENT_3D('',#45932,#35391,#35392);
#29329=AXIS2_PLACEMENT_3D('',#45936,#35395,#35396);
#29330=AXIS2_PLACEMENT_3D('',#45938,#35397,#35398);
#29331=AXIS2_PLACEMENT_3D('',#45940,#35399,#35400);
#29332=AXIS2_PLACEMENT_3D('',#45942,#35401,#35402);
#29333=AXIS2_PLACEMENT_3D('',#45944,#35403,#35404);
#29334=AXIS2_PLACEMENT_3D('',#45949,#35406,#35407);
#29335=AXIS2_PLACEMENT_3D('',#45953,#35409,#35410);
#29336=AXIS2_PLACEMENT_3D('',#45957,#35412,#35413);
#29337=AXIS2_PLACEMENT_3D('',#45960,#35415,#35416);
#29338=AXIS2_PLACEMENT_3D('',#45961,#35417,#35418);
#29339=AXIS2_PLACEMENT_3D('',#45967,#35422,#35423);
#29340=AXIS2_PLACEMENT_3D('',#45971,#35425,#35426);
#29341=AXIS2_PLACEMENT_3D('',#45972,#35427,#35428);
#29342=AXIS2_PLACEMENT_3D('',#45973,#35429,#35430);
#29343=AXIS2_PLACEMENT_3D('',#45979,#35434,#35435);
#29344=AXIS2_PLACEMENT_3D('',#45983,#35437,#35438);
#29345=AXIS2_PLACEMENT_3D('',#45984,#35439,#35440);
#29346=AXIS2_PLACEMENT_3D('',#45985,#35441,#35442);
#29347=AXIS2_PLACEMENT_3D('',#45990,#35446,#35447);
#29348=AXIS2_PLACEMENT_3D('',#45993,#35449,#35450);
#29349=AXIS2_PLACEMENT_3D('',#45994,#35451,#35452);
#29350=AXIS2_PLACEMENT_3D('',#45998,#35455,#35456);
#29351=AXIS2_PLACEMENT_3D('',#45999,#35457,#35458);
#29352=AXIS2_PLACEMENT_3D('',#46000,#35459,#35460);
#29353=AXIS2_PLACEMENT_3D('',#46003,#35463,#35464);
#29354=AXIS2_PLACEMENT_3D('',#46005,#35466,#35467);
#29355=AXIS2_PLACEMENT_3D('',#46006,#35468,#35469);
#29356=AXIS2_PLACEMENT_3D('',#46008,#35470,#35471);
#29357=AXIS2_PLACEMENT_3D('',#46010,#35472,#35473);
#29358=AXIS2_PLACEMENT_3D('',#46012,#35474,#35475);
#29359=AXIS2_PLACEMENT_3D('',#46014,#35476,#35477);
#29360=AXIS2_PLACEMENT_3D('',#46015,#35478,#35479);
#29361=AXIS2_PLACEMENT_3D('',#46024,#35484,#35485);
#29362=AXIS2_PLACEMENT_3D('',#46028,#35487,#35488);
#29363=AXIS2_PLACEMENT_3D('',#46029,#35489,#35490);
#29364=AXIS2_PLACEMENT_3D('',#46030,#35491,#35492);
#29365=AXIS2_PLACEMENT_3D('',#46036,#35496,#35497);
#29366=AXIS2_PLACEMENT_3D('',#46040,#35499,#35500);
#29367=AXIS2_PLACEMENT_3D('',#46041,#35501,#35502);
#29368=AXIS2_PLACEMENT_3D('',#46042,#35503,#35504);
#29369=AXIS2_PLACEMENT_3D('',#46048,#35508,#35509);
#29370=AXIS2_PLACEMENT_3D('',#46052,#35511,#35512);
#29371=AXIS2_PLACEMENT_3D('',#46053,#35513,#35514);
#29372=AXIS2_PLACEMENT_3D('',#46054,#35515,#35516);
#29373=AXIS2_PLACEMENT_3D('',#46060,#35520,#35521);
#29374=AXIS2_PLACEMENT_3D('',#46061,#35522,#35523);
#29375=AXIS2_PLACEMENT_3D('',#46062,#35524,#35525);
#29376=AXIS2_PLACEMENT_3D('',#46063,#35526,#35527);
#29377=AXIS2_PLACEMENT_3D('',#46066,#35530,#35531);
#29378=AXIS2_PLACEMENT_3D('',#46068,#35533,#35534);
#29379=AXIS2_PLACEMENT_3D('',#46070,#35536,#35537);
#29380=AXIS2_PLACEMENT_3D('',#46072,#35539,#35540);
#29381=AXIS2_PLACEMENT_3D('',#46073,#35541,#35542);
#29382=AXIS2_PLACEMENT_3D('',#46075,#35544,#35545);
#29383=AXIS2_PLACEMENT_3D('',#46077,#35547,#35548);
#29384=AXIS2_PLACEMENT_3D('',#46079,#35550,#35551);
#29385=AXIS2_PLACEMENT_3D('',#46080,#35552,#35553);
#29386=AXIS2_PLACEMENT_3D('',#46082,#35555,#35556);
#29387=AXIS2_PLACEMENT_3D('',#46084,#35558,#35559);
#29388=AXIS2_PLACEMENT_3D('',#46086,#35561,#35562);
#29389=AXIS2_PLACEMENT_3D('',#46088,#35564,#35565);
#29390=AXIS2_PLACEMENT_3D('',#46089,#35566,#35567);
#29391=AXIS2_PLACEMENT_3D('',#46090,#35568,#35569);
#29392=AXIS2_PLACEMENT_3D('',#46097,#35570,#35571);
#29393=AXIS2_PLACEMENT_3D('',#46099,#35572,#35573);
#29394=AXIS2_PLACEMENT_3D('',#46104,#35574,#35575);
#29395=AXIS2_PLACEMENT_3D('',#46105,#35576,#35577);
#29396=AXIS2_PLACEMENT_3D('',#46113,#35579,#35580);
#29397=AXIS2_PLACEMENT_3D('',#46114,#35581,#35582);
#29398=AXIS2_PLACEMENT_3D('',#46128,#35583,#35584);
#29399=AXIS2_PLACEMENT_3D('',#46134,#35585,#35586);
#29400=AXIS2_PLACEMENT_3D('',#46148,#35587,#35588);
#29401=AXIS2_PLACEMENT_3D('',#46162,#35589,#35590);
#29402=AXIS2_PLACEMENT_3D('',#46176,#35591,#35592);
#29403=AXIS2_PLACEMENT_3D('',#46184,#35593,#35594);
#29404=AXIS2_PLACEMENT_3D('',#46187,#35595,#35596);
#29405=AXIS2_PLACEMENT_3D('',#46188,#35597,#35598);
#29406=AXIS2_PLACEMENT_3D('',#46191,#35600,#35601);
#29407=AXIS2_PLACEMENT_3D('',#46192,#35602,#35603);
#29408=AXIS2_PLACEMENT_3D('',#46195,#35604,#35605);
#29409=AXIS2_PLACEMENT_3D('',#46196,#35606,#35607);
#29410=AXIS2_PLACEMENT_3D('',#46198,#35609,#35610);
#29411=AXIS2_PLACEMENT_3D('',#46200,#35611,#35612);
#29412=AXIS2_PLACEMENT_3D('',#46201,#35613,#35614);
#29413=AXIS2_PLACEMENT_3D('',#46207,#35615,#35616);
#29414=AXIS2_PLACEMENT_3D('',#46211,#35617,#35618);
#29415=AXIS2_PLACEMENT_3D('',#46220,#35619,#35620);
#29416=AXIS2_PLACEMENT_3D('',#46221,#35621,#35622);
#29417=AXIS2_PLACEMENT_3D('',#46228,#35626,#35627);
#29418=AXIS2_PLACEMENT_3D('',#46234,#35631,#35632);
#29419=AXIS2_PLACEMENT_3D('',#46241,#35636,#35637);
#29420=AXIS2_PLACEMENT_3D('',#46248,#35641,#35642);
#29421=AXIS2_PLACEMENT_3D('',#46254,#35646,#35647);
#29422=AXIS2_PLACEMENT_3D('',#46257,#35650,#35651);
#29423=AXIS2_PLACEMENT_3D('',#46264,#35655,#35656);
#29424=AXIS2_PLACEMENT_3D('',#46267,#35659,#35660);
#29425=AXIS2_PLACEMENT_3D('',#46274,#35664,#35665);
#29426=AXIS2_PLACEMENT_3D('',#46281,#35669,#35670);
#29427=AXIS2_PLACEMENT_3D('',#46284,#35673,#35674);
#29428=AXIS2_PLACEMENT_3D('',#46287,#35677,#35678);
#29429=AXIS2_PLACEMENT_3D('',#46290,#35681,#35682);
#29430=AXIS2_PLACEMENT_3D('',#46293,#35685,#35686);
#29431=AXIS2_PLACEMENT_3D('',#46296,#35689,#35690);
#29432=AXIS2_PLACEMENT_3D('',#46299,#35693,#35694);
#29433=AXIS2_PLACEMENT_3D('',#46302,#35697,#35698);
#29434=AXIS2_PLACEMENT_3D('',#46304,#35700,#35701);
#29435=AXIS2_PLACEMENT_3D('',#46306,#35703,#35704);
#29436=AXIS2_PLACEMENT_3D('',#46307,#35705,#35706);
#29437=AXIS2_PLACEMENT_3D('',#46308,#35707,#35708);
#29438=AXIS2_PLACEMENT_3D('',#46311,#35709,#35710);
#29439=AXIS2_PLACEMENT_3D('',#46312,#35711,#35712);
#29440=AXIS2_PLACEMENT_3D('',#46314,#35714,#35715);
#29441=AXIS2_PLACEMENT_3D('',#46317,#35716,#35717);
#29442=AXIS2_PLACEMENT_3D('',#46318,#35718,#35719);
#29443=AXIS2_PLACEMENT_3D('',#46351,#35721,#35722);
#29444=AXIS2_PLACEMENT_3D('',#46353,#35724,#35725);
#29445=AXIS2_PLACEMENT_3D('',#46360,#35729,#35730);
#29446=AXIS2_PLACEMENT_3D('',#46366,#35734,#35735);
#29447=AXIS2_PLACEMENT_3D('',#46374,#35740,#35741);
#29448=AXIS2_PLACEMENT_3D('',#46382,#35746,#35747);
#29449=AXIS2_PLACEMENT_3D('',#46389,#35752,#35753);
#29450=AXIS2_PLACEMENT_3D('',#46393,#35756,#35757);
#29451=AXIS2_PLACEMENT_3D('',#46399,#35761,#35762);
#29452=AXIS2_PLACEMENT_3D('',#46406,#35766,#35767);
#29453=AXIS2_PLACEMENT_3D('',#46413,#35771,#35772);
#29454=AXIS2_PLACEMENT_3D('',#46418,#35776,#35777);
#29455=AXIS2_PLACEMENT_3D('',#46421,#35780,#35781);
#29456=AXIS2_PLACEMENT_3D('',#46424,#35784,#35785);
#29457=AXIS2_PLACEMENT_3D('',#46427,#35788,#35789);
#29458=AXIS2_PLACEMENT_3D('',#46432,#35793,#35794);
#29459=AXIS2_PLACEMENT_3D('',#46434,#35796,#35797);
#29460=AXIS2_PLACEMENT_3D('',#46436,#35799,#35800);
#29461=AXIS2_PLACEMENT_3D('',#46437,#35801,#35802);
#29462=AXIS2_PLACEMENT_3D('',#46438,#35803,#35804);
#29463=AXIS2_PLACEMENT_3D('',#46445,#35808,#35809);
#29464=AXIS2_PLACEMENT_3D('',#46451,#35813,#35814);
#29465=AXIS2_PLACEMENT_3D('',#46458,#35818,#35819);
#29466=AXIS2_PLACEMENT_3D('',#46465,#35823,#35824);
#29467=AXIS2_PLACEMENT_3D('',#46471,#35828,#35829);
#29468=AXIS2_PLACEMENT_3D('',#46474,#35832,#35833);
#29469=AXIS2_PLACEMENT_3D('',#46481,#35837,#35838);
#29470=AXIS2_PLACEMENT_3D('',#46484,#35841,#35842);
#29471=AXIS2_PLACEMENT_3D('',#46491,#35846,#35847);
#29472=AXIS2_PLACEMENT_3D('',#46498,#35851,#35852);
#29473=AXIS2_PLACEMENT_3D('',#46501,#35855,#35856);
#29474=AXIS2_PLACEMENT_3D('',#46504,#35859,#35860);
#29475=AXIS2_PLACEMENT_3D('',#46507,#35863,#35864);
#29476=AXIS2_PLACEMENT_3D('',#46510,#35867,#35868);
#29477=AXIS2_PLACEMENT_3D('',#46513,#35871,#35872);
#29478=AXIS2_PLACEMENT_3D('',#46516,#35875,#35876);
#29479=AXIS2_PLACEMENT_3D('',#46519,#35879,#35880);
#29480=AXIS2_PLACEMENT_3D('',#46521,#35882,#35883);
#29481=AXIS2_PLACEMENT_3D('',#46523,#35885,#35886);
#29482=AXIS2_PLACEMENT_3D('',#46524,#35887,#35888);
#29483=AXIS2_PLACEMENT_3D('',#46677,#35890,#35891);
#29484=AXIS2_PLACEMENT_3D('',#46681,#35893,#35894);
#29485=AXIS2_PLACEMENT_3D('',#46682,#35895,#35896);
#29486=AXIS2_PLACEMENT_3D('',#46683,#35897,#35898);
#29487=AXIS2_PLACEMENT_3D('',#46685,#35900,#35901);
#29488=AXIS2_PLACEMENT_3D('',#46687,#35903,#35904);
#29489=AXIS2_PLACEMENT_3D('',#46689,#35906,#35907);
#29490=AXIS2_PLACEMENT_3D('',#46690,#35908,#35909);
#29491=AXIS2_PLACEMENT_3D('',#46691,#35910,#35911);
#29492=AXIS2_PLACEMENT_3D('',#46693,#35913,#35914);
#29493=AXIS2_PLACEMENT_3D('',#46694,#35915,#35916);
#29494=AXIS2_PLACEMENT_3D('',#46696,#35917,#35918);
#29495=AXIS2_PLACEMENT_3D('',#46699,#35921,#35922);
#29496=AXIS2_PLACEMENT_3D('',#46700,#35923,#35924);
#29497=AXIS2_PLACEMENT_3D('',#46701,#35925,#35926);
#29498=AXIS2_PLACEMENT_3D('',#46717,#35928,#35929);
#29499=AXIS2_PLACEMENT_3D('',#46728,#35930,#35931);
#29500=AXIS2_PLACEMENT_3D('',#46776,#35933,#35934);
#29501=AXIS2_PLACEMENT_3D('',#46824,#35936,#35937);
#29502=AXIS2_PLACEMENT_3D('',#46872,#35939,#35940);
#29503=AXIS2_PLACEMENT_3D('',#46926,#35942,#35943);
#29504=AXIS2_PLACEMENT_3D('',#46974,#35945,#35946);
#29505=AXIS2_PLACEMENT_3D('',#47022,#35948,#35949);
#29506=AXIS2_PLACEMENT_3D('',#47076,#35951,#35952);
#29507=AXIS2_PLACEMENT_3D('',#47124,#35954,#35955);
#29508=AXIS2_PLACEMENT_3D('',#47172,#35957,#35958);
#29509=AXIS2_PLACEMENT_3D('',#47220,#35960,#35961);
#29510=AXIS2_PLACEMENT_3D('',#47274,#35963,#35964);
#29511=AXIS2_PLACEMENT_3D('',#47322,#35966,#35967);
#29512=AXIS2_PLACEMENT_3D('',#47370,#35969,#35970);
#29513=AXIS2_PLACEMENT_3D('',#47424,#35972,#35973);
#29514=AXIS2_PLACEMENT_3D('',#47472,#35975,#35976);
#29515=AXIS2_PLACEMENT_3D('',#47520,#35978,#35979);
#29516=AXIS2_PLACEMENT_3D('',#47568,#35981,#35982);
#29517=AXIS2_PLACEMENT_3D('',#47622,#35984,#35985);
#29518=AXIS2_PLACEMENT_3D('',#47670,#35987,#35988);
#29519=AXIS2_PLACEMENT_3D('',#47679,#35990,#35991);
#29520=AXIS2_PLACEMENT_3D('',#47680,#35992,#35993);
#29521=AXIS2_PLACEMENT_3D('',#47695,#35995,#35996);
#29522=AXIS2_PLACEMENT_3D('',#47706,#35997,#35998);
#29523=AXIS2_PLACEMENT_3D('',#47731,#36000,#36001);
#29524=AXIS2_PLACEMENT_3D('',#47756,#36003,#36004);
#29525=AXIS2_PLACEMENT_3D('',#47780,#36006,#36007);
#29526=AXIS2_PLACEMENT_3D('',#47804,#36009,#36010);
#29527=AXIS2_PLACEMENT_3D('',#47829,#36012,#36013);
#29528=AXIS2_PLACEMENT_3D('',#47854,#36015,#36016);
#29529=AXIS2_PLACEMENT_3D('',#47878,#36018,#36019);
#29530=AXIS2_PLACEMENT_3D('',#47903,#36021,#36022);
#29531=AXIS2_PLACEMENT_3D('',#47928,#36024,#36025);
#29532=AXIS2_PLACEMENT_3D('',#47952,#36027,#36028);
#29533=AXIS2_PLACEMENT_3D('',#47976,#36030,#36031);
#29534=AXIS2_PLACEMENT_3D('',#48001,#36033,#36034);
#29535=AXIS2_PLACEMENT_3D('',#48026,#36036,#36037);
#29536=AXIS2_PLACEMENT_3D('',#48050,#36039,#36040);
#29537=AXIS2_PLACEMENT_3D('',#48075,#36042,#36043);
#29538=AXIS2_PLACEMENT_3D('',#48100,#36045,#36046);
#29539=AXIS2_PLACEMENT_3D('',#48124,#36048,#36049);
#29540=AXIS2_PLACEMENT_3D('',#48902,#36051,#36052);
#29541=AXIS2_PLACEMENT_3D('',#48904,#36053,#36054);
#29542=AXIS2_PLACEMENT_3D('',#48905,#36055,#36056);
#29543=AXIS2_PLACEMENT_3D('',#49010,#36057,#36058);
#29544=AXIS2_PLACEMENT_3D('',#49011,#36059,#36060);
#29545=AXIS2_PLACEMENT_3D('',#49662,#36061,#36062);
#29546=AXIS2_PLACEMENT_3D('',#49686,#36064,#36065);
#29547=AXIS2_PLACEMENT_3D('',#49694,#36066,#36067);
#29548=AXIS2_PLACEMENT_3D('',#49700,#36071,#36072);
#29549=AXIS2_PLACEMENT_3D('',#49704,#36075,#36076);
#29550=AXIS2_PLACEMENT_3D('',#49708,#36079,#36080);
#29551=AXIS2_PLACEMENT_3D('',#49714,#36084,#36085);
#29552=AXIS2_PLACEMENT_3D('',#49715,#36086,#36087);
#29553=AXIS2_PLACEMENT_3D('',#49717,#36089,#36090);
#29554=AXIS2_PLACEMENT_3D('',#49719,#36092,#36093);
#29555=AXIS2_PLACEMENT_3D('',#49720,#36094,#36095);
#29556=AXIS2_PLACEMENT_3D('',#49721,#36096,#36097);
#29557=AXIS2_PLACEMENT_3D('',#49723,#36098,#36099);
#29558=AXIS2_PLACEMENT_3D('',#49724,#36100,#36101);
#29559=AXIS2_PLACEMENT_3D('',#49726,#36103,#36104);
#29560=AXIS2_PLACEMENT_3D('',#49727,#36105,#36106);
#29561=AXIS2_PLACEMENT_3D('',#49728,#36107,#36108);
#29562=AXIS2_PLACEMENT_3D('',#49744,#36110,#36111);
#29563=AXIS2_PLACEMENT_3D('',#49755,#36112,#36113);
#29564=AXIS2_PLACEMENT_3D('',#49803,#36115,#36116);
#29565=AXIS2_PLACEMENT_3D('',#49851,#36118,#36119);
#29566=AXIS2_PLACEMENT_3D('',#49899,#36121,#36122);
#29567=AXIS2_PLACEMENT_3D('',#49953,#36124,#36125);
#29568=AXIS2_PLACEMENT_3D('',#50001,#36127,#36128);
#29569=AXIS2_PLACEMENT_3D('',#50049,#36130,#36131);
#29570=AXIS2_PLACEMENT_3D('',#50103,#36133,#36134);
#29571=AXIS2_PLACEMENT_3D('',#50151,#36136,#36137);
#29572=AXIS2_PLACEMENT_3D('',#50199,#36139,#36140);
#29573=AXIS2_PLACEMENT_3D('',#50247,#36142,#36143);
#29574=AXIS2_PLACEMENT_3D('',#50301,#36145,#36146);
#29575=AXIS2_PLACEMENT_3D('',#50349,#36148,#36149);
#29576=AXIS2_PLACEMENT_3D('',#50397,#36151,#36152);
#29577=AXIS2_PLACEMENT_3D('',#50451,#36154,#36155);
#29578=AXIS2_PLACEMENT_3D('',#50499,#36157,#36158);
#29579=AXIS2_PLACEMENT_3D('',#50547,#36160,#36161);
#29580=AXIS2_PLACEMENT_3D('',#50595,#36163,#36164);
#29581=AXIS2_PLACEMENT_3D('',#50649,#36166,#36167);
#29582=AXIS2_PLACEMENT_3D('',#50697,#36169,#36170);
#29583=AXIS2_PLACEMENT_3D('',#50706,#36172,#36173);
#29584=AXIS2_PLACEMENT_3D('',#50707,#36174,#36175);
#29585=AXIS2_PLACEMENT_3D('',#50722,#36177,#36178);
#29586=AXIS2_PLACEMENT_3D('',#50733,#36179,#36180);
#29587=AXIS2_PLACEMENT_3D('',#50758,#36182,#36183);
#29588=AXIS2_PLACEMENT_3D('',#50783,#36185,#36186);
#29589=AXIS2_PLACEMENT_3D('',#50807,#36188,#36189);
#29590=AXIS2_PLACEMENT_3D('',#50831,#36191,#36192);
#29591=AXIS2_PLACEMENT_3D('',#50856,#36194,#36195);
#29592=AXIS2_PLACEMENT_3D('',#50881,#36197,#36198);
#29593=AXIS2_PLACEMENT_3D('',#50905,#36200,#36201);
#29594=AXIS2_PLACEMENT_3D('',#50930,#36203,#36204);
#29595=AXIS2_PLACEMENT_3D('',#50955,#36206,#36207);
#29596=AXIS2_PLACEMENT_3D('',#50979,#36209,#36210);
#29597=AXIS2_PLACEMENT_3D('',#51003,#36212,#36213);
#29598=AXIS2_PLACEMENT_3D('',#51028,#36215,#36216);
#29599=AXIS2_PLACEMENT_3D('',#51053,#36218,#36219);
#29600=AXIS2_PLACEMENT_3D('',#51077,#36221,#36222);
#29601=AXIS2_PLACEMENT_3D('',#51102,#36224,#36225);
#29602=AXIS2_PLACEMENT_3D('',#51127,#36227,#36228);
#29603=AXIS2_PLACEMENT_3D('',#51151,#36230,#36231);
#29604=AXIS2_PLACEMENT_3D('',#51929,#36233,#36234);
#29605=AXIS2_PLACEMENT_3D('',#51931,#36235,#36236);
#29606=AXIS2_PLACEMENT_3D('',#51932,#36237,#36238);
#29607=AXIS2_PLACEMENT_3D('',#52037,#36239,#36240);
#29608=AXIS2_PLACEMENT_3D('',#52038,#36241,#36242);
#29609=AXIS2_PLACEMENT_3D('',#52689,#36243,#36244);
#29610=AXIS2_PLACEMENT_3D('',#52698,#36249,#36250);
#29611=AXIS2_PLACEMENT_3D('',#52700,#36251,#36252);
#29612=AXIS2_PLACEMENT_3D('',#52702,#36254,#36255);
#29613=AXIS2_PLACEMENT_3D('',#52706,#36258,#36259);
#29614=AXIS2_PLACEMENT_3D('',#52707,#36260,#36261);
#29615=AXIS2_PLACEMENT_3D('',#52708,#36262,#36263);
#29616=AXIS2_PLACEMENT_3D('',#52717,#36268,#36269);
#29617=AXIS2_PLACEMENT_3D('',#52719,#36270,#36271);
#29618=AXIS2_PLACEMENT_3D('',#52721,#36273,#36274);
#29619=AXIS2_PLACEMENT_3D('',#52725,#36277,#36278);
#29620=AXIS2_PLACEMENT_3D('',#52726,#36279,#36280);
#29621=AXIS2_PLACEMENT_3D('',#52727,#36281,#36282);
#29622=AXIS2_PLACEMENT_3D('',#52736,#36287,#36288);
#29623=AXIS2_PLACEMENT_3D('',#52738,#36289,#36290);
#29624=AXIS2_PLACEMENT_3D('',#52740,#36292,#36293);
#29625=AXIS2_PLACEMENT_3D('',#52744,#36296,#36297);
#29626=AXIS2_PLACEMENT_3D('',#52745,#36298,#36299);
#29627=AXIS2_PLACEMENT_3D('',#52746,#36300,#36301);
#29628=AXIS2_PLACEMENT_3D('',#52755,#36306,#36307);
#29629=AXIS2_PLACEMENT_3D('',#52757,#36308,#36309);
#29630=AXIS2_PLACEMENT_3D('',#52759,#36311,#36312);
#29631=AXIS2_PLACEMENT_3D('',#52763,#36315,#36316);
#29632=AXIS2_PLACEMENT_3D('',#52764,#36317,#36318);
#29633=AXIS2_PLACEMENT_3D('',#52765,#36319,#36320);
#29634=AXIS2_PLACEMENT_3D('',#52774,#36325,#36326);
#29635=AXIS2_PLACEMENT_3D('',#52776,#36327,#36328);
#29636=AXIS2_PLACEMENT_3D('',#52778,#36330,#36331);
#29637=AXIS2_PLACEMENT_3D('',#52782,#36334,#36335);
#29638=AXIS2_PLACEMENT_3D('',#52783,#36336,#36337);
#29639=AXIS2_PLACEMENT_3D('',#52784,#36338,#36339);
#29640=AXIS2_PLACEMENT_3D('',#52793,#36344,#36345);
#29641=AXIS2_PLACEMENT_3D('',#52795,#36346,#36347);
#29642=AXIS2_PLACEMENT_3D('',#52797,#36349,#36350);
#29643=AXIS2_PLACEMENT_3D('',#52801,#36353,#36354);
#29644=AXIS2_PLACEMENT_3D('',#52802,#36355,#36356);
#29645=AXIS2_PLACEMENT_3D('',#52803,#36357,#36358);
#29646=AXIS2_PLACEMENT_3D('',#52812,#36363,#36364);
#29647=AXIS2_PLACEMENT_3D('',#52814,#36365,#36366);
#29648=AXIS2_PLACEMENT_3D('',#52816,#36368,#36369);
#29649=AXIS2_PLACEMENT_3D('',#52820,#36372,#36373);
#29650=AXIS2_PLACEMENT_3D('',#52821,#36374,#36375);
#29651=AXIS2_PLACEMENT_3D('',#52822,#36376,#36377);
#29652=AXIS2_PLACEMENT_3D('',#52831,#36382,#36383);
#29653=AXIS2_PLACEMENT_3D('',#52833,#36384,#36385);
#29654=AXIS2_PLACEMENT_3D('',#52835,#36387,#36388);
#29655=AXIS2_PLACEMENT_3D('',#52839,#36391,#36392);
#29656=AXIS2_PLACEMENT_3D('',#52840,#36393,#36394);
#29657=AXIS2_PLACEMENT_3D('',#52841,#36395,#36396);
#29658=AXIS2_PLACEMENT_3D('',#52850,#36401,#36402);
#29659=AXIS2_PLACEMENT_3D('',#52852,#36403,#36404);
#29660=AXIS2_PLACEMENT_3D('',#52854,#36406,#36407);
#29661=AXIS2_PLACEMENT_3D('',#52858,#36410,#36411);
#29662=AXIS2_PLACEMENT_3D('',#52859,#36412,#36413);
#29663=AXIS2_PLACEMENT_3D('',#52860,#36414,#36415);
#29664=AXIS2_PLACEMENT_3D('',#52869,#36420,#36421);
#29665=AXIS2_PLACEMENT_3D('',#52871,#36422,#36423);
#29666=AXIS2_PLACEMENT_3D('',#52873,#36425,#36426);
#29667=AXIS2_PLACEMENT_3D('',#52877,#36429,#36430);
#29668=AXIS2_PLACEMENT_3D('',#52878,#36431,#36432);
#29669=AXIS2_PLACEMENT_3D('',#52879,#36433,#36434);
#29670=AXIS2_PLACEMENT_3D('',#52888,#36439,#36440);
#29671=AXIS2_PLACEMENT_3D('',#52890,#36441,#36442);
#29672=AXIS2_PLACEMENT_3D('',#52892,#36444,#36445);
#29673=AXIS2_PLACEMENT_3D('',#52896,#36448,#36449);
#29674=AXIS2_PLACEMENT_3D('',#52897,#36450,#36451);
#29675=AXIS2_PLACEMENT_3D('',#52898,#36452,#36453);
#29676=AXIS2_PLACEMENT_3D('',#52907,#36458,#36459);
#29677=AXIS2_PLACEMENT_3D('',#52909,#36460,#36461);
#29678=AXIS2_PLACEMENT_3D('',#52911,#36463,#36464);
#29679=AXIS2_PLACEMENT_3D('',#52915,#36467,#36468);
#29680=AXIS2_PLACEMENT_3D('',#52916,#36469,#36470);
#29681=AXIS2_PLACEMENT_3D('',#52917,#36471,#36472);
#29682=AXIS2_PLACEMENT_3D('',#52926,#36477,#36478);
#29683=AXIS2_PLACEMENT_3D('',#52928,#36479,#36480);
#29684=AXIS2_PLACEMENT_3D('',#52930,#36482,#36483);
#29685=AXIS2_PLACEMENT_3D('',#52934,#36486,#36487);
#29686=AXIS2_PLACEMENT_3D('',#52935,#36488,#36489);
#29687=AXIS2_PLACEMENT_3D('',#52936,#36490,#36491);
#29688=AXIS2_PLACEMENT_3D('',#52945,#36496,#36497);
#29689=AXIS2_PLACEMENT_3D('',#52947,#36498,#36499);
#29690=AXIS2_PLACEMENT_3D('',#52949,#36501,#36502);
#29691=AXIS2_PLACEMENT_3D('',#52953,#36505,#36506);
#29692=AXIS2_PLACEMENT_3D('',#52954,#36507,#36508);
#29693=AXIS2_PLACEMENT_3D('',#52955,#36509,#36510);
#29694=AXIS2_PLACEMENT_3D('',#52964,#36515,#36516);
#29695=AXIS2_PLACEMENT_3D('',#52966,#36517,#36518);
#29696=AXIS2_PLACEMENT_3D('',#52968,#36520,#36521);
#29697=AXIS2_PLACEMENT_3D('',#52972,#36524,#36525);
#29698=AXIS2_PLACEMENT_3D('',#52973,#36526,#36527);
#29699=AXIS2_PLACEMENT_3D('',#52974,#36528,#36529);
#29700=AXIS2_PLACEMENT_3D('',#52983,#36534,#36535);
#29701=AXIS2_PLACEMENT_3D('',#52985,#36536,#36537);
#29702=AXIS2_PLACEMENT_3D('',#52987,#36539,#36540);
#29703=AXIS2_PLACEMENT_3D('',#52991,#36543,#36544);
#29704=AXIS2_PLACEMENT_3D('',#52992,#36545,#36546);
#29705=AXIS2_PLACEMENT_3D('',#52993,#36547,#36548);
#29706=AXIS2_PLACEMENT_3D('',#53002,#36553,#36554);
#29707=AXIS2_PLACEMENT_3D('',#53004,#36555,#36556);
#29708=AXIS2_PLACEMENT_3D('',#53006,#36558,#36559);
#29709=AXIS2_PLACEMENT_3D('',#53010,#36562,#36563);
#29710=AXIS2_PLACEMENT_3D('',#53011,#36564,#36565);
#29711=AXIS2_PLACEMENT_3D('',#53012,#36566,#36567);
#29712=AXIS2_PLACEMENT_3D('',#53021,#36572,#36573);
#29713=AXIS2_PLACEMENT_3D('',#53023,#36574,#36575);
#29714=AXIS2_PLACEMENT_3D('',#53026,#36577,#36578);
#29715=AXIS2_PLACEMENT_3D('',#53027,#36579,#36580);
#29716=AXIS2_PLACEMENT_3D('',#53031,#36583,#36584);
#29717=AXIS2_PLACEMENT_3D('',#53033,#36585,#36586);
#29718=AXIS2_PLACEMENT_3D('',#53034,#36587,#36588);
#29719=AXIS2_PLACEMENT_3D('',#53035,#36589,#36590);
#29720=AXIS2_PLACEMENT_3D('',#53044,#36595,#36596);
#29721=AXIS2_PLACEMENT_3D('',#53046,#36597,#36598);
#29722=AXIS2_PLACEMENT_3D('',#53048,#36600,#36601);
#29723=AXIS2_PLACEMENT_3D('',#53052,#36604,#36605);
#29724=AXIS2_PLACEMENT_3D('',#53053,#36606,#36607);
#29725=AXIS2_PLACEMENT_3D('',#53054,#36608,#36609);
#29726=AXIS2_PLACEMENT_3D('',#53063,#36614,#36615);
#29727=AXIS2_PLACEMENT_3D('',#53065,#36616,#36617);
#29728=AXIS2_PLACEMENT_3D('',#53067,#36619,#36620);
#29729=AXIS2_PLACEMENT_3D('',#53071,#36623,#36624);
#29730=AXIS2_PLACEMENT_3D('',#53072,#36625,#36626);
#29731=AXIS2_PLACEMENT_3D('',#53073,#36627,#36628);
#29732=AXIS2_PLACEMENT_3D('',#53082,#36633,#36634);
#29733=AXIS2_PLACEMENT_3D('',#53084,#36635,#36636);
#29734=AXIS2_PLACEMENT_3D('',#53086,#36638,#36639);
#29735=AXIS2_PLACEMENT_3D('',#53090,#36642,#36643);
#29736=AXIS2_PLACEMENT_3D('',#53091,#36644,#36645);
#29737=AXIS2_PLACEMENT_3D('',#53092,#36646,#36647);
#29738=AXIS2_PLACEMENT_3D('',#53101,#36652,#36653);
#29739=AXIS2_PLACEMENT_3D('',#53103,#36654,#36655);
#29740=AXIS2_PLACEMENT_3D('',#53105,#36657,#36658);
#29741=AXIS2_PLACEMENT_3D('',#53109,#36661,#36662);
#29742=AXIS2_PLACEMENT_3D('',#53110,#36663,#36664);
#29743=AXIS2_PLACEMENT_3D('',#53111,#36665,#36666);
#29744=AXIS2_PLACEMENT_3D('',#53120,#36671,#36672);
#29745=AXIS2_PLACEMENT_3D('',#53122,#36673,#36674);
#29746=AXIS2_PLACEMENT_3D('',#53124,#36676,#36677);
#29747=AXIS2_PLACEMENT_3D('',#53128,#36680,#36681);
#29748=AXIS2_PLACEMENT_3D('',#53129,#36682,#36683);
#29749=AXIS2_PLACEMENT_3D('',#53130,#36684,#36685);
#29750=AXIS2_PLACEMENT_3D('',#53139,#36690,#36691);
#29751=AXIS2_PLACEMENT_3D('',#53141,#36692,#36693);
#29752=AXIS2_PLACEMENT_3D('',#53143,#36695,#36696);
#29753=AXIS2_PLACEMENT_3D('',#53147,#36699,#36700);
#29754=AXIS2_PLACEMENT_3D('',#53148,#36701,#36702);
#29755=AXIS2_PLACEMENT_3D('',#53149,#36703,#36704);
#29756=AXIS2_PLACEMENT_3D('',#53158,#36709,#36710);
#29757=AXIS2_PLACEMENT_3D('',#53160,#36711,#36712);
#29758=AXIS2_PLACEMENT_3D('',#53162,#36714,#36715);
#29759=AXIS2_PLACEMENT_3D('',#53166,#36718,#36719);
#29760=AXIS2_PLACEMENT_3D('',#53167,#36720,#36721);
#29761=AXIS2_PLACEMENT_3D('',#53168,#36722,#36723);
#29762=AXIS2_PLACEMENT_3D('',#53177,#36728,#36729);
#29763=AXIS2_PLACEMENT_3D('',#53179,#36730,#36731);
#29764=AXIS2_PLACEMENT_3D('',#53181,#36733,#36734);
#29765=AXIS2_PLACEMENT_3D('',#53185,#36737,#36738);
#29766=AXIS2_PLACEMENT_3D('',#53186,#36739,#36740);
#29767=AXIS2_PLACEMENT_3D('',#53187,#36741,#36742);
#29768=AXIS2_PLACEMENT_3D('',#53196,#36747,#36748);
#29769=AXIS2_PLACEMENT_3D('',#53198,#36749,#36750);
#29770=AXIS2_PLACEMENT_3D('',#53200,#36752,#36753);
#29771=AXIS2_PLACEMENT_3D('',#53204,#36756,#36757);
#29772=AXIS2_PLACEMENT_3D('',#53205,#36758,#36759);
#29773=AXIS2_PLACEMENT_3D('',#53206,#36760,#36761);
#29774=AXIS2_PLACEMENT_3D('',#53215,#36766,#36767);
#29775=AXIS2_PLACEMENT_3D('',#53217,#36768,#36769);
#29776=AXIS2_PLACEMENT_3D('',#53219,#36771,#36772);
#29777=AXIS2_PLACEMENT_3D('',#53223,#36775,#36776);
#29778=AXIS2_PLACEMENT_3D('',#53224,#36777,#36778);
#29779=AXIS2_PLACEMENT_3D('',#53225,#36779,#36780);
#29780=AXIS2_PLACEMENT_3D('',#53234,#36785,#36786);
#29781=AXIS2_PLACEMENT_3D('',#53236,#36787,#36788);
#29782=AXIS2_PLACEMENT_3D('',#53238,#36790,#36791);
#29783=AXIS2_PLACEMENT_3D('',#53242,#36794,#36795);
#29784=AXIS2_PLACEMENT_3D('',#53243,#36796,#36797);
#29785=AXIS2_PLACEMENT_3D('',#53244,#36798,#36799);
#29786=AXIS2_PLACEMENT_3D('',#53253,#36804,#36805);
#29787=AXIS2_PLACEMENT_3D('',#53255,#36806,#36807);
#29788=AXIS2_PLACEMENT_3D('',#53257,#36809,#36810);
#29789=AXIS2_PLACEMENT_3D('',#53261,#36813,#36814);
#29790=AXIS2_PLACEMENT_3D('',#53262,#36815,#36816);
#29791=AXIS2_PLACEMENT_3D('',#53263,#36817,#36818);
#29792=AXIS2_PLACEMENT_3D('',#53272,#36823,#36824);
#29793=AXIS2_PLACEMENT_3D('',#53274,#36825,#36826);
#29794=AXIS2_PLACEMENT_3D('',#53276,#36828,#36829);
#29795=AXIS2_PLACEMENT_3D('',#53280,#36832,#36833);
#29796=AXIS2_PLACEMENT_3D('',#53281,#36834,#36835);
#29797=AXIS2_PLACEMENT_3D('',#53282,#36836,#36837);
#29798=AXIS2_PLACEMENT_3D('',#53291,#36842,#36843);
#29799=AXIS2_PLACEMENT_3D('',#53293,#36844,#36845);
#29800=AXIS2_PLACEMENT_3D('',#53295,#36847,#36848);
#29801=AXIS2_PLACEMENT_3D('',#53299,#36851,#36852);
#29802=AXIS2_PLACEMENT_3D('',#53300,#36853,#36854);
#29803=AXIS2_PLACEMENT_3D('',#53301,#36855,#36856);
#29804=AXIS2_PLACEMENT_3D('',#53310,#36861,#36862);
#29805=AXIS2_PLACEMENT_3D('',#53312,#36863,#36864);
#29806=AXIS2_PLACEMENT_3D('',#53314,#36866,#36867);
#29807=AXIS2_PLACEMENT_3D('',#53318,#36870,#36871);
#29808=AXIS2_PLACEMENT_3D('',#53319,#36872,#36873);
#29809=AXIS2_PLACEMENT_3D('',#53320,#36874,#36875);
#29810=AXIS2_PLACEMENT_3D('',#53329,#36880,#36881);
#29811=AXIS2_PLACEMENT_3D('',#53331,#36882,#36883);
#29812=AXIS2_PLACEMENT_3D('',#53333,#36885,#36886);
#29813=AXIS2_PLACEMENT_3D('',#53337,#36889,#36890);
#29814=AXIS2_PLACEMENT_3D('',#53338,#36891,#36892);
#29815=AXIS2_PLACEMENT_3D('',#53339,#36893,#36894);
#29816=AXIS2_PLACEMENT_3D('',#53348,#36899,#36900);
#29817=AXIS2_PLACEMENT_3D('',#53350,#36901,#36902);
#29818=AXIS2_PLACEMENT_3D('',#53352,#36904,#36905);
#29819=AXIS2_PLACEMENT_3D('',#53356,#36908,#36909);
#29820=AXIS2_PLACEMENT_3D('',#53357,#36910,#36911);
#29821=AXIS2_PLACEMENT_3D('',#53358,#36912,#36913);
#29822=AXIS2_PLACEMENT_3D('',#53367,#36918,#36919);
#29823=AXIS2_PLACEMENT_3D('',#53369,#36920,#36921);
#29824=AXIS2_PLACEMENT_3D('',#53371,#36923,#36924);
#29825=AXIS2_PLACEMENT_3D('',#53375,#36927,#36928);
#29826=AXIS2_PLACEMENT_3D('',#53376,#36929,#36930);
#29827=AXIS2_PLACEMENT_3D('',#53377,#36931,#36932);
#29828=AXIS2_PLACEMENT_3D('',#53386,#36937,#36938);
#29829=AXIS2_PLACEMENT_3D('',#53392,#36942,#36943);
#29830=AXIS2_PLACEMENT_3D('',#53398,#36947,#36948);
#29831=AXIS2_PLACEMENT_3D('',#53404,#36952,#36953);
#29832=AXIS2_PLACEMENT_3D('',#53410,#36957,#36958);
#29833=AXIS2_PLACEMENT_3D('',#53413,#36961,#36962);
#29834=AXIS2_PLACEMENT_3D('',#53414,#36963,#36964);
#29835=AXIS2_PLACEMENT_3D('',#53416,#36965,#36966);
#29836=AXIS2_PLACEMENT_3D('',#53417,#36967,#36968);
#29837=AXIS2_PLACEMENT_3D('',#53419,#36970,#36971);
#29838=AXIS2_PLACEMENT_3D('',#53420,#36972,#36973);
#29839=AXIS2_PLACEMENT_3D('',#53421,#36974,#36975);
#29840=AXIS2_PLACEMENT_3D('',#53423,#36976,#36977);
#29841=AXIS2_PLACEMENT_3D('',#53424,#36978,#36979);
#29842=AXIS2_PLACEMENT_3D('',#53426,#36980,#36981);
#29843=AXIS2_PLACEMENT_3D('',#53429,#36984,#36985);
#29844=AXIS2_PLACEMENT_3D('',#53431,#36986,#36987);
#29845=AXIS2_PLACEMENT_3D('',#53433,#36989,#36990);
#29846=AXIS2_PLACEMENT_3D('',#53434,#36991,#36992);
#29847=AXIS2_PLACEMENT_3D('',#53435,#36993,#36994);
#29848=AXIS2_PLACEMENT_3D('',#53442,#36998,#36999);
#29849=AXIS2_PLACEMENT_3D('',#53448,#37003,#37004);
#29850=AXIS2_PLACEMENT_3D('',#53455,#37008,#37009);
#29851=AXIS2_PLACEMENT_3D('',#53461,#37013,#37014);
#29852=AXIS2_PLACEMENT_3D('',#53464,#37017,#37018);
#29853=AXIS2_PLACEMENT_3D('',#53471,#37022,#37023);
#29854=AXIS2_PLACEMENT_3D('',#53477,#37027,#37028);
#29855=AXIS2_PLACEMENT_3D('',#53484,#37032,#37033);
#29856=AXIS2_PLACEMENT_3D('',#53490,#37037,#37038);
#29857=AXIS2_PLACEMENT_3D('',#53493,#37041,#37042);
#29858=AXIS2_PLACEMENT_3D('',#53500,#37046,#37047);
#29859=AXIS2_PLACEMENT_3D('',#53506,#37051,#37052);
#29860=AXIS2_PLACEMENT_3D('',#53513,#37056,#37057);
#29861=AXIS2_PLACEMENT_3D('',#53519,#37061,#37062);
#29862=AXIS2_PLACEMENT_3D('',#53522,#37065,#37066);
#29863=AXIS2_PLACEMENT_3D('',#53525,#37069,#37070);
#29864=AXIS2_PLACEMENT_3D('',#53528,#37073,#37074);
#29865=AXIS2_PLACEMENT_3D('',#53531,#37077,#37078);
#29866=AXIS2_PLACEMENT_3D('',#53533,#37080,#37081);
#29867=AXIS2_PLACEMENT_3D('',#53535,#37083,#37084);
#29868=AXIS2_PLACEMENT_3D('',#53537,#37086,#37087);
#29869=AXIS2_PLACEMENT_3D('',#53550,#37094,#37095);
#29870=AXIS2_PLACEMENT_3D('',#53556,#37099,#37100);
#29871=AXIS2_PLACEMENT_3D('',#53560,#37103,#37104);
#29872=AXIS2_PLACEMENT_3D('',#53566,#37108,#37109);
#29873=AXIS2_PLACEMENT_3D('',#53570,#37112,#37113);
#29874=AXIS2_PLACEMENT_3D('',#53572,#37115,#37116);
#29875=AXIS2_PLACEMENT_3D('',#53574,#37118,#37119);
#29876=AXIS2_PLACEMENT_3D('',#53580,#37123,#37124);
#29877=AXIS2_PLACEMENT_3D('',#53584,#37127,#37128);
#29878=AXIS2_PLACEMENT_3D('',#53588,#37131,#37132);
#29879=AXIS2_PLACEMENT_3D('',#53592,#37135,#37136);
#29880=AXIS2_PLACEMENT_3D('',#53596,#37139,#37140);
#29881=AXIS2_PLACEMENT_3D('',#53598,#37142,#37143);
#29882=AXIS2_PLACEMENT_3D('',#53599,#37144,#37145);
#29883=AXIS2_PLACEMENT_3D('',#53604,#37149,#37150);
#29884=AXIS2_PLACEMENT_3D('',#53605,#37151,#37152);
#29885=AXIS2_PLACEMENT_3D('',#53606,#37153,#37154);
#29886=AXIS2_PLACEMENT_3D('',#53607,#37155,#37156);
#29887=AXIS2_PLACEMENT_3D('',#53608,#37157,#37158);
#29888=AXIS2_PLACEMENT_3D('',#53610,#37159,#37160);
#29889=AXIS2_PLACEMENT_3D('',#53611,#37161,#37162);
#29890=AXIS2_PLACEMENT_3D('',#53613,#37163,#37164);
#29891=AXIS2_PLACEMENT_3D('',#53615,#37166,#37167);
#29892=AXIS2_PLACEMENT_3D('',#53617,#37169,#37170);
#29893=AXIS2_PLACEMENT_3D('',#53618,#37171,#37172);
#29894=AXIS2_PLACEMENT_3D('',#53634,#37174,#37175);
#29895=AXIS2_PLACEMENT_3D('',#53642,#37176,#37177);
#29896=AXIS2_PLACEMENT_3D('',#53690,#37179,#37180);
#29897=AXIS2_PLACEMENT_3D('',#53738,#37182,#37183);
#29898=AXIS2_PLACEMENT_3D('',#53792,#37185,#37186);
#29899=AXIS2_PLACEMENT_3D('',#53840,#37188,#37189);
#29900=AXIS2_PLACEMENT_3D('',#53888,#37191,#37192);
#29901=AXIS2_PLACEMENT_3D('',#53936,#37194,#37195);
#29902=AXIS2_PLACEMENT_3D('',#53990,#37197,#37198);
#29903=AXIS2_PLACEMENT_3D('',#54038,#37200,#37201);
#29904=AXIS2_PLACEMENT_3D('',#54086,#37203,#37204);
#29905=AXIS2_PLACEMENT_3D('',#54140,#37206,#37207);
#29906=AXIS2_PLACEMENT_3D('',#54188,#37209,#37210);
#29907=AXIS2_PLACEMENT_3D('',#54193,#37212,#37213);
#29908=AXIS2_PLACEMENT_3D('',#54235,#37214,#37215);
#29909=AXIS2_PLACEMENT_3D('',#54248,#37217,#37218);
#29910=AXIS2_PLACEMENT_3D('',#54255,#37219,#37220);
#29911=AXIS2_PLACEMENT_3D('',#54279,#37222,#37223);
#29912=AXIS2_PLACEMENT_3D('',#54304,#37225,#37226);
#29913=AXIS2_PLACEMENT_3D('',#54329,#37228,#37229);
#29914=AXIS2_PLACEMENT_3D('',#54353,#37231,#37232);
#29915=AXIS2_PLACEMENT_3D('',#54378,#37234,#37235);
#29916=AXIS2_PLACEMENT_3D('',#54403,#37237,#37238);
#29917=AXIS2_PLACEMENT_3D('',#54427,#37240,#37241);
#29918=AXIS2_PLACEMENT_3D('',#54451,#37243,#37244);
#29919=AXIS2_PLACEMENT_3D('',#54476,#37246,#37247);
#29920=AXIS2_PLACEMENT_3D('',#54501,#37249,#37250);
#29921=AXIS2_PLACEMENT_3D('',#55038,#37252,#37253);
#29922=AXIS2_PLACEMENT_3D('',#55040,#37254,#37255);
#29923=AXIS2_PLACEMENT_3D('',#55041,#37256,#37257);
#29924=AXIS2_PLACEMENT_3D('',#55128,#37258,#37259);
#29925=AXIS2_PLACEMENT_3D('',#55129,#37260,#37261);
#29926=AXIS2_PLACEMENT_3D('',#55551,#37262,#37263);
#29927=AXIS2_PLACEMENT_3D('',#55565,#37267,#37268);
#29928=AXIS2_PLACEMENT_3D('',#55576,#37271,#37272);
#29929=AXIS2_PLACEMENT_3D('',#55587,#37275,#37276);
#29930=AXIS2_PLACEMENT_3D('',#55598,#37279,#37280);
#29931=AXIS2_PLACEMENT_3D('',#55609,#37283,#37284);
#29932=AXIS2_PLACEMENT_3D('',#55617,#37286,#37287);
#29933=AXIS2_PLACEMENT_3D('',#55618,#37288,#37289);
#29934=AXIS2_PLACEMENT_3D('',#55620,#37290,#37291);
#29935=AXIS2_PLACEMENT_3D('',#55621,#37292,#37293);
#29936=AXIS2_PLACEMENT_3D('',#55623,#37295,#37296);
#29937=AXIS2_PLACEMENT_3D('',#55624,#37297,#37298);
#29938=AXIS2_PLACEMENT_3D('',#55625,#37299,#37300);
#29939=AXIS2_PLACEMENT_3D('',#55627,#37301,#37302);
#29940=AXIS2_PLACEMENT_3D('',#55658,#37303,#37304);
#29941=AXIS2_PLACEMENT_3D('',#55659,#37305,#37306);
#29942=AXIS2_PLACEMENT_3D('',#55660,#37307,#37308);
#29943=AXIS2_PLACEMENT_3D('',#55661,#37309,#37310);
#29944=AXIS2_PLACEMENT_3D('',#55662,#37311,#37312);
#29945=AXIS2_PLACEMENT_3D('',#55663,#37313,#37314);
#29946=AXIS2_PLACEMENT_3D('',#55664,#37315,#37316);
#29947=AXIS2_PLACEMENT_3D('',#55665,#37317,#37318);
#29948=AXIS2_PLACEMENT_3D('',#55666,#37319,#37320);
#29949=AXIS2_PLACEMENT_3D('',#55667,#37321,#37322);
#29950=AXIS2_PLACEMENT_3D('',#55668,#37323,#37324);
#29951=AXIS2_PLACEMENT_3D('',#55669,#37325,#37326);
#29952=AXIS2_PLACEMENT_3D('',#55670,#37327,#37328);
#29953=AXIS2_PLACEMENT_3D('',#55671,#37329,#37330);
#29954=AXIS2_PLACEMENT_3D('',#55672,#37331,#37332);
#29955=AXIS2_PLACEMENT_3D('',#55673,#37333,#37334);
#29956=AXIS2_PLACEMENT_3D('',#55674,#37335,#37336);
#29957=AXIS2_PLACEMENT_3D('',#55675,#37337,#37338);
#29958=AXIS2_PLACEMENT_3D('',#55676,#37339,#37340);
#29959=AXIS2_PLACEMENT_3D('',#55677,#37341,#37342);
#29960=AXIS2_PLACEMENT_3D('',#55678,#37343,#37344);
#29961=AXIS2_PLACEMENT_3D('',#55679,#37345,#37346);
#29962=AXIS2_PLACEMENT_3D('',#55680,#37347,#37348);
#29963=AXIS2_PLACEMENT_3D('',#55681,#37349,#37350);
#29964=AXIS2_PLACEMENT_3D('',#55682,#37351,#37352);
#29965=AXIS2_PLACEMENT_3D('',#55683,#37353,#37354);
#29966=AXIS2_PLACEMENT_3D('',#55684,#37355,#37356);
#29967=AXIS2_PLACEMENT_3D('',#55685,#37357,#37358);
#29968=AXIS2_PLACEMENT_3D('',#55686,#37359,#37360);
#29969=AXIS2_PLACEMENT_3D('',#55687,#37361,#37362);
#29970=AXIS2_PLACEMENT_3D('',#55688,#37363,#37364);
#29971=AXIS2_PLACEMENT_3D('',#55689,#37365,#37366);
#29972=AXIS2_PLACEMENT_3D('',#55690,#37367,#37368);
#29973=AXIS2_PLACEMENT_3D('',#55691,#37369,#37370);
#29974=AXIS2_PLACEMENT_3D('',#55692,#37371,#37372);
#29975=AXIS2_PLACEMENT_3D('',#55693,#37373,#37374);
#29976=DIRECTION('axis',(0.,0.,1.));
#29977=DIRECTION('refdir',(1.,0.,0.));
#29978=DIRECTION('axis',(0.,0.,1.));
#29979=DIRECTION('refdir',(1.,0.,0.));
#29980=DIRECTION('center_axis',(0.,-1.,0.));
#29981=DIRECTION('ref_axis',(0.,0.,1.));
#29982=DIRECTION('center_axis',(0.,1.,0.));
#29983=DIRECTION('ref_axis',(0.,0.,1.));
#29984=DIRECTION('center_axis',(1.,0.,-1.22464679914735E-16));
#29985=DIRECTION('ref_axis',(-1.22464679914735E-16,0.,-1.));
#29986=DIRECTION('center_axis',(0.,-1.,0.));
#29987=DIRECTION('ref_axis',(0.,0.,1.));
#29988=DIRECTION('center_axis',(0.,1.,0.));
#29989=DIRECTION('ref_axis',(0.,0.,1.));
#29990=DIRECTION('center_axis',(0.,-1.,0.));
#29991=DIRECTION('ref_axis',(0.,0.,-1.));
#29992=DIRECTION('center_axis',(0.,1.,0.));
#29993=DIRECTION('ref_axis',(-0.013060400300148,0.,-0.999914709334751));
#29994=DIRECTION('',(0.,-1.,0.));
#29995=DIRECTION('center_axis',(0.,-1.,0.));
#29996=DIRECTION('ref_axis',(-0.468970569827389,0.,0.883213793277581));
#29997=DIRECTION('center_axis',(0.,-1.,0.));
#29998=DIRECTION('ref_axis',(-0.468970569827389,0.,0.883213793277581));
#29999=DIRECTION('',(0.,1.,0.));
#30000=DIRECTION('center_axis',(0.,1.,0.));
#30001=DIRECTION('ref_axis',(0.,0.,1.));
#30002=DIRECTION('',(0.,-1.,0.));
#30003=DIRECTION('center_axis',(0.,-1.,0.));
#30004=DIRECTION('ref_axis',(-0.468970569827389,0.,0.883213793277581));
#30005=DIRECTION('',(0.,1.,0.));
#30006=DIRECTION('center_axis',(0.,1.,0.));
#30007=DIRECTION('ref_axis',(0.,0.,1.));
#30008=DIRECTION('center_axis',(0.,-1.,0.));
#30009=DIRECTION('ref_axis',(1.,0.,0.));
#30010=DIRECTION('center_axis',(0.,-1.,0.));
#30011=DIRECTION('ref_axis',(1.,0.,0.));
#30012=DIRECTION('center_axis',(0.,-1.,0.));
#30013=DIRECTION('ref_axis',(1.,0.,0.));
#30014=DIRECTION('center_axis',(0.,-1.,0.));
#30015=DIRECTION('ref_axis',(1.,0.,0.));
#30016=DIRECTION('center_axis',(0.,-1.,0.));
#30017=DIRECTION('ref_axis',(0.,0.,1.));
#30018=DIRECTION('center_axis',(0.,1.,0.));
#30019=DIRECTION('ref_axis',(-0.468970569827389,0.,0.883213793277581));
#30020=DIRECTION('center_axis',(-0.883213793277581,0.,-0.468970569827389));
#30021=DIRECTION('ref_axis',(0.468970569827389,0.,-0.883213793277581));
#30022=DIRECTION('center_axis',(0.,1.,0.));
#30023=DIRECTION('ref_axis',(-0.468970569827389,0.,0.883213793277581));
#30024=DIRECTION('center_axis',(0.,-1.,0.));
#30025=DIRECTION('ref_axis',(0.,0.,1.));
#30026=DIRECTION('center_axis',(0.,-1.,0.));
#30027=DIRECTION('ref_axis',(0.,0.,1.));
#30028=DIRECTION('center_axis',(0.,-1.,0.));
#30029=DIRECTION('ref_axis',(0.,0.,-1.));
#30030=DIRECTION('center_axis',(0.,1.,0.));
#30031=DIRECTION('ref_axis',(1.,0.,0.));
#30032=DIRECTION('center_axis',(0.,1.,0.));
#30033=DIRECTION('ref_axis',(1.,0.,0.));
#30034=DIRECTION('center_axis',(0.,1.,0.));
#30035=DIRECTION('ref_axis',(1.,0.,0.));
#30036=DIRECTION('center_axis',(0.,1.,0.));
#30037=DIRECTION('ref_axis',(1.,0.,0.));
#30038=DIRECTION('center_axis',(0.,1.,0.));
#30039=DIRECTION('ref_axis',(1.,0.,0.));
#30040=DIRECTION('center_axis',(0.,1.,0.));
#30041=DIRECTION('ref_axis',(1.,0.,0.));
#30042=DIRECTION('center_axis',(0.,1.,0.));
#30043=DIRECTION('ref_axis',(1.,0.,0.));
#30044=DIRECTION('center_axis',(0.,1.,0.));
#30045=DIRECTION('ref_axis',(1.,0.,0.));
#30046=DIRECTION('center_axis',(0.,-1.,0.));
#30047=DIRECTION('ref_axis',(0.,0.,1.));
#30048=DIRECTION('center_axis',(0.,-1.,0.));
#30049=DIRECTION('ref_axis',(-0.707106781186551,0.,-0.707106781186544));
#30050=DIRECTION('center_axis',(0.,-1.,0.));
#30051=DIRECTION('ref_axis',(-1.,0.,0.));
#30052=DIRECTION('',(0.,-1.,0.));
#30053=DIRECTION('center_axis',(0.,1.,0.));
#30054=DIRECTION('ref_axis',(0.,0.,-1.));
#30055=DIRECTION('',(0.,1.,0.));
#30056=DIRECTION('center_axis',(-1.,4.44089209850062E-15,0.));
#30057=DIRECTION('ref_axis',(0.,0.,-1.));
#30058=DIRECTION('center_axis',(0.,0.,-1.));
#30059=DIRECTION('ref_axis',(-0.707106781186548,-0.707106781186548,0.));
#30060=DIRECTION('center_axis',(0.,0.,1.));
#30061=DIRECTION('ref_axis',(-0.707106781186548,-0.707106781186548,0.));
#30062=DIRECTION('center_axis',(1.,0.,0.));
#30063=DIRECTION('ref_axis',(0.,-0.707106781186549,-0.707106781186546));
#30064=DIRECTION('center_axis',(-1.,-4.44089209850062E-15,0.));
#30065=DIRECTION('ref_axis',(0.,0.,-1.));
#30066=DIRECTION('',(-1.,0.,0.));
#30067=DIRECTION('',(1.,0.,0.));
#30068=DIRECTION('center_axis',(-4.44089209850064E-15,-1.,0.));
#30069=DIRECTION('ref_axis',(0.,0.,-1.));
#30070=DIRECTION('center_axis',(0.,0.,-1.));
#30071=DIRECTION('ref_axis',(0.707106781186547,-0.707106781186548,0.));
#30072=DIRECTION('center_axis',(0.,0.,1.));
#30073=DIRECTION('ref_axis',(0.707106781186547,-0.707106781186548,0.));
#30074=DIRECTION('center_axis',(0.,1.,0.));
#30075=DIRECTION('ref_axis',(0.707106781186551,0.,-0.707106781186544));
#30076=DIRECTION('center_axis',(0.,-1.,0.));
#30077=DIRECTION('ref_axis',(0.,0.,-1.));
#30078=DIRECTION('',(0.,-1.,0.));
#30079=DIRECTION('',(0.,1.,0.));
#30080=DIRECTION('center_axis',(1.,-4.44089209850062E-15,0.));
#30081=DIRECTION('ref_axis',(0.,0.,-1.));
#30082=DIRECTION('center_axis',(0.,0.,-1.));
#30083=DIRECTION('ref_axis',(0.707106781186549,0.707106781186546,0.));
#30084=DIRECTION('center_axis',(0.,0.,1.));
#30085=DIRECTION('ref_axis',(0.707106781186549,0.707106781186546,0.));
#30086=DIRECTION('center_axis',(-1.,0.,0.));
#30087=DIRECTION('ref_axis',(0.,0.707106781186551,-0.707106781186544));
#30088=DIRECTION('center_axis',(1.,4.44089209850062E-15,0.));
#30089=DIRECTION('ref_axis',(0.,0.,-1.));
#30090=DIRECTION('',(1.,0.,0.));
#30091=DIRECTION('',(-1.,0.,0.));
#30092=DIRECTION('center_axis',(0.,0.,-1.));
#30093=DIRECTION('ref_axis',(-0.707106781186546,0.707106781186549,0.));
#30094=DIRECTION('center_axis',(0.,0.,1.));
#30095=DIRECTION('ref_axis',(-0.707106781186546,0.707106781186549,0.));
#30096=DIRECTION('center_axis',(0.,0.,1.));
#30097=DIRECTION('ref_axis',(1.,4.4408920985006E-15,0.));
#30098=DIRECTION('',(0.,0.,1.));
#30099=DIRECTION('center_axis',(0.,0.,1.));
#30100=DIRECTION('ref_axis',(0.707106781186549,0.707106781186546,0.));
#30101=DIRECTION('',(0.,0.,1.));
#30102=DIRECTION('center_axis',(0.,1.,0.));
#30103=DIRECTION('ref_axis',(-1.,0.,0.));
#30104=DIRECTION('',(0.,0.,1.));
#30105=DIRECTION('',(-1.,0.,0.));
#30106=DIRECTION('center_axis',(0.,0.,1.));
#30107=DIRECTION('ref_axis',(-4.4408920985006E-15,1.,0.));
#30108=DIRECTION('',(0.,0.,1.));
#30109=DIRECTION('center_axis',(0.,0.,1.));
#30110=DIRECTION('ref_axis',(-0.707106781186546,0.707106781186549,0.));
#30111=DIRECTION('center_axis',(-1.,0.,0.));
#30112=DIRECTION('ref_axis',(0.,-1.,0.));
#30113=DIRECTION('',(0.,0.,1.));
#30114=DIRECTION('',(0.,-1.,0.));
#30115=DIRECTION('center_axis',(0.,0.,1.));
#30116=DIRECTION('ref_axis',(1.,0.,0.));
#30117=DIRECTION('center_axis',(0.,0.,1.));
#30118=DIRECTION('ref_axis',(1.,0.,0.));
#30119=DIRECTION('center_axis',(0.,0.,1.));
#30120=DIRECTION('ref_axis',(1.,0.,0.));
#30121=DIRECTION('center_axis',(1.,0.,0.));
#30122=DIRECTION('ref_axis',(0.,-0.707106781186549,0.707106781186546));
#30123=DIRECTION('center_axis',(1.,0.,0.));
#30124=DIRECTION('ref_axis',(0.,0.,1.));
#30125=DIRECTION('',(1.,0.,0.));
#30126=DIRECTION('center_axis',(-1.,-4.44089209850062E-15,0.));
#30127=DIRECTION('ref_axis',(4.44089209850062E-15,-1.,0.));
#30128=DIRECTION('',(-1.,0.,0.));
#30129=DIRECTION('center_axis',(-4.44089209850064E-15,-1.,0.));
#30130=DIRECTION('ref_axis',(1.,-4.44089209850064E-15,0.));
#30131=DIRECTION('center_axis',(0.,0.,-1.));
#30132=DIRECTION('ref_axis',(0.707106781186547,-0.707106781186548,0.));
#30133=DIRECTION('center_axis',(0.,0.,1.));
#30134=DIRECTION('ref_axis',(0.707106781186547,-0.707106781186548,0.));
#30135=DIRECTION('center_axis',(0.,1.,0.));
#30136=DIRECTION('ref_axis',(0.707106781186551,0.,0.707106781186544));
#30137=DIRECTION('center_axis',(0.,-1.,0.));
#30138=DIRECTION('ref_axis',(1.,0.,0.));
#30139=DIRECTION('',(0.,-1.,0.));
#30140=DIRECTION('',(0.,1.,0.));
#30141=DIRECTION('center_axis',(1.,-4.44089209850062E-15,0.));
#30142=DIRECTION('ref_axis',(4.44089209850062E-15,1.,0.));
#30143=DIRECTION('center_axis',(0.,0.,-1.));
#30144=DIRECTION('ref_axis',(0.707106781186549,0.707106781186546,0.));
#30145=DIRECTION('center_axis',(-1.,0.,0.));
#30146=DIRECTION('ref_axis',(0.,0.707106781186551,0.707106781186544));
#30147=DIRECTION('center_axis',(1.,4.44089209850062E-15,0.));
#30148=DIRECTION('ref_axis',(-4.44089209850062E-15,1.,0.));
#30149=DIRECTION('',(1.,0.,0.));
#30150=DIRECTION('center_axis',(4.44089209850062E-15,1.,0.));
#30151=DIRECTION('ref_axis',(-1.,4.44089209850062E-15,0.));
#30152=DIRECTION('center_axis',(0.,0.,-1.));
#30153=DIRECTION('ref_axis',(-0.707106781186546,0.707106781186549,0.));
#30154=DIRECTION('center_axis',(0.,-1.,0.));
#30155=DIRECTION('ref_axis',(-0.707106781186551,0.,0.707106781186544));
#30156=DIRECTION('center_axis',(0.,1.,0.));
#30157=DIRECTION('ref_axis',(-1.,0.,0.));
#30158=DIRECTION('',(0.,1.,0.));
#30159=DIRECTION('center_axis',(0.,0.,-1.));
#30160=DIRECTION('ref_axis',(-0.707106781186548,-0.707106781186548,0.));
#30161=DIRECTION('center_axis',(0.,0.,1.));
#30162=DIRECTION('ref_axis',(-0.707106781186548,-0.707106781186548,0.));
#30163=DIRECTION('center_axis',(1.,0.,0.));
#30164=DIRECTION('ref_axis',(0.,1.,0.));
#30165=DIRECTION('',(0.,0.,1.));
#30166=DIRECTION('center_axis',(0.,0.,1.));
#30167=DIRECTION('ref_axis',(2.2204460492503E-15,-1.,0.));
#30168=DIRECTION('',(0.,0.,1.));
#30169=DIRECTION('center_axis',(0.,-1.,0.));
#30170=DIRECTION('ref_axis',(1.,0.,0.));
#30171=DIRECTION('',(0.,0.,1.));
#30172=DIRECTION('center_axis',(0.,0.,1.));
#30173=DIRECTION('ref_axis',(1.,0.,0.));
#30174=DIRECTION('center_axis',(0.,0.,1.));
#30175=DIRECTION('ref_axis',(7.40148683083437E-16,-1.,0.));
#30176=DIRECTION('',(1.,0.,0.));
#30177=DIRECTION('center_axis',(0.,0.,1.));
#30178=DIRECTION('ref_axis',(-1.,-1.11022302462516E-15,0.));
#30179=DIRECTION('',(0.,-1.,0.));
#30180=DIRECTION('center_axis',(0.,0.,1.));
#30181=DIRECTION('ref_axis',(-2.22044604925031E-15,1.,0.));
#30182=DIRECTION('',(-1.,0.,0.));
#30183=DIRECTION('center_axis',(0.,0.,1.));
#30184=DIRECTION('ref_axis',(1.,2.22044604925031E-15,0.));
#30185=DIRECTION('',(0.,1.,0.));
#30186=DIRECTION('center_axis',(0.,0.,-1.));
#30187=DIRECTION('ref_axis',(1.,0.,0.));
#30188=DIRECTION('center_axis',(0.,0.,-1.));
#30189=DIRECTION('ref_axis',(1.,0.,0.));
#30190=DIRECTION('center_axis',(0.,-1.,0.));
#30191=DIRECTION('ref_axis',(-0.707106781186557,0.,0.707106781186538));
#30192=DIRECTION('center_axis',(0.,-1.,0.));
#30193=DIRECTION('ref_axis',(0.,0.,1.));
#30194=DIRECTION('',(0.,-1.,0.));
#30195=DIRECTION('center_axis',(0.,1.,0.));
#30196=DIRECTION('ref_axis',(-1.,0.,0.));
#30197=DIRECTION('',(0.,1.,0.));
#30198=DIRECTION('center_axis',(-1.,0.,0.));
#30199=DIRECTION('ref_axis',(0.,-1.,0.));
#30200=DIRECTION('center_axis',(0.,0.,-1.));
#30201=DIRECTION('ref_axis',(-0.707106781186548,-0.707106781186548,0.));
#30202=DIRECTION('center_axis',(0.,0.,1.));
#30203=DIRECTION('ref_axis',(-0.707106781186547,-0.707106781186547,0.));
#30204=DIRECTION('center_axis',(1.,0.,0.));
#30205=DIRECTION('ref_axis',(0.,-0.707106781186555,0.70710678118654));
#30206=DIRECTION('center_axis',(-1.,0.,0.));
#30207=DIRECTION('ref_axis',(0.,-1.,0.));
#30208=DIRECTION('',(-1.,0.,0.));
#30209=DIRECTION('',(1.,0.,0.));
#30210=DIRECTION('center_axis',(2.22044604925031E-15,-1.,0.));
#30211=DIRECTION('ref_axis',(1.,2.22044604925031E-15,0.));
#30212=DIRECTION('center_axis',(0.,0.,-1.));
#30213=DIRECTION('ref_axis',(0.707106781186548,-0.707106781186548,0.));
#30214=DIRECTION('center_axis',(0.,0.,1.));
#30215=DIRECTION('ref_axis',(0.707106781186548,-0.707106781186548,0.));
#30216=DIRECTION('center_axis',(0.,1.,0.));
#30217=DIRECTION('ref_axis',(0.707106781186555,0.,0.70710678118654));
#30218=DIRECTION('center_axis',(0.,-1.,0.));
#30219=DIRECTION('ref_axis',(1.,0.,0.));
#30220=DIRECTION('',(0.,-1.,0.));
#30221=DIRECTION('',(0.,1.,0.));
#30222=DIRECTION('center_axis',(1.,2.22044604925032E-15,0.));
#30223=DIRECTION('ref_axis',(-2.22044604925032E-15,1.,0.));
#30224=DIRECTION('center_axis',(0.,0.,-1.));
#30225=DIRECTION('ref_axis',(0.707106781186548,0.707106781186548,0.));
#30226=DIRECTION('center_axis',(0.,0.,1.));
#30227=DIRECTION('ref_axis',(0.707106781186548,0.707106781186548,0.));
#30228=DIRECTION('center_axis',(-1.,0.,0.));
#30229=DIRECTION('ref_axis',(0.,0.707106781186555,0.70710678118654));
#30230=DIRECTION('center_axis',(1.,0.,0.));
#30231=DIRECTION('ref_axis',(0.,1.,0.));
#30232=DIRECTION('',(1.,0.,0.));
#30233=DIRECTION('',(-1.,0.,0.));
#30234=DIRECTION('center_axis',(0.,0.,-1.));
#30235=DIRECTION('ref_axis',(-0.707106781186549,0.707106781186546,0.));
#30236=DIRECTION('center_axis',(0.,0.,1.));
#30237=DIRECTION('ref_axis',(-0.707106781186549,0.707106781186546,0.));
#30238=DIRECTION('center_axis',(0.,0.,1.));
#30239=DIRECTION('ref_axis',(-1.48029736616688E-15,-1.,0.));
#30240=DIRECTION('',(0.,0.,1.));
#30241=DIRECTION('center_axis',(0.,0.,-1.));
#30242=DIRECTION('ref_axis',(-1.48029736616688E-15,-1.,0.));
#30243=DIRECTION('',(0.,0.,1.));
#30244=DIRECTION('center_axis',(0.,-1.,0.));
#30245=DIRECTION('ref_axis',(1.,0.,0.));
#30246=DIRECTION('',(0.,0.,1.));
#30247=DIRECTION('',(-1.,0.,0.));
#30248=DIRECTION('center_axis',(0.,0.,1.));
#30249=DIRECTION('ref_axis',(-1.,-1.48029736616687E-15,0.));
#30250=DIRECTION('',(0.,0.,1.));
#30251=DIRECTION('center_axis',(0.,0.,-1.));
#30252=DIRECTION('ref_axis',(-1.,-1.48029736616687E-15,0.));
#30253=DIRECTION('center_axis',(-1.,0.,0.));
#30254=DIRECTION('ref_axis',(0.,-1.,0.));
#30255=DIRECTION('',(0.,0.,1.));
#30256=DIRECTION('',(0.,1.,0.));
#30257=DIRECTION('center_axis',(0.,0.,1.));
#30258=DIRECTION('ref_axis',(1.,0.,0.));
#30259=DIRECTION('center_axis',(0.,0.,-1.));
#30260=DIRECTION('ref_axis',(1.,0.,0.));
#30261=DIRECTION('center_axis',(0.,-1.,0.));
#30262=DIRECTION('ref_axis',(-0.707106781186555,0.,0.70710678118654));
#30263=DIRECTION('center_axis',(0.,-1.,0.));
#30264=DIRECTION('ref_axis',(0.,0.,1.));
#30265=DIRECTION('',(0.,-1.,0.));
#30266=DIRECTION('center_axis',(0.,1.,0.));
#30267=DIRECTION('ref_axis',(-1.,0.,0.));
#30268=DIRECTION('',(0.,1.,0.));
#30269=DIRECTION('center_axis',(-1.,-2.22044604925031E-15,0.));
#30270=DIRECTION('ref_axis',(2.22044604925031E-15,-1.,0.));
#30271=DIRECTION('center_axis',(0.,0.,-1.));
#30272=DIRECTION('ref_axis',(-0.707106781186548,-0.707106781186548,0.));
#30273=DIRECTION('center_axis',(0.,0.,1.));
#30274=DIRECTION('ref_axis',(-0.707106781186548,-0.707106781186548,0.));
#30275=DIRECTION('center_axis',(1.,0.,0.));
#30276=DIRECTION('ref_axis',(0.,-0.707106781186555,0.70710678118654));
#30277=DIRECTION('center_axis',(-1.,0.,0.));
#30278=DIRECTION('ref_axis',(0.,-1.,0.));
#30279=DIRECTION('',(-1.,0.,0.));
#30280=DIRECTION('',(1.,0.,0.));
#30281=DIRECTION('center_axis',(-2.22044604925031E-15,-1.,0.));
#30282=DIRECTION('ref_axis',(1.,-2.22044604925031E-15,0.));
#30283=DIRECTION('center_axis',(0.,0.,-1.));
#30284=DIRECTION('ref_axis',(0.707106781186548,-0.707106781186548,0.));
#30285=DIRECTION('center_axis',(0.,0.,1.));
#30286=DIRECTION('ref_axis',(0.707106781186547,-0.707106781186547,0.));
#30287=DIRECTION('center_axis',(0.,1.,0.));
#30288=DIRECTION('ref_axis',(0.707106781186557,0.,0.707106781186538));
#30289=DIRECTION('center_axis',(0.,-1.,0.));
#30290=DIRECTION('ref_axis',(1.,0.,0.));
#30291=DIRECTION('',(0.,-1.,0.));
#30292=DIRECTION('',(0.,1.,0.));
#30293=DIRECTION('center_axis',(1.,0.,0.));
#30294=DIRECTION('ref_axis',(0.,1.,0.));
#30295=DIRECTION('center_axis',(0.,0.,-1.));
#30296=DIRECTION('ref_axis',(0.707106781186548,0.707106781186547,0.));
#30297=DIRECTION('center_axis',(0.,0.,1.));
#30298=DIRECTION('ref_axis',(0.707106781186548,0.707106781186547,0.));
#30299=DIRECTION('center_axis',(-1.,0.,0.));
#30300=DIRECTION('ref_axis',(0.,0.707106781186555,0.70710678118654));
#30301=DIRECTION('center_axis',(1.,0.,0.));
#30302=DIRECTION('ref_axis',(0.,1.,0.));
#30303=DIRECTION('',(1.,0.,0.));
#30304=DIRECTION('',(-1.,0.,0.));
#30305=DIRECTION('center_axis',(0.,0.,-1.));
#30306=DIRECTION('ref_axis',(-0.707106781186549,0.707106781186546,0.));
#30307=DIRECTION('center_axis',(0.,0.,1.));
#30308=DIRECTION('ref_axis',(-0.707106781186549,0.707106781186546,0.));
#30309=DIRECTION('center_axis',(0.,0.,1.));
#30310=DIRECTION('ref_axis',(0.,-1.,0.));
#30311=DIRECTION('',(0.,0.,1.));
#30312=DIRECTION('center_axis',(0.,0.,-1.));
#30313=DIRECTION('ref_axis',(0.,-1.,0.));
#30314=DIRECTION('',(0.,0.,1.));
#30315=DIRECTION('center_axis',(0.,-1.,0.));
#30316=DIRECTION('ref_axis',(1.,0.,0.));
#30317=DIRECTION('',(0.,0.,1.));
#30318=DIRECTION('',(-1.,0.,0.));
#30319=DIRECTION('center_axis',(0.,0.,1.));
#30320=DIRECTION('ref_axis',(-1.,1.48029736616688E-15,0.));
#30321=DIRECTION('',(0.,0.,1.));
#30322=DIRECTION('center_axis',(0.,0.,-1.));
#30323=DIRECTION('ref_axis',(-1.,1.48029736616688E-15,0.));
#30324=DIRECTION('center_axis',(-1.,0.,0.));
#30325=DIRECTION('ref_axis',(0.,-1.,0.));
#30326=DIRECTION('',(0.,0.,1.));
#30327=DIRECTION('',(0.,1.,0.));
#30328=DIRECTION('center_axis',(0.,0.,1.));
#30329=DIRECTION('ref_axis',(1.,0.,0.));
#30330=DIRECTION('center_axis',(0.,0.,-1.));
#30331=DIRECTION('ref_axis',(1.,0.,0.));
#30332=DIRECTION('center_axis',(0.,1.,0.));
#30333=DIRECTION('ref_axis',(0.,0.,1.));
#30334=DIRECTION('center_axis',(-1.,0.,1.22464679914735E-16));
#30335=DIRECTION('ref_axis',(-1.22464679914735E-16,0.,-1.));
#30336=DIRECTION('center_axis',(0.,1.,0.));
#30337=DIRECTION('ref_axis',(0.,0.,1.));
#30338=DIRECTION('center_axis',(0.,1.,0.));
#30339=DIRECTION('ref_axis',(0.,0.,1.));
#30340=DIRECTION('',(0.,1.,0.));
#30341=DIRECTION('center_axis',(0.,1.,0.));
#30342=DIRECTION('ref_axis',(0.5,0.,0.866025403784439));
#30343=DIRECTION('',(0.,1.,0.));
#30344=DIRECTION('center_axis',(0.,1.,0.));
#30345=DIRECTION('ref_axis',(1.,0.,0.));
#30346=DIRECTION('',(0.,1.,0.));
#30347=DIRECTION('center_axis',(0.,1.,0.));
#30348=DIRECTION('ref_axis',(0.5,0.,0.866025403784439));
#30349=DIRECTION('center_axis',(0.,1.,0.));
#30350=DIRECTION('ref_axis',(0.,0.,1.));
#30351=DIRECTION('center_axis',(0.,-1.,0.));
#30352=DIRECTION('ref_axis',(6.12323399573677E-17,0.,-1.));
#30353=DIRECTION('center_axis',(-1.,0.,1.22464679914735E-16));
#30354=DIRECTION('ref_axis',(-1.22464679914735E-16,0.,-1.));
#30355=DIRECTION('center_axis',(0.,1.,0.));
#30356=DIRECTION('ref_axis',(6.12323399573677E-17,0.,-1.));
#30357=DIRECTION('center_axis',(0.,1.,0.));
#30358=DIRECTION('ref_axis',(0.,0.,1.));
#30359=DIRECTION('',(-0.499999999999999,0.,-0.866025403784439));
#30360=DIRECTION('',(-0.5,0.,0.866025403784439));
#30361=DIRECTION('center_axis',(0.,1.,0.));
#30362=DIRECTION('ref_axis',(-1.1686558153949E-16,0.,-1.));
#30363=DIRECTION('center_axis',(0.,1.,0.));
#30364=DIRECTION('ref_axis',(0.,0.,1.));
#30365=DIRECTION('',(0.,1.,0.));
#30366=DIRECTION('center_axis',(0.,1.,0.));
#30367=DIRECTION('ref_axis',(1.,0.,0.));
#30368=DIRECTION('center_axis',(0.499999999999999,0.,0.866025403784439));
#30369=DIRECTION('ref_axis',(0.612372435695794,-0.707106781186549,-0.353553390593273));
#30370=DIRECTION('',(0.499999999999999,0.,0.866025403784439));
#30371=DIRECTION('center_axis',(0.,-1.,0.));
#30372=DIRECTION('ref_axis',(0.,0.,-1.));
#30373=DIRECTION('center_axis',(0.,-1.,0.));
#30374=DIRECTION('ref_axis',(-1.1686558153949E-16,0.,-1.));
#30375=DIRECTION('center_axis',(0.5,0.,-0.866025403784439));
#30376=DIRECTION('ref_axis',(-0.612372435695795,-0.707106781186548,-0.353553390593273));
#30377=DIRECTION('',(0.5,0.,-0.866025403784439));
#30378=DIRECTION('center_axis',(-0.866025403784439,0.,0.499999999999999));
#30379=DIRECTION('ref_axis',(0.499999999999999,0.,0.866025403784439));
#30380=DIRECTION('',(0.,1.,0.));
#30381=DIRECTION('',(0.499999999999999,0.,0.866025403784439));
#30382=DIRECTION('center_axis',(0.,1.,0.));
#30383=DIRECTION('ref_axis',(1.55820775385987E-16,0.,-1.));
#30384=DIRECTION('',(0.,1.,0.));
#30385=DIRECTION('center_axis',(0.,-1.,0.));
#30386=DIRECTION('ref_axis',(0.5,0.,0.866025403784439));
#30387=DIRECTION('center_axis',(0.866025403784439,0.,0.5));
#30388=DIRECTION('ref_axis',(0.5,0.,-0.866025403784439));
#30389=DIRECTION('',(0.5,0.,-0.866025403784439));
#30390=DIRECTION('center_axis',(-1.,0.,0.));
#30391=DIRECTION('ref_axis',(0.,0.,1.));
#30392=DIRECTION('center_axis',(-7.2886433738689E-15,0.474973683481511,
0.880000000000003));
#30393=DIRECTION('ref_axis',(1.,-1.11022302462515E-15,8.8817841970012E-15));
#30394=DIRECTION('center_axis',(-1.,0.,0.));
#30395=DIRECTION('ref_axis',(0.,1.5907673188659E-15,1.));
#30396=DIRECTION('center_axis',(-1.,0.,0.));
#30397=DIRECTION('ref_axis',(0.,1.5907673188659E-15,1.));
#30398=DIRECTION('center_axis',(0.,-0.474973683481513,0.880000000000002));
#30399=DIRECTION('ref_axis',(0.,-0.880000000000002,-0.474973683481513));
#30400=DIRECTION('center_axis',(1.,0.,0.));
#30401=DIRECTION('ref_axis',(0.,1.5907673188659E-15,1.));
#30402=DIRECTION('center_axis',(-1.02090452894056E-12,0.474973683483218,
0.879999999999082));
#30403=DIRECTION('ref_axis',(0.,-0.879999999999082,0.474973683483219));
#30404=DIRECTION('center_axis',(-1.,0.,0.));
#30405=DIRECTION('ref_axis',(0.,-9.12405358762789E-13,-1.));
#30406=DIRECTION('center_axis',(-5.27326719492196E-16,0.474973683481515,
-0.880000000000001));
#30407=DIRECTION('ref_axis',(0.,0.880000000000001,0.474973683481515));
#30408=DIRECTION('center_axis',(1.,0.,0.));
#30409=DIRECTION('ref_axis',(0.,2.12102309182119E-15,-1.));
#30410=DIRECTION('center_axis',(-1.,0.,0.));
#30411=DIRECTION('ref_axis',(0.,2.12102309182119E-15,-1.));
#30412=DIRECTION('center_axis',(0.,0.,1.));
#30413=DIRECTION('ref_axis',(-5.92118946466753E-15,-1.,0.));
#30414=DIRECTION('',(0.,0.,1.));
#30415=DIRECTION('center_axis',(0.,0.,1.));
#30416=DIRECTION('ref_axis',(0.707106781186548,-0.707106781186547,0.));
#30417=DIRECTION('',(0.,0.,1.));
#30418=DIRECTION('center_axis',(0.,0.,1.));
#30419=DIRECTION('ref_axis',(-5.92118946466753E-15,-1.,0.));
#30420=DIRECTION('',(0.,0.,1.));
#30421=DIRECTION('center_axis',(1.,0.,0.));
#30422=DIRECTION('ref_axis',(0.,1.,0.));
#30423=DIRECTION('',(0.,0.,1.));
#30424=DIRECTION('',(0.,1.,0.));
#30425=DIRECTION('center_axis',(-1.,0.,0.));
#30426=DIRECTION('ref_axis',(0.,0.,-1.));
#30427=DIRECTION('',(-1.,0.,0.));
#30428=DIRECTION('center_axis',(-1.,0.,0.));
#30429=DIRECTION('ref_axis',(0.,0.,-1.));
#30430=DIRECTION('center_axis',(-1.,0.,0.));
#30431=DIRECTION('ref_axis',(0.,0.707106781186544,-0.707106781186551));
#30432=DIRECTION('',(-1.,0.,0.));
#30433=DIRECTION('center_axis',(1.,8.88178419700124E-15,0.));
#30434=DIRECTION('ref_axis',(0.,0.,-1.));
#30435=DIRECTION('',(1.,0.,0.));
#30436=DIRECTION('center_axis',(0.,-1.,0.));
#30437=DIRECTION('ref_axis',(-0.707106781186544,0.,-0.707106781186551));
#30438=DIRECTION('center_axis',(0.,-1.,0.));
#30439=DIRECTION('ref_axis',(-1.,0.,0.));
#30440=DIRECTION('',(0.,-1.,0.));
#30441=DIRECTION('center_axis',(-1.11022302462516E-15,1.,0.));
#30442=DIRECTION('ref_axis',(0.,0.,-1.));
#30443=DIRECTION('',(0.,1.,0.));
#30444=DIRECTION('center_axis',(0.,0.,1.));
#30445=DIRECTION('ref_axis',(1.,0.,0.));
#30446=DIRECTION('center_axis',(-1.,-8.88178419700125E-15,0.));
#30447=DIRECTION('ref_axis',(0.,0.,-1.));
#30448=DIRECTION('center_axis',(0.,0.,-1.));
#30449=DIRECTION('ref_axis',(-0.707106781186545,-0.70710678118655,0.));
#30450=DIRECTION('center_axis',(0.,0.,1.));
#30451=DIRECTION('ref_axis',(-0.707106781186545,-0.70710678118655,0.));
#30452=DIRECTION('center_axis',(1.,0.,0.));
#30453=DIRECTION('ref_axis',(0.,-0.707106781186546,-0.707106781186549));
#30454=DIRECTION('',(-1.,0.,0.));
#30455=DIRECTION('',(1.,0.,0.));
#30456=DIRECTION('center_axis',(0.,0.,1.));
#30457=DIRECTION('ref_axis',(1.,0.,0.));
#30458=DIRECTION('center_axis',(0.,0.,-1.));
#30459=DIRECTION('ref_axis',(-0.707106781186548,0.707106781186548,0.));
#30460=DIRECTION('center_axis',(0.,0.,1.));
#30461=DIRECTION('ref_axis',(-0.707106781186548,0.707106781186548,0.));
#30462=DIRECTION('center_axis',(0.,0.,1.));
#30463=DIRECTION('ref_axis',(-1.,4.44089209850066E-15,0.));
#30464=DIRECTION('',(0.,0.,1.));
#30465=DIRECTION('center_axis',(0.,0.,1.));
#30466=DIRECTION('ref_axis',(-0.707106781186545,-0.70710678118655,0.));
#30467=DIRECTION('',(0.,0.,1.));
#30468=DIRECTION('',(0.,0.,1.));
#30469=DIRECTION('center_axis',(0.,-1.,0.));
#30470=DIRECTION('ref_axis',(1.,0.,0.));
#30471=DIRECTION('',(1.,0.,0.));
#30472=DIRECTION('',(1.,0.,0.));
#30473=DIRECTION('center_axis',(0.,0.,1.));
#30474=DIRECTION('ref_axis',(1.,0.,0.));
#30475=DIRECTION('center_axis',(0.,-1.,0.));
#30476=DIRECTION('ref_axis',(-0.707106781186548,0.,0.707106781186548));
#30477=DIRECTION('center_axis',(0.,-1.,0.));
#30478=DIRECTION('ref_axis',(0.,0.,1.));
#30479=DIRECTION('',(0.,-1.,0.));
#30480=DIRECTION('center_axis',(-1.11022302462516E-15,1.,0.));
#30481=DIRECTION('ref_axis',(-1.,-1.11022302462516E-15,0.));
#30482=DIRECTION('',(0.,1.,0.));
#30483=DIRECTION('center_axis',(0.,0.,1.));
#30484=DIRECTION('ref_axis',(1.,0.,0.));
#30485=DIRECTION('center_axis',(-1.,-8.88178419700125E-15,0.));
#30486=DIRECTION('ref_axis',(8.88178419700125E-15,-1.,0.));
#30487=DIRECTION('center_axis',(0.,0.,-1.));
#30488=DIRECTION('ref_axis',(-0.707106781186545,-0.70710678118655,0.));
#30489=DIRECTION('center_axis',(1.,0.,0.));
#30490=DIRECTION('ref_axis',(0.,-0.707106781186549,0.707106781186546));
#30491=DIRECTION('center_axis',(-1.,0.,0.));
#30492=DIRECTION('ref_axis',(0.,-1.,0.));
#30493=DIRECTION('',(-1.,0.,0.));
#30494=DIRECTION('center_axis',(0.,0.,1.));
#30495=DIRECTION('ref_axis',(1.,0.,0.));
#30496=DIRECTION('center_axis',(4.4408920985006E-15,-1.,0.));
#30497=DIRECTION('ref_axis',(1.,4.4408920985006E-15,0.));
#30498=DIRECTION('center_axis',(0.,0.,-1.));
#30499=DIRECTION('ref_axis',(0.707106781186548,-0.707106781186547,0.));
#30500=DIRECTION('center_axis',(0.,1.,0.));
#30501=DIRECTION('ref_axis',(0.707106781186548,0.,0.707106781186548));
#30502=DIRECTION('center_axis',(0.,-1.,0.));
#30503=DIRECTION('ref_axis',(1.,0.,0.));
#30504=DIRECTION('',(0.,-1.,0.));
#30505=DIRECTION('center_axis',(0.,0.,1.));
#30506=DIRECTION('ref_axis',(1.,0.,0.));
#30507=DIRECTION('center_axis',(1.,0.,0.));
#30508=DIRECTION('ref_axis',(0.,1.,0.));
#30509=DIRECTION('center_axis',(0.,0.,-1.));
#30510=DIRECTION('ref_axis',(0.707106781186548,0.707106781186548,0.));
#30511=DIRECTION('center_axis',(0.,0.,1.));
#30512=DIRECTION('ref_axis',(0.707106781186548,0.707106781186548,0.));
#30513=DIRECTION('center_axis',(-1.,0.,0.));
#30514=DIRECTION('ref_axis',(0.,0.707106781186548,0.707106781186548));
#30515=DIRECTION('center_axis',(1.,8.88178419700124E-15,0.));
#30516=DIRECTION('ref_axis',(-8.88178419700124E-15,1.,0.));
#30517=DIRECTION('',(1.,0.,0.));
#30518=DIRECTION('',(-1.,0.,0.));
#30519=DIRECTION('center_axis',(0.,0.,1.));
#30520=DIRECTION('ref_axis',(1.,0.,0.));
#30521=DIRECTION('center_axis',(0.,0.,-1.));
#30522=DIRECTION('ref_axis',(-0.707106781186548,0.707106781186548,0.));
#30523=DIRECTION('center_axis',(0.,0.,1.));
#30524=DIRECTION('ref_axis',(-0.707106781186548,0.707106781186548,0.));
#30525=DIRECTION('center_axis',(-1.,0.,0.));
#30526=DIRECTION('ref_axis',(0.,-1.,0.));
#30527=DIRECTION('',(0.,0.,1.));
#30528=DIRECTION('center_axis',(-1.,0.,0.));
#30529=DIRECTION('ref_axis',(0.,-1.32563943238825E-15,1.));
#30530=DIRECTION('center_axis',(0.,0.,1.));
#30531=DIRECTION('ref_axis',(1.,0.,0.));
#30532=DIRECTION('center_axis',(0.,0.,-1.));
#30533=DIRECTION('ref_axis',(0.,1.,0.));
#30534=DIRECTION('',(1.,0.,0.));
#30535=DIRECTION('center_axis',(0.,0.,-1.));
#30536=DIRECTION('ref_axis',(1.,-4.44089209850064E-15,0.));
#30537=DIRECTION('',(0.,-1.,0.));
#30538=DIRECTION('center_axis',(0.,0.,-1.));
#30539=DIRECTION('ref_axis',(2.96059473233376E-15,1.,0.));
#30540=DIRECTION('',(1.,0.,0.));
#30541=DIRECTION('center_axis',(0.,0.,-1.));
#30542=DIRECTION('ref_axis',(1.,-1.48029736616687E-15,0.));
#30543=DIRECTION('',(0.,-1.,0.));
#30544=DIRECTION('center_axis',(0.,0.,-1.));
#30545=DIRECTION('ref_axis',(1.,0.,0.));
#30546=DIRECTION('center_axis',(1.,0.,0.));
#30547=DIRECTION('ref_axis',(0.,5.1364535115188E-16,1.));
#30548=DIRECTION('center_axis',(0.,-0.47497368348152,0.879999999999998));
#30549=DIRECTION('ref_axis',(-1.,0.,0.));
#30550=DIRECTION('center_axis',(1.,0.,0.));
#30551=DIRECTION('ref_axis',(0.,-1.32563943238825E-15,1.));
#30552=DIRECTION('center_axis',(1.,0.,0.));
#30553=DIRECTION('ref_axis',(0.,-1.32563943238825E-15,1.));
#30554=DIRECTION('center_axis',(0.,0.474973683481518,0.88));
#30555=DIRECTION('ref_axis',(0.,0.88,-0.474973683481518));
#30556=DIRECTION('center_axis',(1.02248650909906E-12,-0.474973683483223,
0.879999999999079));
#30557=DIRECTION('ref_axis',(0.,0.879999999999079,0.474973683483223));
#30558=DIRECTION('center_axis',(1.,0.,0.));
#30559=DIRECTION('ref_axis',(0.,0.,-1.));
#30560=DIRECTION('center_axis',(0.,-0.474973683481516,-0.88));
#30561=DIRECTION('ref_axis',(0.,-0.88,0.474973683481516));
#30562=DIRECTION('center_axis',(-1.,0.,0.));
#30563=DIRECTION('ref_axis',(0.,-1.0605115459106E-15,-1.));
#30564=DIRECTION('center_axis',(1.,0.,0.));
#30565=DIRECTION('ref_axis',(0.,-1.0605115459106E-15,-1.));
#30566=DIRECTION('center_axis',(0.,0.,1.));
#30567=DIRECTION('ref_axis',(2.96059473233376E-15,1.,0.));
#30568=DIRECTION('',(0.,0.,1.));
#30569=DIRECTION('',(0.,0.,1.));
#30570=DIRECTION('center_axis',(1.,0.,0.));
#30571=DIRECTION('ref_axis',(0.,0.,-1.));
#30572=DIRECTION('',(1.,0.,0.));
#30573=DIRECTION('center_axis',(1.,0.,0.));
#30574=DIRECTION('ref_axis',(0.,0.,-1.));
#30575=DIRECTION('center_axis',(0.,0.,-1.));
#30576=DIRECTION('ref_axis',(1.,0.,0.));
#30577=DIRECTION('',(0.,0.,-1.));
#30578=DIRECTION('center_axis',(0.,0.,-1.));
#30579=DIRECTION('ref_axis',(1.,0.,0.));
#30580=DIRECTION('',(0.,0.,-1.));
#30581=DIRECTION('center_axis',(0.,0.,-1.));
#30582=DIRECTION('ref_axis',(1.,0.,0.));
#30583=DIRECTION('',(0.,0.,-1.));
#30584=DIRECTION('center_axis',(0.,0.,-1.));
#30585=DIRECTION('ref_axis',(1.,0.,0.));
#30586=DIRECTION('center_axis',(0.,0.,1.));
#30587=DIRECTION('ref_axis',(1.,0.,0.));
#30588=DIRECTION('center_axis',(0.,0.,-1.));
#30589=DIRECTION('ref_axis',(1.,0.,0.));
#30590=DIRECTION('',(0.,0.,-1.));
#30591=DIRECTION('center_axis',(0.,0.,-1.));
#30592=DIRECTION('ref_axis',(1.,0.,0.));
#30593=DIRECTION('center_axis',(0.,0.,1.));
#30594=DIRECTION('ref_axis',(1.,0.,0.));
#30595=DIRECTION('center_axis',(0.,0.,-1.));
#30596=DIRECTION('ref_axis',(1.,0.,0.));
#30597=DIRECTION('',(0.,0.,-1.));
#30598=DIRECTION('center_axis',(0.,0.,-1.));
#30599=DIRECTION('ref_axis',(1.,0.,0.));
#30600=DIRECTION('center_axis',(0.,0.,1.));
#30601=DIRECTION('ref_axis',(1.,0.,0.));
#30602=DIRECTION('center_axis',(1.,0.,0.));
#30603=DIRECTION('ref_axis',(0.,0.,-1.));
#30604=DIRECTION('center_axis',(-1.,0.,0.));
#30605=DIRECTION('ref_axis',(0.,-1.,0.));
#30606=DIRECTION('center_axis',(1.,0.,0.));
#30607=DIRECTION('ref_axis',(0.,0.,-1.));
#30608=DIRECTION('center_axis',(1.,0.,0.));
#30609=DIRECTION('ref_axis',(0.,1.,0.));
#30610=DIRECTION('',(0.,1.,0.));
#30611=DIRECTION('',(0.,0.,1.));
#30612=DIRECTION('center_axis',(0.,-1.,0.));
#30613=DIRECTION('ref_axis',(1.,0.,0.));
#30614=DIRECTION('',(0.,-1.,0.));
#30615=DIRECTION('center_axis',(0.,-1.,0.));
#30616=DIRECTION('ref_axis',(1.,0.,0.));
#30617=DIRECTION('center_axis',(0.,1.,0.));
#30618=DIRECTION('ref_axis',(1.,0.,0.));
#30619=DIRECTION('center_axis',(0.,-1.,0.));
#30620=DIRECTION('ref_axis',(1.,0.,0.));
#30621=DIRECTION('',(0.,-1.,0.));
#30622=DIRECTION('center_axis',(0.,-1.,0.));
#30623=DIRECTION('ref_axis',(1.,0.,0.));
#30624=DIRECTION('center_axis',(0.,1.,0.));
#30625=DIRECTION('ref_axis',(1.,0.,0.));
#30626=DIRECTION('center_axis',(0.,-1.,0.));
#30627=DIRECTION('ref_axis',(1.,0.,0.));
#30628=DIRECTION('',(0.,-1.,0.));
#30629=DIRECTION('center_axis',(0.,-1.,0.));
#30630=DIRECTION('ref_axis',(1.,0.,0.));
#30631=DIRECTION('center_axis',(0.,1.,0.));
#30632=DIRECTION('ref_axis',(1.,0.,0.));
#30633=DIRECTION('center_axis',(0.,-1.,0.));
#30634=DIRECTION('ref_axis',(1.,0.,0.));
#30635=DIRECTION('',(0.,-1.,0.));
#30636=DIRECTION('center_axis',(0.,-1.,0.));
#30637=DIRECTION('ref_axis',(1.,0.,0.));
#30638=DIRECTION('center_axis',(0.,1.,0.));
#30639=DIRECTION('ref_axis',(1.,0.,0.));
#30640=DIRECTION('center_axis',(0.,1.,0.));
#30641=DIRECTION('ref_axis',(1.,0.,0.));
#30642=DIRECTION('',(0.,1.,0.));
#30643=DIRECTION('center_axis',(0.,1.,0.));
#30644=DIRECTION('ref_axis',(1.,0.,0.));
#30645=DIRECTION('center_axis',(0.,1.,0.));
#30646=DIRECTION('ref_axis',(1.,0.,0.));
#30647=DIRECTION('center_axis',(0.,1.,0.));
#30648=DIRECTION('ref_axis',(1.,0.,0.));
#30649=DIRECTION('',(0.,1.,0.));
#30650=DIRECTION('center_axis',(0.,1.,0.));
#30651=DIRECTION('ref_axis',(1.,0.,0.));
#30652=DIRECTION('center_axis',(0.,1.,0.));
#30653=DIRECTION('ref_axis',(1.,0.,0.));
#30654=DIRECTION('center_axis',(0.,1.,0.));
#30655=DIRECTION('ref_axis',(1.,0.,0.));
#30656=DIRECTION('',(0.,1.,0.));
#30657=DIRECTION('center_axis',(0.,1.,0.));
#30658=DIRECTION('ref_axis',(1.,0.,0.));
#30659=DIRECTION('center_axis',(0.,1.,0.));
#30660=DIRECTION('ref_axis',(1.,0.,0.));
#30661=DIRECTION('center_axis',(0.,1.,0.));
#30662=DIRECTION('ref_axis',(1.,0.,0.));
#30663=DIRECTION('',(0.,1.,0.));
#30664=DIRECTION('center_axis',(0.,1.,0.));
#30665=DIRECTION('ref_axis',(1.,0.,0.));
#30666=DIRECTION('center_axis',(0.,1.,0.));
#30667=DIRECTION('ref_axis',(1.,0.,0.));
#30668=DIRECTION('center_axis',(0.,1.,0.));
#30669=DIRECTION('ref_axis',(1.,0.,0.));
#30670=DIRECTION('',(0.,1.,0.));
#30671=DIRECTION('center_axis',(0.,1.,0.));
#30672=DIRECTION('ref_axis',(1.,0.,0.));
#30673=DIRECTION('center_axis',(0.,1.,0.));
#30674=DIRECTION('ref_axis',(1.,0.,0.));
#30675=DIRECTION('center_axis',(0.,1.,0.));
#30676=DIRECTION('ref_axis',(1.,0.,0.));
#30677=DIRECTION('',(0.,1.,0.));
#30678=DIRECTION('center_axis',(0.,1.,0.));
#30679=DIRECTION('ref_axis',(1.,0.,0.));
#30680=DIRECTION('center_axis',(0.,1.,0.));
#30681=DIRECTION('ref_axis',(1.,0.,0.));
#30682=DIRECTION('center_axis',(0.,1.,0.));
#30683=DIRECTION('ref_axis',(1.,0.,0.));
#30684=DIRECTION('',(0.,1.,0.));
#30685=DIRECTION('center_axis',(0.,1.,0.));
#30686=DIRECTION('ref_axis',(1.,0.,0.));
#30687=DIRECTION('center_axis',(0.,1.,0.));
#30688=DIRECTION('ref_axis',(1.,0.,0.));
#30689=DIRECTION('center_axis',(0.,1.,0.));
#30690=DIRECTION('ref_axis',(1.,0.,0.));
#30691=DIRECTION('',(0.,1.,0.));
#30692=DIRECTION('center_axis',(0.,1.,0.));
#30693=DIRECTION('ref_axis',(1.,0.,0.));
#30694=DIRECTION('center_axis',(0.,1.,0.));
#30695=DIRECTION('ref_axis',(1.,0.,0.));
#30696=DIRECTION('center_axis',(0.,1.,0.));
#30697=DIRECTION('ref_axis',(1.,0.,0.));
#30698=DIRECTION('center_axis',(0.,1.,0.));
#30699=DIRECTION('ref_axis',(0.,0.,1.));
#30700=DIRECTION('center_axis',(0.,1.,0.));
#30701=DIRECTION('ref_axis',(1.,0.,0.));
#30702=DIRECTION('center_axis',(0.,1.,0.));
#30703=DIRECTION('ref_axis',(0.,0.,1.));
#30704=DIRECTION('',(0.,1.,0.));
#30705=DIRECTION('center_axis',(0.,0.,1.));
#30706=DIRECTION('ref_axis',(2.96059473233376E-15,1.,0.));
#30707=DIRECTION('',(0.,0.,1.));
#30708=DIRECTION('center_axis',(0.,1.,0.));
#30709=DIRECTION('ref_axis',(-1.,0.,0.));
#30710=DIRECTION('',(0.,0.,1.));
#30711=DIRECTION('center_axis',(0.,0.,1.));
#30712=DIRECTION('ref_axis',(1.,-1.48029736616687E-15,0.));
#30713=DIRECTION('',(0.,0.,1.));
#30714=DIRECTION('center_axis',(1.,0.,0.));
#30715=DIRECTION('ref_axis',(0.,1.,0.));
#30716=DIRECTION('center_axis',(0.,0.,1.));
#30717=DIRECTION('ref_axis',(0.,1.,0.));
#30718=DIRECTION('',(0.,0.,1.));
#30719=DIRECTION('center_axis',(0.,1.,0.));
#30720=DIRECTION('ref_axis',(-1.,0.,0.));
#30721=DIRECTION('',(0.,0.,1.));
#30722=DIRECTION('center_axis',(0.,0.,1.));
#30723=DIRECTION('ref_axis',(1.,-4.44089209850064E-15,0.));
#30724=DIRECTION('',(0.,0.,1.));
#30725=DIRECTION('center_axis',(1.,0.,0.));
#30726=DIRECTION('ref_axis',(0.,1.,0.));
#30727=DIRECTION('center_axis',(0.,0.,1.));
#30728=DIRECTION('ref_axis',(-1.,-4.44089209850061E-15,0.));
#30729=DIRECTION('center_axis',(0.,0.,1.));
#30730=DIRECTION('ref_axis',(7.40148683083437E-16,-1.,0.));
#30731=DIRECTION('',(0.,0.,1.));
#30732=DIRECTION('',(0.,0.,1.));
#30733=DIRECTION('center_axis',(0.,-1.,0.));
#30734=DIRECTION('ref_axis',(1.,0.,0.));
#30735=DIRECTION('',(0.,0.,1.));
#30736=DIRECTION('center_axis',(0.,0.,1.));
#30737=DIRECTION('ref_axis',(-1.,-1.11022302462516E-15,0.));
#30738=DIRECTION('',(0.,0.,1.));
#30739=DIRECTION('center_axis',(-1.,0.,0.));
#30740=DIRECTION('ref_axis',(0.,-1.,0.));
#30741=DIRECTION('',(0.,0.,1.));
#30742=DIRECTION('center_axis',(0.,0.,1.));
#30743=DIRECTION('ref_axis',(-2.22044604925031E-15,1.,0.));
#30744=DIRECTION('',(0.,0.,1.));
#30745=DIRECTION('center_axis',(0.,1.,0.));
#30746=DIRECTION('ref_axis',(-1.,0.,0.));
#30747=DIRECTION('',(0.,0.,1.));
#30748=DIRECTION('center_axis',(0.,0.,1.));
#30749=DIRECTION('ref_axis',(1.,2.22044604925031E-15,0.));
#30750=DIRECTION('',(0.,0.,1.));
#30751=DIRECTION('center_axis',(1.,0.,0.));
#30752=DIRECTION('ref_axis',(0.,1.,0.));
#30753=DIRECTION('center_axis',(0.,0.,1.));
#30754=DIRECTION('ref_axis',(1.,0.,0.));
#30755=DIRECTION('',(1.,0.,0.));
#30756=DIRECTION('center_axis',(0.,0.,1.));
#30757=DIRECTION('ref_axis',(1.,-2.96059473233376E-15,0.));
#30758=DIRECTION('center_axis',(0.,1.,0.));
#30759=DIRECTION('ref_axis',(-1.,0.,0.));
#30760=DIRECTION('',(0.,0.,1.));
#30761=DIRECTION('center_axis',(0.,0.,1.));
#30762=DIRECTION('ref_axis',(1.,-2.96059473233376E-15,0.));
#30763=DIRECTION('axis',(0.,0.,1.));
#30764=DIRECTION('refdir',(1.,0.,0.));
#30765=DIRECTION('',(-0.707106781186548,0.,0.707106781186547));
#30766=DIRECTION('',(0.70710678118655,-3.14018491736755E-15,-0.707106781186545));
#30767=DIRECTION('center_axis',(-0.707106781186546,0.,-0.707106781186549));
#30768=DIRECTION('ref_axis',(-0.707106781186549,0.,0.707106781186546));
#30769=DIRECTION('',(-0.707106781186549,0.,0.707106781186546));
#30770=DIRECTION('',(0.,-1.,0.));
#30771=DIRECTION('',(0.,1.,0.));
#30772=DIRECTION('center_axis',(0.,-1.,0.));
#30773=DIRECTION('ref_axis',(0.,0.,-1.));
#30774=DIRECTION('',(-1.,0.,0.));
#30775=DIRECTION('',(-0.707106781186548,0.,-0.707106781186547));
#30776=DIRECTION('',(-1.85037170770859E-16,0.,-1.));
#30777=DIRECTION('center_axis',(0.,-1.,0.));
#30778=DIRECTION('ref_axis',(0.,0.,1.));
#30779=DIRECTION('center_axis',(0.,-1.,0.));
#30780=DIRECTION('ref_axis',(0.,0.,1.));
#30781=DIRECTION('',(1.85037170770859E-16,0.,1.));
#30782=DIRECTION('center_axis',(1.,0.,0.));
#30783=DIRECTION('ref_axis',(0.,-0.707106781186548,-0.707106781186548));
#30784=DIRECTION('',(1.,0.,0.));
#30785=DIRECTION('center_axis',(0.,0.,-1.));
#30786=DIRECTION('ref_axis',(1.,0.,0.));
#30787=DIRECTION('',(-1.,0.,0.));
#30788=DIRECTION('',(0.,1.,0.));
#30789=DIRECTION('',(0.707106781186548,0.,0.707106781186547));
#30790=DIRECTION('center_axis',(0.707106781186552,0.,-0.707106781186543));
#30791=DIRECTION('ref_axis',(-0.707106781186543,0.,-0.707106781186552));
#30792=DIRECTION('',(-0.707106781186543,0.,-0.707106781186552));
#30793=DIRECTION('',(0.,-1.,0.));
#30794=DIRECTION('center_axis',(1.85037170770859E-16,0.,1.));
#30795=DIRECTION('ref_axis',(0.707106781186547,-0.707106781186548,0.));
#30796=DIRECTION('',(1.85037170770859E-16,0.,1.));
#30797=DIRECTION('center_axis',(1.,0.,-1.85037170770859E-16));
#30798=DIRECTION('ref_axis',(1.85037170770859E-16,0.,1.));
#30799=DIRECTION('',(-1.85037170770859E-16,0.,-1.));
#30800=DIRECTION('',(0.,1.,0.));
#30801=DIRECTION('',(0.707106781186547,0.,0.707106781186548));
#30802=DIRECTION('',(-0.707106781186546,0.,-0.707106781186549));
#30803=DIRECTION('center_axis',(-0.707106781186549,0.,0.707106781186546));
#30804=DIRECTION('ref_axis',(0.707106781186546,0.,0.707106781186549));
#30805=DIRECTION('',(0.707106781186546,0.,0.707106781186549));
#30806=DIRECTION('',(0.,-1.,0.));
#30807=DIRECTION('',(0.,1.,0.));
#30808=DIRECTION('center_axis',(0.,-1.,0.));
#30809=DIRECTION('ref_axis',(0.,0.,-1.));
#30810=DIRECTION('',(0.,0.,1.));
#30811=DIRECTION('',(-1.,0.,1.15648231731787E-16));
#30812=DIRECTION('center_axis',(0.,-1.,0.));
#30813=DIRECTION('ref_axis',(0.,0.,1.));
#30814=DIRECTION('',(1.,0.,-9.25185853854297E-17));
#30815=DIRECTION('center_axis',(0.,0.,-1.));
#30816=DIRECTION('ref_axis',(-0.707106781186548,-0.707106781186548,0.));
#30817=DIRECTION('',(0.,0.,-1.));
#30818=DIRECTION('center_axis',(0.,-3.70074341541719E-16,1.));
#30819=DIRECTION('ref_axis',(-1.,0.,0.));
#30820=DIRECTION('center_axis',(-1.,0.,0.));
#30821=DIRECTION('ref_axis',(0.,0.,-1.));
#30822=DIRECTION('',(0.,0.,1.));
#30823=DIRECTION('',(0.,1.,0.));
#30824=DIRECTION('',(0.707106781186548,0.,-0.707106781186547));
#30825=DIRECTION('',(-0.707106781186549,0.,0.707106781186546));
#30826=DIRECTION('center_axis',(0.707106781186546,0.,0.707106781186549));
#30827=DIRECTION('ref_axis',(0.707106781186549,0.,-0.707106781186546));
#30828=DIRECTION('',(0.707106781186549,0.,-0.707106781186546));
#30829=DIRECTION('',(0.,-1.,0.));
#30830=DIRECTION('',(0.,1.,0.));
#30831=DIRECTION('center_axis',(0.,-1.,0.));
#30832=DIRECTION('ref_axis',(0.,0.,-1.));
#30833=DIRECTION('',(1.,0.,0.));
#30834=DIRECTION('',(0.707106781186549,0.,0.707106781186546));
#30835=DIRECTION('',(6.93889390390723E-17,0.,1.));
#30836=DIRECTION('center_axis',(0.,-1.,0.));
#30837=DIRECTION('ref_axis',(0.,0.,1.));
#30838=DIRECTION('',(-9.25185853854297E-17,0.,-1.));
#30839=DIRECTION('center_axis',(-1.,0.,0.));
#30840=DIRECTION('ref_axis',(0.,-0.707106781186548,0.707106781186548));
#30841=DIRECTION('',(-1.,0.,0.));
#30842=DIRECTION('center_axis',(0.,0.,1.));
#30843=DIRECTION('ref_axis',(-1.,0.,0.));
#30844=DIRECTION('',(1.,0.,0.));
#30845=DIRECTION('',(0.,1.,0.));
#30846=DIRECTION('',(-0.707106781186548,0.,-0.707106781186547));
#30847=DIRECTION('center_axis',(-0.707106781186552,0.,0.707106781186543));
#30848=DIRECTION('ref_axis',(0.707106781186543,0.,0.707106781186552));
#30849=DIRECTION('',(0.707106781186543,0.,0.707106781186552));
#30850=DIRECTION('',(0.,-1.,0.));
#30851=DIRECTION('center_axis',(-6.93889390390723E-17,0.,-1.));
#30852=DIRECTION('ref_axis',(-0.707106781186547,-0.707106781186548,0.));
#30853=DIRECTION('',(-6.93889390390723E-17,0.,-1.));
#30854=DIRECTION('center_axis',(-1.,0.,6.93889390390723E-17));
#30855=DIRECTION('ref_axis',(-6.93889390390723E-17,0.,-1.));
#30856=DIRECTION('',(6.93889390390723E-17,0.,1.));
#30857=DIRECTION('',(0.,1.,0.));
#30858=DIRECTION('',(-0.707106781186547,0.,-0.707106781186548));
#30859=DIRECTION('',(0.707106781186544,0.,0.707106781186551));
#30860=DIRECTION('center_axis',(0.707106781186549,0.,-0.707106781186546));
#30861=DIRECTION('ref_axis',(-0.707106781186546,0.,-0.707106781186549));
#30862=DIRECTION('',(-0.707106781186546,0.,-0.707106781186549));
#30863=DIRECTION('',(0.,-1.,0.));
#30864=DIRECTION('',(0.,1.,0.));
#30865=DIRECTION('center_axis',(0.,-1.,0.));
#30866=DIRECTION('ref_axis',(0.,0.,-1.));
#30867=DIRECTION('',(0.,0.,-1.));
#30868=DIRECTION('',(0.707106781186546,0.,-0.707106781186549));
#30869=DIRECTION('',(1.,0.,0.));
#30870=DIRECTION('center_axis',(0.,-1.,0.));
#30871=DIRECTION('ref_axis',(0.,0.,1.));
#30872=DIRECTION('',(-1.,0.,0.));
#30873=DIRECTION('center_axis',(0.,0.,1.));
#30874=DIRECTION('ref_axis',(0.707106781186548,-0.707106781186548,0.));
#30875=DIRECTION('',(0.,0.,1.));
#30876=DIRECTION('center_axis',(1.,0.,0.));
#30877=DIRECTION('ref_axis',(0.,0.,1.));
#30878=DIRECTION('',(0.,0.,-1.));
#30879=DIRECTION('',(0.,1.,0.));
#30880=DIRECTION('',(-0.707106781186546,0.,0.707106781186549));
#30881=DIRECTION('center_axis',(0.707106781186543,0.,0.707106781186552));
#30882=DIRECTION('ref_axis',(0.707106781186552,0.,-0.707106781186543));
#30883=DIRECTION('',(0.707106781186552,0.,-0.707106781186543));
#30884=DIRECTION('',(0.,-1.,0.));
#30885=DIRECTION('center_axis',(-1.,0.,0.));
#30886=DIRECTION('ref_axis',(0.,-0.707106781186548,0.707106781186547));
#30887=DIRECTION('',(-1.,0.,0.));
#30888=DIRECTION('center_axis',(0.,0.,1.));
#30889=DIRECTION('ref_axis',(-1.,0.,0.));
#30890=DIRECTION('',(1.,0.,0.));
#30891=DIRECTION('',(0.,1.,0.));
#30892=DIRECTION('center_axis',(0.,1.,0.));
#30893=DIRECTION('ref_axis',(0.,0.,1.));
#30894=DIRECTION('center_axis',(0.,-1.,0.));
#30895=DIRECTION('ref_axis',(6.12323399573676E-17,0.,-1.));
#30896=DIRECTION('center_axis',(-1.,0.,1.22464679914735E-16));
#30897=DIRECTION('ref_axis',(-1.22464679914735E-16,0.,-1.));
#30898=DIRECTION('center_axis',(0.,1.,0.));
#30899=DIRECTION('ref_axis',(-3.06161699786838E-17,0.,-1.));
#30900=DIRECTION('center_axis',(0.,1.,0.));
#30901=DIRECTION('ref_axis',(0.,0.,1.));
#30902=DIRECTION('',(8.65956056235492E-17,-0.707106781186548,0.707106781186547));
#30903=DIRECTION('center_axis',(0.,-1.,0.));
#30904=DIRECTION('ref_axis',(-3.06161699786838E-17,0.,-1.));
#30905=DIRECTION('center_axis',(0.,1.,0.));
#30906=DIRECTION('ref_axis',(0.,0.,1.));
#30907=DIRECTION('center_axis',(0.,1.,0.));
#30908=DIRECTION('ref_axis',(6.12323399573676E-17,0.,-1.));
#30909=DIRECTION('',(0.,-1.,0.));
#30910=DIRECTION('center_axis',(0.,1.,0.));
#30911=DIRECTION('ref_axis',(0.,0.,1.));
#30912=DIRECTION('center_axis',(-1.,0.,1.22464679914735E-16));
#30913=DIRECTION('ref_axis',(-1.22464679914735E-16,0.,-1.));
#30914=DIRECTION('center_axis',(0.,1.,0.));
#30915=DIRECTION('ref_axis',(6.12323399573677E-17,0.,-1.));
#30916=DIRECTION('center_axis',(0.,-1.,0.));
#30917=DIRECTION('ref_axis',(0.,0.,-1.));
#30918=DIRECTION('center_axis',(0.,1.,0.));
#30919=DIRECTION('ref_axis',(1.,0.,0.));
#30920=DIRECTION('center_axis',(0.,1.,0.));
#30921=DIRECTION('ref_axis',(1.,0.,0.));
#30922=DIRECTION('center_axis',(0.,1.,0.));
#30923=DIRECTION('ref_axis',(1.,0.,0.));
#30924=DIRECTION('center_axis',(0.,1.,0.));
#30925=DIRECTION('ref_axis',(1.,0.,0.));
#30926=DIRECTION('center_axis',(0.,1.,0.));
#30927=DIRECTION('ref_axis',(1.,0.,0.));
#30928=DIRECTION('center_axis',(0.,1.,0.));
#30929=DIRECTION('ref_axis',(1.,0.,0.));
#30930=DIRECTION('center_axis',(0.,1.,0.));
#30931=DIRECTION('ref_axis',(1.,0.,0.));
#30932=DIRECTION('center_axis',(0.,1.,0.));
#30933=DIRECTION('ref_axis',(1.,0.,0.));
#30934=DIRECTION('',(1.85037170770859E-16,0.,1.));
#30935=DIRECTION('center_axis',(0.,1.,0.));
#30936=DIRECTION('ref_axis',(0.,0.,1.));
#30937=DIRECTION('',(-1.,0.,1.15648231731787E-16));
#30938=DIRECTION('center_axis',(0.,1.,0.));
#30939=DIRECTION('ref_axis',(-0.707106781186548,0.,-0.707106781186547));
#30940=DIRECTION('',(1.,0.,-9.25185853854297E-17));
#30941=DIRECTION('center_axis',(0.,1.,0.));
#30942=DIRECTION('ref_axis',(0.,0.,1.));
#30943=DIRECTION('',(-9.25185853854297E-17,0.,-1.));
#30944=DIRECTION('center_axis',(0.,1.,0.));
#30945=DIRECTION('ref_axis',(0.,0.,1.));
#30946=DIRECTION('',(-1.,0.,0.));
#30947=DIRECTION('center_axis',(0.,1.,0.));
#30948=DIRECTION('ref_axis',(0.,0.,1.));
#30949=DIRECTION('center_axis',(1.,0.,0.));
#30950=DIRECTION('ref_axis',(0.,-0.707106781186548,-0.707106781186547));
#30951=DIRECTION('',(1.,0.,0.));
#30952=DIRECTION('center_axis',(0.,0.,-1.));
#30953=DIRECTION('ref_axis',(1.,0.,0.));
#30954=DIRECTION('',(0.,-1.,0.));
#30955=DIRECTION('center_axis',(9.25185853854297E-17,0.,1.));
#30956=DIRECTION('ref_axis',(0.707106781186547,-0.707106781186548,0.));
#30957=DIRECTION('',(9.25185853854297E-17,0.,1.));
#30958=DIRECTION('center_axis',(1.,0.,-9.25185853854297E-17));
#30959=DIRECTION('ref_axis',(9.25185853854297E-17,0.,1.));
#30960=DIRECTION('',(0.,-1.,0.));
#30961=DIRECTION('center_axis',(0.,1.,0.));
#30962=DIRECTION('ref_axis',(0.,0.,1.));
#30963=DIRECTION('center_axis',(0.,-1.,0.));
#30964=DIRECTION('ref_axis',(6.12323399573677E-17,0.,-1.));
#30965=DIRECTION('center_axis',(-1.,0.,1.22464679914735E-16));
#30966=DIRECTION('ref_axis',(-1.22464679914735E-16,0.,-1.));
#30967=DIRECTION('center_axis',(0.,1.,0.));
#30968=DIRECTION('ref_axis',(0.,0.,1.));
#30969=DIRECTION('center_axis',(0.,1.,0.));
#30970=DIRECTION('ref_axis',(0.,0.,1.));
#30971=DIRECTION('center_axis',(0.,-1.,0.));
#30972=DIRECTION('ref_axis',(1.,0.,0.));
#30973=DIRECTION('center_axis',(0.,-1.,0.));
#30974=DIRECTION('ref_axis',(1.,0.,0.));
#30975=DIRECTION('center_axis',(0.,1.,0.));
#30976=DIRECTION('ref_axis',(0.,0.,1.));
#30977=DIRECTION('center_axis',(0.,-1.,0.));
#30978=DIRECTION('ref_axis',(1.,0.,0.));
#30979=DIRECTION('center_axis',(0.,-1.,0.));
#30980=DIRECTION('ref_axis',(1.,0.,0.));
#30981=DIRECTION('center_axis',(0.,1.,0.));
#30982=DIRECTION('ref_axis',(0.,0.,1.));
#30983=DIRECTION('center_axis',(0.,-1.,0.));
#30984=DIRECTION('ref_axis',(1.,0.,0.));
#30985=DIRECTION('center_axis',(0.,-1.,0.));
#30986=DIRECTION('ref_axis',(1.,0.,0.));
#30987=DIRECTION('center_axis',(0.,1.,0.));
#30988=DIRECTION('ref_axis',(0.,0.,1.));
#30989=DIRECTION('center_axis',(0.,-1.,0.));
#30990=DIRECTION('ref_axis',(1.,0.,0.));
#30991=DIRECTION('center_axis',(0.,-1.,0.));
#30992=DIRECTION('ref_axis',(1.,0.,0.));
#30993=DIRECTION('center_axis',(0.,1.,0.));
#30994=DIRECTION('ref_axis',(0.,0.,1.));
#30995=DIRECTION('center_axis',(0.,-1.,0.));
#30996=DIRECTION('ref_axis',(1.,0.,0.));
#30997=DIRECTION('center_axis',(0.,-1.,0.));
#30998=DIRECTION('ref_axis',(1.,0.,0.));
#30999=DIRECTION('center_axis',(0.,1.,0.));
#31000=DIRECTION('ref_axis',(0.,0.,1.));
#31001=DIRECTION('center_axis',(0.,-1.,0.));
#31002=DIRECTION('ref_axis',(1.,0.,0.));
#31003=DIRECTION('center_axis',(0.,-1.,0.));
#31004=DIRECTION('ref_axis',(1.,0.,0.));
#31005=DIRECTION('center_axis',(0.,1.,0.));
#31006=DIRECTION('ref_axis',(0.,0.,1.));
#31007=DIRECTION('center_axis',(0.,1.,0.));
#31008=DIRECTION('ref_axis',(0.,0.,1.));
#31009=DIRECTION('center_axis',(0.,-1.,0.));
#31010=DIRECTION('ref_axis',(1.,0.,0.));
#31011=DIRECTION('center_axis',(0.,-1.,0.));
#31012=DIRECTION('ref_axis',(1.,0.,0.));
#31013=DIRECTION('center_axis',(0.,1.,0.));
#31014=DIRECTION('ref_axis',(0.,0.,1.));
#31015=DIRECTION('center_axis',(0.,-1.,0.));
#31016=DIRECTION('ref_axis',(1.,0.,0.));
#31017=DIRECTION('center_axis',(0.,-1.,0.));
#31018=DIRECTION('ref_axis',(1.,0.,0.));
#31019=DIRECTION('center_axis',(0.,1.,0.));
#31020=DIRECTION('ref_axis',(0.,0.,1.));
#31021=DIRECTION('center_axis',(0.,-1.,0.));
#31022=DIRECTION('ref_axis',(-3.06161699786838E-17,0.,-1.));
#31023=DIRECTION('center_axis',(-1.,0.,1.22464679914735E-16));
#31024=DIRECTION('ref_axis',(-1.22464679914735E-16,0.,-1.));
#31025=DIRECTION('center_axis',(0.,1.,0.));
#31026=DIRECTION('ref_axis',(6.12323399573677E-17,0.,-1.));
#31027=DIRECTION('center_axis',(0.,1.,0.));
#31028=DIRECTION('ref_axis',(0.,0.,1.));
#31029=DIRECTION('center_axis',(0.,1.,0.));
#31030=DIRECTION('ref_axis',(-3.06161699786838E-17,0.,-1.));
#31031=DIRECTION('',(8.65956056235495E-17,-0.707106781186546,0.707106781186549));
#31032=DIRECTION('center_axis',(0.,-1.,0.));
#31033=DIRECTION('ref_axis',(0.,0.,-1.));
#31034=DIRECTION('',(0.996199654101518,0.,0.0870990767345742));
#31035=DIRECTION('',(-0.997179284808876,0.,-0.0750564717266851));
#31036=DIRECTION('',(-0.569209969005557,0.,-0.822192198445529));
#31037=DIRECTION('',(0.,0.,-1.));
#31038=DIRECTION('',(-1.,0.,0.));
#31039=DIRECTION('',(0.,0.,1.));
#31040=DIRECTION('',(-0.555834771638921,0.,0.831292792364464));
#31041=DIRECTION('',(1.,0.,0.));
#31042=DIRECTION('',(0.547249318401935,0.,-0.836969643122507));
#31043=DIRECTION('',(0.550221176517859,0.,0.835018956019145));
#31044=DIRECTION('',(1.,0.,0.));
#31045=DIRECTION('',(1.,0.,0.));
#31046=DIRECTION('',(0.,0.,-1.));
#31047=DIRECTION('',(-1.,0.,0.));
#31048=DIRECTION('',(0.,0.,-1.));
#31049=DIRECTION('',(1.,0.,0.));
#31050=DIRECTION('',(0.,0.,-1.));
#31051=DIRECTION('',(-1.,0.,0.));
#31052=DIRECTION('',(0.,0.,-1.));
#31053=DIRECTION('',(1.,0.,0.));
#31054=DIRECTION('',(0.,0.,-1.));
#31055=DIRECTION('',(1.,0.,0.));
#31056=DIRECTION('',(0.,0.,-1.));
#31057=DIRECTION('',(1.,0.,0.));
#31058=DIRECTION('',(1.,0.,0.));
#31059=DIRECTION('',(0.,0.,-1.));
#31060=DIRECTION('',(1.,0.,0.));
#31061=DIRECTION('',(0.53851434427711,0.,-0.842616342713452));
#31062=DIRECTION('',(-0.358509645558692,0.,-0.933526022155452));
#31063=DIRECTION('',(-1.,0.,0.));
#31064=DIRECTION('',(-0.378780343133087,0.,0.925486602634517));
#31065=DIRECTION('',(-1.,0.,0.));
#31066=DIRECTION('',(-0.359401529578064,0.,0.933183015563907));
#31067=DIRECTION('',(-1.,0.,0.));
#31068=DIRECTION('',(-0.340892911214198,0.,-0.940102134389614));
#31069=DIRECTION('',(-1.,0.,0.));
#31070=DIRECTION('',(-0.536696416993486,0.,0.843775417979425));
#31071=DIRECTION('',(-1.,0.,0.));
#31072=DIRECTION('',(0.,0.,-1.));
#31073=DIRECTION('',(1.,0.,0.));
#31074=DIRECTION('',(0.,0.,-1.));
#31075=DIRECTION('center_axis',(-1.,0.,9.25185853854297E-17));
#31076=DIRECTION('ref_axis',(0.,-0.707106781186548,0.707106781186547));
#31077=DIRECTION('',(-1.,0.,9.25185853854297E-17));
#31078=DIRECTION('center_axis',(0.,-1.,0.));
#31079=DIRECTION('ref_axis',(-0.707106781186548,0.,-0.707106781186547));
#31080=DIRECTION('center_axis',(0.,1.,0.));
#31081=DIRECTION('ref_axis',(0.,0.,-1.));
#31082=DIRECTION('',(0.,-1.,0.));
#31083=DIRECTION('center_axis',(0.40824829046386,0.408248290463862,-0.816496580927728));
#31084=DIRECTION('ref_axis',(-0.577350269189624,-0.577350269189627,-0.577350269189626));
#31085=DIRECTION('center_axis',(-1.,0.,1.15648231731787E-16));
#31086=DIRECTION('ref_axis',(0.,-0.707106781186549,-0.707106781186546));
#31087=DIRECTION('center_axis',(1.,0.,-1.15648231731787E-16));
#31088=DIRECTION('ref_axis',(0.,-0.707106781186548,-0.707106781186547));
#31089=DIRECTION('',(1.,0.,-1.15648231731787E-16));
#31090=DIRECTION('center_axis',(-1.15648231731787E-16,0.,-1.));
#31091=DIRECTION('ref_axis',(1.,0.,-1.15648231731787E-16));
#31092=DIRECTION('',(0.,1.,0.));
#31093=DIRECTION('center_axis',(0.,1.,0.));
#31094=DIRECTION('ref_axis',(0.,0.,1.));
#31095=DIRECTION('center_axis',(0.,-1.,0.));
#31096=DIRECTION('ref_axis',(6.12323399573677E-17,0.,-1.));
#31097=DIRECTION('center_axis',(-1.,0.,1.22464679914735E-16));
#31098=DIRECTION('ref_axis',(-1.22464679914735E-16,0.,-1.));
#31099=DIRECTION('center_axis',(0.,1.,0.));
#31100=DIRECTION('ref_axis',(0.,0.,1.));
#31101=DIRECTION('',(0.,-1.,0.));
#31102=DIRECTION('',(0.,-1.,0.));
#31103=DIRECTION('',(0.,-1.,0.));
#31104=DIRECTION('center_axis',(-1.85037170770859E-16,0.,-1.));
#31105=DIRECTION('ref_axis',(-0.707106781186547,-0.707106781186548,0.));
#31106=DIRECTION('',(-1.85037170770859E-16,0.,-1.));
#31107=DIRECTION('center_axis',(-1.,0.,1.85037170770859E-16));
#31108=DIRECTION('ref_axis',(-1.85037170770859E-16,0.,-1.));
#31109=DIRECTION('center_axis',(0.,1.,0.));
#31110=DIRECTION('ref_axis',(-1.22464679914735E-16,0.,-1.));
#31111=DIRECTION('center_axis',(0.,-1.,0.));
#31112=DIRECTION('ref_axis',(1.94775969232484E-16,0.,-1.));
#31113=DIRECTION('center_axis',(0.,1.,0.));
#31114=DIRECTION('ref_axis',(1.94775969232484E-16,0.,-1.));
#31115=DIRECTION('center_axis',(-0.499999999999999,0.,-0.866025403784439));
#31116=DIRECTION('ref_axis',(0.612372435695794,0.707106781186546,-0.353553390593278));
#31117=DIRECTION('',(0.499999999999999,0.,0.866025403784439));
#31118=DIRECTION('',(-0.499999999999999,0.,-0.866025403784439));
#31119=DIRECTION('center_axis',(-0.5,0.,0.866025403784439));
#31120=DIRECTION('ref_axis',(-0.612372435695794,0.707106781186546,-0.353553390593278));
#31121=DIRECTION('',(-0.5,0.,0.866025403784439));
#31122=DIRECTION('',(0.5,0.,-0.866025403784439));
#31123=DIRECTION('center_axis',(0.,-1.,0.));
#31124=DIRECTION('ref_axis',(0.,0.,-1.));
#31125=DIRECTION('center_axis',(0.,1.,0.));
#31126=DIRECTION('ref_axis',(1.,0.,0.));
#31127=DIRECTION('center_axis',(0.,1.,0.));
#31128=DIRECTION('ref_axis',(2.13501882696539E-19,0.,-1.));
#31129=DIRECTION('center_axis',(0.,-1.,0.));
#31130=DIRECTION('ref_axis',(2.13501882696539E-19,0.,-1.));
#31131=DIRECTION('center_axis',(0.,-1.,0.));
#31132=DIRECTION('ref_axis',(2.13501882696539E-19,0.,-1.));
#31133=DIRECTION('center_axis',(1.,0.,1.22678181797432E-16));
#31134=DIRECTION('ref_axis',(-1.22678181797432E-16,0.,1.));
#31135=DIRECTION('center_axis',(0.,1.,0.));
#31136=DIRECTION('ref_axis',(1.,0.,0.));
#31137=DIRECTION('center_axis',(0.,1.,0.));
#31138=DIRECTION('ref_axis',(0.,0.,1.));
#31139=DIRECTION('',(0.,-1.,0.));
#31140=DIRECTION('center_axis',(0.,-1.,0.));
#31141=DIRECTION('ref_axis',(0.5,0.,0.866025403784439));
#31142=DIRECTION('',(0.,1.,0.));
#31143=DIRECTION('center_axis',(0.,-1.,0.));
#31144=DIRECTION('ref_axis',(0.5,0.,0.866025403784439));
#31145=DIRECTION('',(0.,-1.,0.));
#31146=DIRECTION('center_axis',(0.,-1.,0.));
#31147=DIRECTION('ref_axis',(0.,0.,-1.));
#31148=DIRECTION('center_axis',(-1.,0.,-1.22464679914735E-16));
#31149=DIRECTION('ref_axis',(-1.22464679914735E-16,0.,1.));
#31150=DIRECTION('center_axis',(0.,-1.,0.));
#31151=DIRECTION('ref_axis',(0.,0.,1.));
#31152=DIRECTION('center_axis',(0.,-1.,0.));
#31153=DIRECTION('ref_axis',(0.,0.,1.));
#31154=DIRECTION('center_axis',(0.,1.,0.));
#31155=DIRECTION('ref_axis',(1.,0.,0.));
#31156=DIRECTION('',(0.,1.,0.));
#31157=DIRECTION('center_axis',(0.,1.,0.));
#31158=DIRECTION('ref_axis',(1.,0.,0.));
#31159=DIRECTION('',(0.,1.,0.));
#31160=DIRECTION('center_axis',(0.,1.,0.));
#31161=DIRECTION('ref_axis',(1.,0.,0.));
#31162=DIRECTION('',(0.,1.,0.));
#31163=DIRECTION('center_axis',(0.,1.,0.));
#31164=DIRECTION('ref_axis',(1.,0.,0.));
#31165=DIRECTION('',(0.,1.,0.));
#31166=DIRECTION('center_axis',(0.,1.,0.));
#31167=DIRECTION('ref_axis',(0.,0.,1.));
#31168=DIRECTION('center_axis',(0.,1.,0.));
#31169=DIRECTION('ref_axis',(1.,0.,0.));
#31170=DIRECTION('',(0.,1.,0.));
#31171=DIRECTION('center_axis',(0.,0.,-1.));
#31172=DIRECTION('ref_axis',(0.745355992499931,-0.666666666666666,0.));
#31173=DIRECTION('center_axis',(0.,0.,1.));
#31174=DIRECTION('ref_axis',(0.745355992499931,-0.666666666666666,0.));
#31175=DIRECTION('center_axis',(0.,0.,-1.));
#31176=DIRECTION('ref_axis',(0.745355992499931,-0.666666666666666,0.));
#31177=DIRECTION('',(0.,0.,1.));
#31178=DIRECTION('center_axis',(0.,0.,-1.));
#31179=DIRECTION('ref_axis',(0.745355992499931,-0.666666666666666,0.));
#31180=DIRECTION('center_axis',(0.,0.,1.));
#31181=DIRECTION('ref_axis',(0.745355992499931,-0.666666666666666,0.));
#31182=DIRECTION('center_axis',(0.,0.,-1.));
#31183=DIRECTION('ref_axis',(0.745355992499931,-0.666666666666666,0.));
#31184=DIRECTION('',(0.,0.,1.));
#31185=DIRECTION('center_axis',(0.,0.,-1.));
#31186=DIRECTION('ref_axis',(0.745355992499931,-0.666666666666666,0.));
#31187=DIRECTION('center_axis',(0.,0.,1.));
#31188=DIRECTION('ref_axis',(0.745355992499931,-0.666666666666666,0.));
#31189=DIRECTION('center_axis',(0.,0.,-1.));
#31190=DIRECTION('ref_axis',(0.745355992499931,-0.666666666666666,0.));
#31191=DIRECTION('',(0.,0.,1.));
#31192=DIRECTION('center_axis',(-0.358509645558692,0.,-0.933526022155452));
#31193=DIRECTION('ref_axis',(0.695809214768189,-0.666666666666666,-0.267217312686197));
#31194=DIRECTION('center_axis',(0.,0.,1.));
#31195=DIRECTION('ref_axis',(1.,6.90948055922478E-16,0.));
#31196=DIRECTION('center_axis',(0.842616342713453,0.,0.53851434427711));
#31197=DIRECTION('ref_axis',(0.53851434427711,7.44592572834826E-17,-0.842616342713453));
#31198=DIRECTION('center_axis',(0.,0.,-1.));
#31199=DIRECTION('ref_axis',(1.,6.90948055922478E-16,0.));
#31200=DIRECTION('',(0.358509645558692,0.,0.933526022155452));
#31201=DIRECTION('center_axis',(-0.378780343133087,0.,0.925486602634517));
#31202=DIRECTION('ref_axis',(-0.68981698525204,-0.666666666666666,-0.282326198595426));
#31203=DIRECTION('center_axis',(0.,0.,-1.));
#31204=DIRECTION('ref_axis',(-1.,-1.71249422537826E-16,0.));
#31205=DIRECTION('center_axis',(0.,0.,1.));
#31206=DIRECTION('ref_axis',(-1.,-1.71249422537826E-16,0.));
#31207=DIRECTION('',(0.378780343133087,0.,-0.925486602634517));
#31208=DIRECTION('center_axis',(0.,0.,-1.));
#31209=DIRECTION('ref_axis',(-1.,0.,0.));
#31210=DIRECTION('',(0.,1.,0.));
#31211=DIRECTION('',(-1.,0.,0.));
#31212=DIRECTION('',(0.,1.,0.));
#31213=DIRECTION('center_axis',(-0.933183015563908,0.,-0.359401529578064));
#31214=DIRECTION('ref_axis',(-0.359401529578064,0.,0.933183015563907));
#31215=DIRECTION('',(0.,1.,0.));
#31216=DIRECTION('',(-0.359401529578064,0.,0.933183015563907));
#31217=DIRECTION('center_axis',(0.,0.,-1.));
#31218=DIRECTION('ref_axis',(-1.,0.,0.));
#31219=DIRECTION('',(-1.,0.,0.));
#31220=DIRECTION('center_axis',(0.,0.,1.));
#31221=DIRECTION('ref_axis',(1.,0.,0.));
#31222=DIRECTION('',(1.,0.,0.));
#31223=DIRECTION('center_axis',(0.,0.,-1.));
#31224=DIRECTION('ref_axis',(-1.,0.,0.));
#31225=DIRECTION('',(0.,1.,0.));
#31226=DIRECTION('',(-1.,0.,0.));
#31227=DIRECTION('',(0.,1.,0.));
#31228=DIRECTION('',(-1.,0.,0.));
#31229=DIRECTION('',(0.,1.,0.));
#31230=DIRECTION('center_axis',(0.940102134389614,0.,-0.340892911214198));
#31231=DIRECTION('ref_axis',(-0.340892911214198,0.,-0.940102134389614));
#31232=DIRECTION('',(-0.340892911214198,0.,-0.940102134389614));
#31233=DIRECTION('center_axis',(0.,1.,0.));
#31234=DIRECTION('ref_axis',(0.,0.,1.));
#31235=DIRECTION('center_axis',(0.,0.,1.));
#31236=DIRECTION('ref_axis',(1.,0.,0.));
#31237=DIRECTION('',(0.,1.,0.));
#31238=DIRECTION('',(1.,0.,0.));
#31239=DIRECTION('',(0.,1.,0.));
#31240=DIRECTION('center_axis',(1.,0.,0.));
#31241=DIRECTION('ref_axis',(0.,0.,-1.));
#31242=DIRECTION('',(0.,1.,0.));
#31243=DIRECTION('',(0.,0.,-1.));
#31244=DIRECTION('center_axis',(0.,0.,-1.));
#31245=DIRECTION('ref_axis',(-1.,0.,0.));
#31246=DIRECTION('',(0.,1.,0.));
#31247=DIRECTION('',(-1.,0.,0.));
#31248=DIRECTION('center_axis',(1.,0.,0.));
#31249=DIRECTION('ref_axis',(0.,0.,-1.));
#31250=DIRECTION('',(0.,1.,0.));
#31251=DIRECTION('',(0.,0.,-1.));
#31252=DIRECTION('center_axis',(0.,0.,1.));
#31253=DIRECTION('ref_axis',(1.,0.,0.));
#31254=DIRECTION('',(0.,1.,0.));
#31255=DIRECTION('',(1.,0.,0.));
#31256=DIRECTION('center_axis',(1.,0.,0.));
#31257=DIRECTION('ref_axis',(0.,0.,-1.));
#31258=DIRECTION('',(0.,1.,0.));
#31259=DIRECTION('',(0.,0.,-1.));
#31260=DIRECTION('center_axis',(0.,0.,-1.));
#31261=DIRECTION('ref_axis',(-1.,0.,0.));
#31262=DIRECTION('',(0.,1.,0.));
#31263=DIRECTION('',(-1.,0.,0.));
#31264=DIRECTION('center_axis',(1.,0.,0.));
#31265=DIRECTION('ref_axis',(0.,0.,-1.));
#31266=DIRECTION('',(0.,1.,0.));
#31267=DIRECTION('',(0.,0.,-1.));
#31268=DIRECTION('center_axis',(0.,0.,1.));
#31269=DIRECTION('ref_axis',(1.,0.,0.));
#31270=DIRECTION('',(1.,0.,0.));
#31271=DIRECTION('center_axis',(0.,0.,-1.));
#31272=DIRECTION('ref_axis',(-1.,0.,0.));
#31273=DIRECTION('',(0.,1.,0.));
#31274=DIRECTION('',(-1.,0.,0.));
#31275=DIRECTION('center_axis',(1.,0.,0.));
#31276=DIRECTION('ref_axis',(0.,0.,-1.));
#31277=DIRECTION('',(0.,0.,-1.));
#31278=DIRECTION('center_axis',(0.,1.,0.));
#31279=DIRECTION('ref_axis',(0.,0.,1.));
#31280=DIRECTION('',(0.,1.,0.));
#31281=DIRECTION('',(0.,1.,0.));
#31282=DIRECTION('',(0.,1.,0.));
#31283=DIRECTION('',(0.,1.,0.));
#31284=DIRECTION('',(0.,1.,0.));
#31285=DIRECTION('',(0.,1.,0.));
#31286=DIRECTION('',(0.,1.,0.));
#31287=DIRECTION('',(0.,1.,0.));
#31288=DIRECTION('',(0.,1.,0.));
#31289=DIRECTION('',(0.,1.,0.));
#31290=DIRECTION('',(0.,1.,0.));
#31291=DIRECTION('center_axis',(0.,0.,1.));
#31292=DIRECTION('ref_axis',(1.,0.,0.));
#31293=DIRECTION('',(1.,0.,0.));
#31294=DIRECTION('center_axis',(0.,0.,-1.));
#31295=DIRECTION('ref_axis',(-1.,0.,0.));
#31296=DIRECTION('',(0.,1.,0.));
#31297=DIRECTION('',(-1.,0.,0.));
#31298=DIRECTION('center_axis',(0.,-1.,0.));
#31299=DIRECTION('ref_axis',(0.,0.,-1.));
#31300=DIRECTION('',(0.,1.,0.));
#31301=DIRECTION('',(0.,1.,0.));
#31302=DIRECTION('',(0.,1.,0.));
#31303=DIRECTION('',(0.,1.,0.));
#31304=DIRECTION('',(0.,1.,0.));
#31305=DIRECTION('',(0.,1.,0.));
#31306=DIRECTION('',(0.,1.,0.));
#31307=DIRECTION('',(0.,1.,0.));
#31308=DIRECTION('',(0.,1.,0.));
#31309=DIRECTION('',(0.,1.,0.));
#31310=DIRECTION('',(0.,1.,0.));
#31311=DIRECTION('',(0.,1.,0.));
#31312=DIRECTION('',(0.,1.,0.));
#31313=DIRECTION('',(0.,1.,0.));
#31314=DIRECTION('center_axis',(0.0750564717266851,0.,-0.997179284808876));
#31315=DIRECTION('ref_axis',(-0.997179284808876,0.,-0.0750564717266851));
#31316=DIRECTION('',(0.,1.,0.));
#31317=DIRECTION('',(-0.997179284808876,0.,-0.0750564717266851));
#31318=DIRECTION('',(0.,1.,0.));
#31319=DIRECTION('',(0.,1.,0.));
#31320=DIRECTION('',(0.,1.,0.));
#31321=DIRECTION('',(0.,1.,0.));
#31322=DIRECTION('',(0.,1.,0.));
#31323=DIRECTION('',(0.,1.,0.));
#31324=DIRECTION('',(0.,1.,0.));
#31325=DIRECTION('',(0.,1.,0.));
#31326=DIRECTION('',(0.,1.,0.));
#31327=DIRECTION('',(0.,1.,0.));
#31328=DIRECTION('',(0.,1.,0.));
#31329=DIRECTION('',(0.,1.,0.));
#31330=DIRECTION('',(0.,1.,0.));
#31331=DIRECTION('',(0.,1.,0.));
#31332=DIRECTION('',(0.,1.,0.));
#31333=DIRECTION('',(0.,1.,0.));
#31334=DIRECTION('',(0.,1.,0.));
#31335=DIRECTION('',(0.,1.,0.));
#31336=DIRECTION('center_axis',(-0.0870990767345742,0.,0.996199654101518));
#31337=DIRECTION('ref_axis',(0.996199654101518,0.,0.0870990767345742));
#31338=DIRECTION('',(0.,1.,0.));
#31339=DIRECTION('',(0.996199654101518,0.,0.0870990767345742));
#31340=DIRECTION('',(0.,1.,0.));
#31341=DIRECTION('center_axis',(0.,-1.,0.));
#31342=DIRECTION('ref_axis',(0.,0.,-1.));
#31343=DIRECTION('center_axis',(0.,0.,-1.));
#31344=DIRECTION('ref_axis',(-1.,0.,0.));
#31345=DIRECTION('',(0.,1.,0.));
#31346=DIRECTION('',(-1.,0.,0.));
#31347=DIRECTION('',(0.,1.,0.));
#31348=DIRECTION('',(0.,1.,0.));
#31349=DIRECTION('',(0.,1.,0.));
#31350=DIRECTION('',(0.,1.,0.));
#31351=DIRECTION('',(0.,1.,0.));
#31352=DIRECTION('center_axis',(-0.843775417979425,0.,-0.536696416993487));
#31353=DIRECTION('ref_axis',(-0.536696416993486,0.,0.843775417979425));
#31354=DIRECTION('',(-0.536696416993487,0.,0.843775417979425));
#31355=DIRECTION('center_axis',(0.842616342713453,0.,0.53851434427711));
#31356=DIRECTION('ref_axis',(0.53851434427711,0.,-0.842616342713452));
#31357=DIRECTION('',(0.,1.,0.));
#31358=DIRECTION('',(0.53851434427711,0.,-0.842616342713452));
#31359=DIRECTION('',(0.,1.,0.));
#31360=DIRECTION('',(0.,1.,0.));
#31361=DIRECTION('',(0.,1.,0.));
#31362=DIRECTION('',(0.,1.,0.));
#31363=DIRECTION('',(0.,1.,0.));
#31364=DIRECTION('',(0.,1.,0.));
#31365=DIRECTION('',(0.,1.,0.));
#31366=DIRECTION('center_axis',(0.,0.,1.));
#31367=DIRECTION('ref_axis',(1.,0.,0.));
#31368=DIRECTION('',(1.,0.,0.));
#31369=DIRECTION('center_axis',(0.,0.,-1.));
#31370=DIRECTION('ref_axis',(-1.,0.,0.));
#31371=DIRECTION('',(0.,1.,0.));
#31372=DIRECTION('',(-1.,0.,0.));
#31373=DIRECTION('center_axis',(1.,0.,0.));
#31374=DIRECTION('ref_axis',(0.,0.,-1.));
#31375=DIRECTION('',(0.,0.,-1.));
#31376=DIRECTION('center_axis',(0.,-1.,0.));
#31377=DIRECTION('ref_axis',(0.,0.,-1.));
#31378=DIRECTION('center_axis',(0.822192198445529,0.,-0.569209969005558));
#31379=DIRECTION('ref_axis',(-0.569209969005557,0.,-0.822192198445529));
#31380=DIRECTION('',(0.,1.,0.));
#31381=DIRECTION('',(-0.569209969005557,0.,-0.822192198445529));
#31382=DIRECTION('',(0.,1.,0.));
#31383=DIRECTION('center_axis',(0.,0.,1.));
#31384=DIRECTION('ref_axis',(1.,0.,0.));
#31385=DIRECTION('',(0.,1.,0.));
#31386=DIRECTION('',(1.,0.,0.));
#31387=DIRECTION('center_axis',(-0.835018956019145,0.,0.550221176517859));
#31388=DIRECTION('ref_axis',(0.550221176517859,0.,0.835018956019145));
#31389=DIRECTION('',(0.,1.,0.));
#31390=DIRECTION('',(0.550221176517859,0.,0.835018956019145));
#31391=DIRECTION('',(0.,1.,0.));
#31392=DIRECTION('',(0.,1.,0.));
#31393=DIRECTION('center_axis',(0.836969643122507,0.,0.547249318401935));
#31394=DIRECTION('ref_axis',(0.547249318401935,0.,-0.836969643122507));
#31395=DIRECTION('',(0.,1.,0.));
#31396=DIRECTION('',(0.547249318401935,0.,-0.836969643122507));
#31397=DIRECTION('center_axis',(0.,0.,1.));
#31398=DIRECTION('ref_axis',(1.,0.,0.));
#31399=DIRECTION('',(0.,1.,0.));
#31400=DIRECTION('',(1.,0.,0.));
#31401=DIRECTION('center_axis',(-0.831292792364464,0.,-0.555834771638921));
#31402=DIRECTION('ref_axis',(-0.555834771638921,0.,0.831292792364464));
#31403=DIRECTION('',(0.,1.,0.));
#31404=DIRECTION('',(-0.555834771638921,0.,0.831292792364464));
#31405=DIRECTION('center_axis',(-1.,0.,0.));
#31406=DIRECTION('ref_axis',(0.,0.,1.));
#31407=DIRECTION('',(0.,1.,0.));
#31408=DIRECTION('',(0.,0.,1.));
#31409=DIRECTION('center_axis',(0.,0.,-1.));
#31410=DIRECTION('ref_axis',(-1.,0.,0.));
#31411=DIRECTION('',(0.,1.,0.));
#31412=DIRECTION('',(-1.,0.,0.));
#31413=DIRECTION('center_axis',(1.,0.,0.));
#31414=DIRECTION('ref_axis',(0.,0.,-1.));
#31415=DIRECTION('',(0.,0.,-1.));
#31416=DIRECTION('center_axis',(0.,-1.,0.));
#31417=DIRECTION('ref_axis',(0.,0.,-1.));
#31418=DIRECTION('center_axis',(0.,1.,0.));
#31419=DIRECTION('ref_axis',(1.,0.,0.));
#31420=DIRECTION('',(0.,1.,0.));
#31421=DIRECTION('center_axis',(0.,1.,0.));
#31422=DIRECTION('ref_axis',(1.,0.,0.));
#31423=DIRECTION('',(0.,1.,0.));
#31424=DIRECTION('center_axis',(0.,1.,0.));
#31425=DIRECTION('ref_axis',(1.,0.,0.));
#31426=DIRECTION('',(0.,1.,0.));
#31427=DIRECTION('center_axis',(0.,1.,0.));
#31428=DIRECTION('ref_axis',(1.,0.,0.));
#31429=DIRECTION('',(0.,1.,0.));
#31430=DIRECTION('center_axis',(0.,-1.,0.));
#31431=DIRECTION('ref_axis',(0.,0.,-1.));
#31432=DIRECTION('center_axis',(0.,-1.,0.));
#31433=DIRECTION('ref_axis',(-7.79103876929934E-17,0.,-1.));
#31434=DIRECTION('',(0.,-1.,0.));
#31435=DIRECTION('center_axis',(0.,1.,0.));
#31436=DIRECTION('ref_axis',(0.5,0.,0.866025403784439));
#31437=DIRECTION('',(0.,-1.,0.));
#31438=DIRECTION('center_axis',(-0.866025403784439,0.,0.499999999999999));
#31439=DIRECTION('ref_axis',(-0.499999999999999,0.,-0.866025403784439));
#31440=DIRECTION('',(-0.499999999999999,0.,-0.866025403784439));
#31441=DIRECTION('center_axis',(0.866025403784439,0.,0.5));
#31442=DIRECTION('ref_axis',(-0.5,0.,0.866025403784439));
#31443=DIRECTION('',(-0.5,0.,0.866025403784439));
#31444=DIRECTION('center_axis',(0.,1.,0.));
#31445=DIRECTION('ref_axis',(1.,0.,0.));
#31446=DIRECTION('center_axis',(9.25185853854297E-17,0.,1.));
#31447=DIRECTION('ref_axis',(-1.,0.,9.25185853854297E-17));
#31448=DIRECTION('axis',(0.,0.,1.));
#31449=DIRECTION('refdir',(1.,0.,0.));
#31450=DIRECTION('center_axis',(0.,1.,0.));
#31451=DIRECTION('ref_axis',(0.,0.,1.));
#31452=DIRECTION('center_axis',(0.,1.,0.));
#31453=DIRECTION('ref_axis',(0.,0.,1.));
#31454=DIRECTION('',(8.65956056235486E-17,-0.707106781186554,0.707106781186541));
#31455=DIRECTION('center_axis',(0.,-1.,0.));
#31456=DIRECTION('ref_axis',(0.,0.,1.));
#31457=DIRECTION('center_axis',(0.,1.,0.));
#31458=DIRECTION('ref_axis',(0.,0.,1.));
#31459=DIRECTION('center_axis',(0.,1.,0.));
#31460=DIRECTION('ref_axis',(0.,0.,1.));
#31461=DIRECTION('',(0.,1.,0.));
#31462=DIRECTION('center_axis',(0.,1.,0.));
#31463=DIRECTION('ref_axis',(1.,0.,0.));
#31464=DIRECTION('center_axis',(0.,1.,0.));
#31465=DIRECTION('ref_axis',(1.,0.,-2.96059473233374E-15));
#31466=DIRECTION('',(1.,0.,0.));
#31467=DIRECTION('center_axis',(0.,1.,0.));
#31468=DIRECTION('ref_axis',(-2.96059473233374E-15,0.,-1.));
#31469=DIRECTION('',(0.,0.,-1.));
#31470=DIRECTION('center_axis',(0.,1.,0.));
#31471=DIRECTION('ref_axis',(-1.,0.,2.96059473233374E-15));
#31472=DIRECTION('',(-1.,0.,0.));
#31473=DIRECTION('center_axis',(0.,1.,0.));
#31474=DIRECTION('ref_axis',(2.96059473233374E-15,0.,1.));
#31475=DIRECTION('',(0.,0.,1.));
#31476=DIRECTION('center_axis',(0.,-1.,0.));
#31477=DIRECTION('ref_axis',(0.,0.,1.));
#31478=DIRECTION('',(-8.65956056235486E-17,-0.707106781186554,-0.707106781186541));
#31479=DIRECTION('center_axis',(0.,-1.,0.));
#31480=DIRECTION('ref_axis',(0.,0.,1.));
#31481=DIRECTION('center_axis',(0.,1.,0.));
#31482=DIRECTION('ref_axis',(0.,0.,1.));
#31483=DIRECTION('center_axis',(0.,1.,0.));
#31484=DIRECTION('ref_axis',(1.,0.,0.));
#31485=DIRECTION('center_axis',(0.,0.,1.));
#31486=DIRECTION('ref_axis',(1.,0.,0.));
#31487=DIRECTION('center_axis',(0.,0.,1.));
#31488=DIRECTION('ref_axis',(1.,0.,0.));
#31489=DIRECTION('',(0.707106781186541,8.65956056235486E-17,-0.707106781186554));
#31490=DIRECTION('center_axis',(0.,0.,-1.));
#31491=DIRECTION('ref_axis',(1.,0.,0.));
#31492=DIRECTION('center_axis',(0.,0.,1.));
#31493=DIRECTION('ref_axis',(1.,0.,0.));
#31494=DIRECTION('center_axis',(0.,0.,1.));
#31495=DIRECTION('ref_axis',(-1.,0.,0.));
#31496=DIRECTION('',(1.,0.,0.));
#31497=DIRECTION('center_axis',(0.,0.,1.));
#31498=DIRECTION('ref_axis',(0.,-1.,0.));
#31499=DIRECTION('',(0.,1.,0.));
#31500=DIRECTION('center_axis',(0.,0.,1.));
#31501=DIRECTION('ref_axis',(1.,0.,0.));
#31502=DIRECTION('',(-1.,0.,0.));
#31503=DIRECTION('',(0.,1.,0.));
#31504=DIRECTION('',(-1.,0.,0.));
#31505=DIRECTION('center_axis',(0.,0.,1.));
#31506=DIRECTION('ref_axis',(0.,1.,0.));
#31507=DIRECTION('',(0.,-1.,0.));
#31508=DIRECTION('center_axis',(0.,0.,1.));
#31509=DIRECTION('ref_axis',(1.,0.,0.));
#31510=DIRECTION('',(1.,0.,0.));
#31511=DIRECTION('center_axis',(0.,0.,1.));
#31512=DIRECTION('ref_axis',(-1.,0.,0.));
#31513=DIRECTION('',(0.,-1.,0.));
#31514=DIRECTION('center_axis',(0.,0.,1.));
#31515=DIRECTION('ref_axis',(4.44089209850064E-15,1.,0.));
#31516=DIRECTION('',(-1.,0.,0.));
#31517=DIRECTION('center_axis',(0.,0.,1.));
#31518=DIRECTION('ref_axis',(1.,0.,0.));
#31519=DIRECTION('',(0.,1.,0.));
#31520=DIRECTION('center_axis',(0.,0.,1.));
#31521=DIRECTION('ref_axis',(-4.44089209850064E-15,-1.,0.));
#31522=DIRECTION('center_axis',(0.,0.,-1.));
#31523=DIRECTION('ref_axis',(1.,0.,0.));
#31524=DIRECTION('',(0.,0.,-1.));
#31525=DIRECTION('center_axis',(0.,0.,1.));
#31526=DIRECTION('ref_axis',(1.,0.,0.));
#31527=DIRECTION('center_axis',(0.,0.,1.));
#31528=DIRECTION('ref_axis',(1.,0.,0.));
#31529=DIRECTION('',(0.707106781186541,8.65956056235486E-17,-0.707106781186554));
#31530=DIRECTION('center_axis',(0.,0.,-1.));
#31531=DIRECTION('ref_axis',(1.,0.,0.));
#31532=DIRECTION('center_axis',(0.,0.,-1.));
#31533=DIRECTION('ref_axis',(1.,0.,0.));
#31534=DIRECTION('',(0.,0.,-1.));
#31535=DIRECTION('center_axis',(0.,0.,1.));
#31536=DIRECTION('ref_axis',(1.,0.,0.));
#31537=DIRECTION('center_axis',(1.,0.,0.));
#31538=DIRECTION('ref_axis',(0.,0.,-1.));
#31539=DIRECTION('',(-0.707106781186546,-0.127511058902472,-0.695514866740871));
#31540=DIRECTION('center_axis',(-1.,0.,0.));
#31541=DIRECTION('ref_axis',(0.,0.,-1.));
#31542=DIRECTION('',(0.707106781186546,-0.127511058902472,0.695514866740871));
#31543=DIRECTION('center_axis',(1.,0.,0.));
#31544=DIRECTION('ref_axis',(0.,0.,-1.));
#31545=DIRECTION('center_axis',(-1.,0.,0.));
#31546=DIRECTION('ref_axis',(0.,0.,1.));
#31547=DIRECTION('',(0.,1.,0.));
#31548=DIRECTION('center_axis',(1.,0.,0.));
#31549=DIRECTION('ref_axis',(0.,0.,-1.));
#31550=DIRECTION('',(0.,1.,0.));
#31551=DIRECTION('',(0.,1.,0.));
#31552=DIRECTION('center_axis',(1.,0.,0.));
#31553=DIRECTION('ref_axis',(0.,0.,-1.));
#31554=DIRECTION('',(0.,1.,0.));
#31555=DIRECTION('center_axis',(1.,0.,0.));
#31556=DIRECTION('ref_axis',(0.,0.,-1.));
#31557=DIRECTION('',(0.,1.,0.));
#31558=DIRECTION('',(0.,0.,1.));
#31559=DIRECTION('',(0.,0.,1.));
#31560=DIRECTION('',(0.,1.,0.));
#31561=DIRECTION('',(0.,0.,1.));
#31562=DIRECTION('center_axis',(1.,0.,0.));
#31563=DIRECTION('ref_axis',(0.,0.707106781186548,-0.707106781186547));
#31564=DIRECTION('',(0.,1.,0.));
#31565=DIRECTION('center_axis',(1.,0.,0.));
#31566=DIRECTION('ref_axis',(0.,-0.707106781186547,-0.707106781186548));
#31567=DIRECTION('',(0.,0.,-1.));
#31568=DIRECTION('center_axis',(1.,0.,0.));
#31569=DIRECTION('ref_axis',(0.,-0.707106781186548,0.707106781186548));
#31570=DIRECTION('',(0.,-1.,0.));
#31571=DIRECTION('center_axis',(1.,0.,0.));
#31572=DIRECTION('ref_axis',(0.,0.707106781186548,0.707106781186547));
#31573=DIRECTION('center_axis',(1.,0.,0.));
#31574=DIRECTION('ref_axis',(0.,0.,-1.));
#31575=DIRECTION('center_axis',(1.,0.,0.));
#31576=DIRECTION('ref_axis',(0.,0.,-1.));
#31577=DIRECTION('',(1.,0.,0.));
#31578=DIRECTION('center_axis',(1.,0.,0.));
#31579=DIRECTION('ref_axis',(0.,-1.22464679914735E-16,1.));
#31580=DIRECTION('',(-0.707106781186544,0.127511058902497,0.695514866740869));
#31581=DIRECTION('center_axis',(-1.,0.,0.));
#31582=DIRECTION('ref_axis',(0.,0.,-1.));
#31583=DIRECTION('center_axis',(-1.,0.,0.));
#31584=DIRECTION('ref_axis',(0.,0.,-1.));
#31585=DIRECTION('',(0.707106781186544,0.127511058902497,-0.695514866740869));
#31586=DIRECTION('center_axis',(0.,1.,0.));
#31587=DIRECTION('ref_axis',(-2.96059473233374E-15,0.,-1.));
#31588=DIRECTION('',(0.,1.,0.));
#31589=DIRECTION('center_axis',(0.,1.,0.));
#31590=DIRECTION('ref_axis',(-2.96059473233374E-15,0.,-1.));
#31591=DIRECTION('center_axis',(1.,0.,0.));
#31592=DIRECTION('ref_axis',(0.,0.,-1.));
#31593=DIRECTION('center_axis',(1.,0.,0.));
#31594=DIRECTION('ref_axis',(0.,0.,-1.));
#31595=DIRECTION('',(1.,0.,0.));
#31596=DIRECTION('center_axis',(1.,0.,0.));
#31597=DIRECTION('ref_axis',(0.,0.,-1.));
#31598=DIRECTION('',(-0.707106781186544,-0.127511058902497,-0.695514866740869));
#31599=DIRECTION('center_axis',(-1.,0.,0.));
#31600=DIRECTION('ref_axis',(0.,0.,-1.));
#31601=DIRECTION('',(0.707106781186544,-0.127511058902497,0.695514866740869));
#31602=DIRECTION('center_axis',(1.,0.,0.));
#31603=DIRECTION('ref_axis',(0.,0.,-1.));
#31604=DIRECTION('center_axis',(1.,0.,0.));
#31605=DIRECTION('ref_axis',(0.,0.,-1.));
#31606=DIRECTION('',(1.,0.,0.));
#31607=DIRECTION('center_axis',(1.,0.,0.));
#31608=DIRECTION('ref_axis',(0.,-1.22464679914735E-16,1.));
#31609=DIRECTION('',(-0.707106781186546,0.127511058902472,0.695514866740871));
#31610=DIRECTION('center_axis',(-1.,0.,0.));
#31611=DIRECTION('ref_axis',(0.,0.,-1.));
#31612=DIRECTION('center_axis',(-1.,0.,0.));
#31613=DIRECTION('ref_axis',(0.,0.,-1.));
#31614=DIRECTION('',(0.707106781186546,0.127511058902472,-0.695514866740871));
#31615=DIRECTION('center_axis',(1.,0.,0.));
#31616=DIRECTION('ref_axis',(0.,0.,-1.));
#31617=DIRECTION('center_axis',(1.,0.,0.));
#31618=DIRECTION('ref_axis',(0.,0.,-1.));
#31619=DIRECTION('',(1.,0.,0.));
#31620=DIRECTION('center_axis',(-1.,0.,0.));
#31621=DIRECTION('ref_axis',(0.,0.,-1.));
#31622=DIRECTION('center_axis',(-1.,0.,0.));
#31623=DIRECTION('ref_axis',(0.,0.,-1.));
#31624=DIRECTION('',(0.707106781186548,-8.65956056235493E-17,-0.707106781186548));
#31625=DIRECTION('center_axis',(-1.,0.,0.));
#31626=DIRECTION('ref_axis',(0.,0.,1.));
#31627=DIRECTION('',(0.,0.,-1.));
#31628=DIRECTION('',(0.,1.,0.));
#31629=DIRECTION('',(0.,0.,-1.));
#31630=DIRECTION('',(0.,1.,0.));
#31631=DIRECTION('center_axis',(-1.,0.,0.));
#31632=DIRECTION('ref_axis',(0.,0.,-1.));
#31633=DIRECTION('center_axis',(-1.,0.,0.));
#31634=DIRECTION('ref_axis',(0.,0.,-1.));
#31635=DIRECTION('',(0.,0.,-1.));
#31636=DIRECTION('center_axis',(-1.,0.,0.));
#31637=DIRECTION('ref_axis',(0.,0.707106781186548,0.707106781186547));
#31638=DIRECTION('',(0.,1.,0.));
#31639=DIRECTION('center_axis',(-1.,0.,0.));
#31640=DIRECTION('ref_axis',(0.,-0.707106781186548,0.707106781186548));
#31641=DIRECTION('',(0.,0.,1.));
#31642=DIRECTION('center_axis',(-1.,0.,0.));
#31643=DIRECTION('ref_axis',(0.,-0.707106781186547,-0.707106781186548));
#31644=DIRECTION('',(0.,-1.,0.));
#31645=DIRECTION('center_axis',(-1.,0.,0.));
#31646=DIRECTION('ref_axis',(0.,0.707106781186548,-0.707106781186547));
#31647=DIRECTION('center_axis',(-1.,0.,0.));
#31648=DIRECTION('ref_axis',(0.,0.,-1.));
#31649=DIRECTION('center_axis',(-1.,0.,0.));
#31650=DIRECTION('ref_axis',(0.,0.,-1.));
#31651=DIRECTION('',(0.707106781186548,-8.65956056235493E-17,-0.707106781186548));
#31652=DIRECTION('center_axis',(-1.,0.,0.));
#31653=DIRECTION('ref_axis',(0.,0.,-1.));
#31654=DIRECTION('',(0.707106781186548,-8.65956056235493E-17,-0.707106781186548));
#31655=DIRECTION('center_axis',(-1.,0.,0.));
#31656=DIRECTION('ref_axis',(0.,0.,-1.));
#31657=DIRECTION('',(0.707106781186548,-8.65956056235493E-17,-0.707106781186548));
#31658=DIRECTION('center_axis',(0.,1.,0.));
#31659=DIRECTION('ref_axis',(1.,0.,0.));
#31660=DIRECTION('center_axis',(0.,1.,0.));
#31661=DIRECTION('ref_axis',(1.,0.,0.));
#31662=DIRECTION('',(0.707106781186541,-0.707106781186554,-8.65956056235486E-17));
#31663=DIRECTION('center_axis',(0.,-1.,0.));
#31664=DIRECTION('ref_axis',(1.,0.,0.));
#31665=DIRECTION('center_axis',(0.,1.,0.));
#31666=DIRECTION('ref_axis',(0.,0.,1.));
#31667=DIRECTION('center_axis',(0.,-1.,0.));
#31668=DIRECTION('ref_axis',(6.12323399573677E-17,0.,-1.));
#31669=DIRECTION('center_axis',(0.,1.,0.));
#31670=DIRECTION('ref_axis',(1.,0.,0.));
#31671=DIRECTION('center_axis',(0.,1.,0.));
#31672=DIRECTION('ref_axis',(1.,0.,0.));
#31673=DIRECTION('center_axis',(0.,1.,0.));
#31674=DIRECTION('ref_axis',(0.,0.,1.));
#31675=DIRECTION('center_axis',(0.,1.,0.));
#31676=DIRECTION('ref_axis',(1.,0.,0.));
#31677=DIRECTION('center_axis',(0.,1.,0.));
#31678=DIRECTION('ref_axis',(1.,0.,0.));
#31679=DIRECTION('center_axis',(0.,1.,0.));
#31680=DIRECTION('ref_axis',(1.,0.,0.));
#31681=DIRECTION('',(0.,1.,0.));
#31682=DIRECTION('center_axis',(0.,1.,0.));
#31683=DIRECTION('ref_axis',(1.,0.,0.));
#31684=DIRECTION('',(0.707106781186541,-0.707106781186554,-8.65956056235486E-17));
#31685=DIRECTION('center_axis',(0.,-1.,0.));
#31686=DIRECTION('ref_axis',(1.,0.,0.));
#31687=DIRECTION('center_axis',(0.,1.,0.));
#31688=DIRECTION('ref_axis',(1.,0.,0.));
#31689=DIRECTION('center_axis',(0.,1.,0.));
#31690=DIRECTION('ref_axis',(1.,0.,0.));
#31691=DIRECTION('',(0.,1.,0.));
#31692=DIRECTION('center_axis',(0.,1.,0.));
#31693=DIRECTION('ref_axis',(1.,0.,0.));
#31694=DIRECTION('',(0.707106781186547,-0.707106781186547,-8.65956056235493E-17));
#31695=DIRECTION('center_axis',(0.,-1.,0.));
#31696=DIRECTION('ref_axis',(1.,0.,0.));
#31697=DIRECTION('center_axis',(0.,1.,0.));
#31698=DIRECTION('ref_axis',(1.,0.,0.));
#31699=DIRECTION('center_axis',(0.,1.,0.));
#31700=DIRECTION('ref_axis',(1.,0.,0.));
#31701=DIRECTION('',(0.,1.,0.));
#31702=DIRECTION('center_axis',(0.,1.,0.));
#31703=DIRECTION('ref_axis',(1.,0.,0.));
#31704=DIRECTION('',(0.707106781186547,-0.707106781186547,-8.65956056235493E-17));
#31705=DIRECTION('center_axis',(0.,-1.,0.));
#31706=DIRECTION('ref_axis',(1.,0.,0.));
#31707=DIRECTION('center_axis',(0.,1.,0.));
#31708=DIRECTION('ref_axis',(1.,0.,0.));
#31709=DIRECTION('center_axis',(0.,1.,0.));
#31710=DIRECTION('ref_axis',(1.,0.,0.));
#31711=DIRECTION('',(0.,1.,0.));
#31712=DIRECTION('center_axis',(0.,0.,-1.));
#31713=DIRECTION('ref_axis',(1.,0.,0.));
#31714=DIRECTION('center_axis',(0.,0.,-1.));
#31715=DIRECTION('ref_axis',(1.,0.,0.));
#31716=DIRECTION('',(0.707106781186541,-8.65956056235486E-17,0.707106781186554));
#31717=DIRECTION('center_axis',(0.,0.,1.));
#31718=DIRECTION('ref_axis',(1.,0.,0.));
#31719=DIRECTION('',(0.,-1.,0.));
#31720=DIRECTION('center_axis',(0.,0.,1.));
#31721=DIRECTION('ref_axis',(-0.707106781186548,0.707106781186548,0.));
#31722=DIRECTION('',(-1.,0.,0.));
#31723=DIRECTION('center_axis',(0.,0.,1.));
#31724=DIRECTION('ref_axis',(0.707106781186549,0.707106781186547,0.));
#31725=DIRECTION('',(0.,1.,0.));
#31726=DIRECTION('center_axis',(0.,0.,1.));
#31727=DIRECTION('ref_axis',(0.707106781186548,-0.707106781186548,0.));
#31728=DIRECTION('',(1.,0.,0.));
#31729=DIRECTION('center_axis',(0.,0.,1.));
#31730=DIRECTION('ref_axis',(-0.707106781186549,-0.707106781186547,0.));
#31731=DIRECTION('center_axis',(0.,0.,-1.));
#31732=DIRECTION('ref_axis',(1.,0.,0.));
#31733=DIRECTION('center_axis',(0.,0.,-1.));
#31734=DIRECTION('ref_axis',(1.,0.,0.));
#31735=DIRECTION('',(0.707106781186541,-8.65956056235486E-17,0.707106781186554));
#31736=DIRECTION('center_axis',(0.,-1.,0.));
#31737=DIRECTION('ref_axis',(0.,0.,1.));
#31738=DIRECTION('center_axis',(0.,1.,0.));
#31739=DIRECTION('ref_axis',(0.,0.,1.));
#31740=DIRECTION('center_axis',(1.,0.,-1.22464679914735E-16));
#31741=DIRECTION('ref_axis',(-1.22464679914735E-16,0.,-1.));
#31742=DIRECTION('center_axis',(0.,-1.,0.));
#31743=DIRECTION('ref_axis',(0.,0.,1.));
#31744=DIRECTION('center_axis',(0.,1.,0.));
#31745=DIRECTION('ref_axis',(0.,0.,1.));
#31746=DIRECTION('',(0.,-1.,0.));
#31747=DIRECTION('center_axis',(0.,-1.,0.));
#31748=DIRECTION('ref_axis',(1.22464679914735E-16,0.,1.));
#31749=DIRECTION('center_axis',(0.,1.,0.));
#31750=DIRECTION('ref_axis',(0.,0.,1.));
#31751=DIRECTION('center_axis',(0.,-1.,0.));
#31752=DIRECTION('ref_axis',(1.,0.,0.));
#31753=DIRECTION('center_axis',(0.,-1.,0.));
#31754=DIRECTION('ref_axis',(1.,0.,0.));
#31755=DIRECTION('center_axis',(0.,-1.,0.));
#31756=DIRECTION('ref_axis',(1.,0.,0.));
#31757=DIRECTION('center_axis',(0.,-1.,0.));
#31758=DIRECTION('ref_axis',(1.,0.,0.));
#31759=DIRECTION('center_axis',(0.,1.,0.));
#31760=DIRECTION('ref_axis',(1.,0.,0.));
#31761=DIRECTION('center_axis',(0.,1.,0.));
#31762=DIRECTION('ref_axis',(1.22464679914735E-16,0.,1.));
#31763=DIRECTION('center_axis',(-1.,0.,0.));
#31764=DIRECTION('ref_axis',(0.,0.,-1.));
#31765=DIRECTION('center_axis',(0.,1.,0.));
#31766=DIRECTION('ref_axis',(1.22464679914735E-16,0.,1.));
#31767=DIRECTION('center_axis',(0.,-1.,0.));
#31768=DIRECTION('ref_axis',(0.,0.,-1.));
#31769=DIRECTION('center_axis',(0.,1.,0.));
#31770=DIRECTION('ref_axis',(1.,0.,0.));
#31771=DIRECTION('center_axis',(0.,1.,0.));
#31772=DIRECTION('ref_axis',(1.,0.,0.));
#31773=DIRECTION('center_axis',(0.,1.,0.));
#31774=DIRECTION('ref_axis',(1.,0.,0.));
#31775=DIRECTION('center_axis',(0.,1.,0.));
#31776=DIRECTION('ref_axis',(1.,0.,0.));
#31777=DIRECTION('center_axis',(0.,1.,0.));
#31778=DIRECTION('ref_axis',(1.,0.,0.));
#31779=DIRECTION('center_axis',(0.,1.,0.));
#31780=DIRECTION('ref_axis',(0.,0.,1.));
#31781=DIRECTION('center_axis',(0.,-1.,0.));
#31782=DIRECTION('ref_axis',(-3.06161699786838E-17,0.,-1.));
#31783=DIRECTION('center_axis',(-1.,0.,1.22464679914735E-16));
#31784=DIRECTION('ref_axis',(-1.22464679914735E-16,0.,-1.));
#31785=DIRECTION('center_axis',(0.,1.,0.));
#31786=DIRECTION('ref_axis',(-3.06161699786838E-17,0.,-1.));
#31787=DIRECTION('center_axis',(0.,1.,0.));
#31788=DIRECTION('ref_axis',(0.,0.,1.));
#31789=DIRECTION('',(1.20086498579063E-16,-0.196116135138187,0.98058067569092));
#31790=DIRECTION('center_axis',(0.,-1.,0.));
#31791=DIRECTION('ref_axis',(-3.06161699786838E-17,0.,-1.));
#31792=DIRECTION('center_axis',(0.,1.,0.));
#31793=DIRECTION('ref_axis',(0.,0.,1.));
#31794=DIRECTION('center_axis',(0.,1.,0.));
#31795=DIRECTION('ref_axis',(1.,0.,0.));
#31796=DIRECTION('',(8.65956056235501E-17,-0.707106781186541,0.707106781186554));
#31797=DIRECTION('center_axis',(0.,1.,0.));
#31798=DIRECTION('ref_axis',(0.,0.,1.));
#31799=DIRECTION('center_axis',(-1.,0.,1.22464679914735E-16));
#31800=DIRECTION('ref_axis',(-1.22464679914735E-16,0.,-1.));
#31801=DIRECTION('center_axis',(0.,1.,0.));
#31802=DIRECTION('ref_axis',(-3.06161699786838E-17,0.,-1.));
#31803=DIRECTION('center_axis',(0.,1.,0.));
#31804=DIRECTION('ref_axis',(0.,0.,1.));
#31805=DIRECTION('',(1.2221746482687E-16,-0.0635079031754479,0.997981335614178));
#31806=DIRECTION('center_axis',(0.,1.,0.));
#31807=DIRECTION('ref_axis',(0.,0.,1.));
#31808=DIRECTION('center_axis',(0.,-1.,0.));
#31809=DIRECTION('ref_axis',(-1.,0.,-1.11022302462516E-16));
#31810=DIRECTION('center_axis',(0.,-1.,0.));
#31811=DIRECTION('ref_axis',(9.18485099360515E-17,0.,1.));
#31812=DIRECTION('center_axis',(0.,-1.,0.));
#31813=DIRECTION('ref_axis',(1.,0.,0.));
#31814=DIRECTION('center_axis',(0.,1.,0.));
#31815=DIRECTION('ref_axis',(0.,0.,1.));
#31816=DIRECTION('center_axis',(0.,1.,0.));
#31817=DIRECTION('ref_axis',(0.,0.,1.));
#31818=DIRECTION('center_axis',(0.,1.,0.));
#31819=DIRECTION('ref_axis',(1.,0.,0.));
#31820=DIRECTION('center_axis',(0.,-1.,0.));
#31821=DIRECTION('ref_axis',(0.,0.,-1.));
#31822=DIRECTION('',(0.,0.,1.));
#31823=DIRECTION('center_axis',(0.,1.,0.));
#31824=DIRECTION('ref_axis',(0.,0.,1.));
#31825=DIRECTION('center_axis',(0.,1.,0.));
#31826=DIRECTION('ref_axis',(6.12323399573677E-17,0.,1.));
#31827=DIRECTION('center_axis',(0.,-1.,0.));
#31828=DIRECTION('ref_axis',(0.,0.,-1.));
#31829=DIRECTION('',(-1.,0.,0.));
#31830=DIRECTION('center_axis',(0.,1.,0.));
#31831=DIRECTION('ref_axis',(0.,0.,1.));
#31832=DIRECTION('center_axis',(0.,1.,0.));
#31833=DIRECTION('ref_axis',(-1.,0.,-1.22464679914735E-16));
#31834=DIRECTION('center_axis',(0.,-1.,0.));
#31835=DIRECTION('ref_axis',(0.,0.,-1.));
#31836=DIRECTION('center_axis',(0.,-1.,0.));
#31837=DIRECTION('ref_axis',(-0.707106781186551,0.,-0.707106781186544));
#31838=DIRECTION('center_axis',(0.,-1.,0.));
#31839=DIRECTION('ref_axis',(-1.,0.,0.));
#31840=DIRECTION('center_axis',(0.,1.,0.));
#31841=DIRECTION('ref_axis',(0.,0.,-1.));
#31842=DIRECTION('',(0.,1.,0.));
#31843=DIRECTION('center_axis',(-1.,0.,0.));
#31844=DIRECTION('ref_axis',(0.,0.,-1.));
#31845=DIRECTION('center_axis',(0.,0.,-1.));
#31846=DIRECTION('ref_axis',(-0.707106781186549,-0.707106781186546,0.));
#31847=DIRECTION('center_axis',(1.,0.,0.));
#31848=DIRECTION('ref_axis',(0.,-0.707106781186554,-0.707106781186541));
#31849=DIRECTION('center_axis',(-1.,-4.44089209850056E-15,0.));
#31850=DIRECTION('ref_axis',(0.,0.,-1.));
#31851=DIRECTION('',(-1.,0.,0.));
#31852=DIRECTION('center_axis',(0.,-1.,0.));
#31853=DIRECTION('ref_axis',(0.,0.,-1.));
#31854=DIRECTION('center_axis',(0.,0.,-1.));
#31855=DIRECTION('ref_axis',(0.707106781186548,-0.707106781186548,0.));
#31856=DIRECTION('center_axis',(0.,1.,0.));
#31857=DIRECTION('ref_axis',(0.707106781186551,0.,-0.707106781186544));
#31858=DIRECTION('center_axis',(0.,-1.,0.));
#31859=DIRECTION('ref_axis',(0.,0.,-1.));
#31860=DIRECTION('',(0.,-1.,0.));
#31861=DIRECTION('center_axis',(1.,0.,0.));
#31862=DIRECTION('ref_axis',(0.,0.,-1.));
#31863=DIRECTION('center_axis',(0.,0.,-1.));
#31864=DIRECTION('ref_axis',(0.707106781186549,0.707106781186546,0.));
#31865=DIRECTION('center_axis',(-1.,0.,0.));
#31866=DIRECTION('ref_axis',(0.,0.707106781186554,-0.707106781186541));
#31867=DIRECTION('center_axis',(1.,4.44089209850056E-15,0.));
#31868=DIRECTION('ref_axis',(0.,0.,-1.));
#31869=DIRECTION('',(1.,0.,0.));
#31870=DIRECTION('center_axis',(0.,0.,-1.));
#31871=DIRECTION('ref_axis',(-0.707106781186548,0.707106781186548,0.));
#31872=DIRECTION('center_axis',(0.,0.,1.));
#31873=DIRECTION('ref_axis',(1.,0.,0.));
#31874=DIRECTION('',(0.,0.,1.));
#31875=DIRECTION('',(0.,0.,1.));
#31876=DIRECTION('center_axis',(0.,1.,0.));
#31877=DIRECTION('ref_axis',(-1.,0.,0.));
#31878=DIRECTION('',(0.,0.,1.));
#31879=DIRECTION('center_axis',(0.,0.,1.));
#31880=DIRECTION('ref_axis',(0.,1.,0.));
#31881=DIRECTION('',(0.,0.,1.));
#31882=DIRECTION('center_axis',(-1.,0.,0.));
#31883=DIRECTION('ref_axis',(0.,-1.,0.));
#31884=DIRECTION('',(0.,0.,1.));
#31885=DIRECTION('center_axis',(0.,1.,0.));
#31886=DIRECTION('ref_axis',(0.,0.,1.));
#31887=DIRECTION('center_axis',(-1.,0.,1.22464679914735E-16));
#31888=DIRECTION('ref_axis',(-1.22464679914735E-16,0.,-1.));
#31889=DIRECTION('center_axis',(0.,1.,0.));
#31890=DIRECTION('ref_axis',(6.12323399573677E-17,0.,-1.));
#31891=DIRECTION('center_axis',(0.,1.,0.));
#31892=DIRECTION('ref_axis',(0.,0.,1.));
#31893=DIRECTION('',(0.,-1.,0.));
#31894=DIRECTION('',(0.,1.,0.));
#31895=DIRECTION('center_axis',(0.,1.,0.));
#31896=DIRECTION('ref_axis',(0.,0.,1.));
#31897=DIRECTION('center_axis',(0.,-1.,0.));
#31898=DIRECTION('ref_axis',(0.,0.,1.));
#31899=DIRECTION('center_axis',(-1.,0.,1.22464679914735E-16));
#31900=DIRECTION('ref_axis',(-1.22464679914735E-16,0.,-1.));
#31901=DIRECTION('center_axis',(0.,1.,0.));
#31902=DIRECTION('ref_axis',(0.,0.,1.));
#31903=DIRECTION('center_axis',(0.,-1.,0.));
#31904=DIRECTION('ref_axis',(0.,0.,1.));
#31905=DIRECTION('center_axis',(0.,-1.,0.));
#31906=DIRECTION('ref_axis',(0.,0.,1.));
#31907=DIRECTION('center_axis',(0.,-1.,0.));
#31908=DIRECTION('ref_axis',(0.,0.,1.));
#31909=DIRECTION('center_axis',(0.,1.,0.));
#31910=DIRECTION('ref_axis',(1.,0.,0.));
#31911=DIRECTION('',(0.,0.,-1.));
#31912=DIRECTION('center_axis',(0.,1.,0.));
#31913=DIRECTION('ref_axis',(2.96059473233374E-15,0.,1.));
#31914=DIRECTION('',(1.,0.,0.));
#31915=DIRECTION('center_axis',(0.,1.,0.));
#31916=DIRECTION('ref_axis',(1.,0.,0.));
#31917=DIRECTION('',(-1.,0.,0.));
#31918=DIRECTION('center_axis',(0.,1.,0.));
#31919=DIRECTION('ref_axis',(1.,0.,-2.96059473233374E-15));
#31920=DIRECTION('',(0.,0.,-1.));
#31921=DIRECTION('center_axis',(0.,1.,0.));
#31922=DIRECTION('ref_axis',(1.,0.,0.));
#31923=DIRECTION('',(-1.,0.,0.));
#31924=DIRECTION('center_axis',(0.,1.,0.));
#31925=DIRECTION('ref_axis',(1.,0.,0.));
#31926=DIRECTION('',(1.,0.,0.));
#31927=DIRECTION('center_axis',(0.,1.,0.));
#31928=DIRECTION('ref_axis',(-1.,0.,2.96059473233374E-15));
#31929=DIRECTION('center_axis',(0.,1.,0.));
#31930=DIRECTION('ref_axis',(0.,0.,1.));
#31931=DIRECTION('center_axis',(0.,-1.,0.));
#31932=DIRECTION('ref_axis',(0.,0.,1.));
#31933=DIRECTION('',(0.,-1.,0.));
#31934=DIRECTION('center_axis',(0.,-1.,0.));
#31935=DIRECTION('ref_axis',(0.,0.,-1.));
#31936=DIRECTION('center_axis',(-1.,0.,-1.22464679914735E-16));
#31937=DIRECTION('ref_axis',(-1.22464679914735E-16,0.,1.));
#31938=DIRECTION('center_axis',(0.,-1.,0.));
#31939=DIRECTION('ref_axis',(0.,0.,1.));
#31940=DIRECTION('center_axis',(0.,-1.,0.));
#31941=DIRECTION('ref_axis',(0.,0.,1.));
#31942=DIRECTION('center_axis',(0.,1.,0.));
#31943=DIRECTION('ref_axis',(0.,0.,1.));
#31944=DIRECTION('center_axis',(0.,1.,0.));
#31945=DIRECTION('ref_axis',(1.,0.,0.));
#31946=DIRECTION('',(0.,1.,0.));
#31947=DIRECTION('center_axis',(0.,1.,0.));
#31948=DIRECTION('ref_axis',(0.,0.,1.));
#31949=DIRECTION('center_axis',(-1.,0.,1.22464679914735E-16));
#31950=DIRECTION('ref_axis',(-1.22464679914735E-16,0.,-1.));
#31951=DIRECTION('center_axis',(0.,1.,0.));
#31952=DIRECTION('ref_axis',(0.,0.,1.));
#31953=DIRECTION('center_axis',(0.,-1.,0.));
#31954=DIRECTION('ref_axis',(0.,0.,-1.));
#31955=DIRECTION('center_axis',(0.,1.,0.));
#31956=DIRECTION('ref_axis',(0.707106781186546,0.,-0.707106781186549));
#31957=DIRECTION('center_axis',(0.,1.,0.));
#31958=DIRECTION('ref_axis',(1.,0.,0.));
#31959=DIRECTION('',(0.,1.,0.));
#31960=DIRECTION('center_axis',(0.,-1.,0.));
#31961=DIRECTION('ref_axis',(0.,0.,-1.));
#31962=DIRECTION('',(0.,-1.,0.));
#31963=DIRECTION('center_axis',(-1.,0.,0.));
#31964=DIRECTION('ref_axis',(0.,0.,1.));
#31965=DIRECTION('center_axis',(0.,2.22044604925032E-15,1.));
#31966=DIRECTION('ref_axis',(0.,-1.,2.22044604925032E-15));
#31967=DIRECTION('center_axis',(1.,0.,0.));
#31968=DIRECTION('ref_axis',(0.,0.707106781186548,0.707106781186547));
#31969=DIRECTION('center_axis',(-1.,0.,0.));
#31970=DIRECTION('ref_axis',(0.,0.707106781186548,0.707106781186547));
#31971=DIRECTION('center_axis',(0.,0.,-1.));
#31972=DIRECTION('ref_axis',(0.707106781186541,-0.707106781186554,0.));
#31973=DIRECTION('center_axis',(0.,-2.22044604925032E-15,1.));
#31974=DIRECTION('ref_axis',(0.,-1.,-2.22044604925032E-15));
#31975=DIRECTION('',(0.,0.,1.));
#31976=DIRECTION('',(0.,0.,-1.));
#31977=DIRECTION('center_axis',(-1.,0.,0.));
#31978=DIRECTION('ref_axis',(0.,0.,1.));
#31979=DIRECTION('center_axis',(0.,1.,0.));
#31980=DIRECTION('ref_axis',(0.,0.,1.));
#31981=DIRECTION('center_axis',(1.,0.,0.));
#31982=DIRECTION('ref_axis',(0.,0.707106781186548,-0.707106781186547));
#31983=DIRECTION('center_axis',(-1.,0.,0.));
#31984=DIRECTION('ref_axis',(0.,0.707106781186548,-0.707106781186547));
#31985=DIRECTION('center_axis',(0.,-1.,0.));
#31986=DIRECTION('ref_axis',(0.707106781186546,0.,0.707106781186549));
#31987=DIRECTION('center_axis',(0.,1.,0.));
#31988=DIRECTION('ref_axis',(0.,0.,1.));
#31989=DIRECTION('',(0.,1.,0.));
#31990=DIRECTION('',(0.,-1.,0.));
#31991=DIRECTION('center_axis',(-1.,0.,0.));
#31992=DIRECTION('ref_axis',(0.,0.,1.));
#31993=DIRECTION('center_axis',(0.,2.22044604925032E-15,-1.));
#31994=DIRECTION('ref_axis',(0.,1.,2.22044604925032E-15));
#31995=DIRECTION('center_axis',(1.,0.,0.));
#31996=DIRECTION('ref_axis',(0.,-0.707106781186547,-0.707106781186548));
#31997=DIRECTION('center_axis',(-1.,0.,0.));
#31998=DIRECTION('ref_axis',(0.,-0.707106781186547,-0.707106781186548));
#31999=DIRECTION('center_axis',(0.,0.,1.));
#32000=DIRECTION('ref_axis',(0.707106781186548,0.707106781186548,0.));
#32001=DIRECTION('center_axis',(0.,0.,-1.));
#32002=DIRECTION('ref_axis',(0.,1.,0.));
#32003=DIRECTION('',(0.,0.,-1.));
#32004=DIRECTION('',(0.,0.,1.));
#32005=DIRECTION('center_axis',(-1.,0.,0.));
#32006=DIRECTION('ref_axis',(0.,0.,1.));
#32007=DIRECTION('center_axis',(1.,0.,0.));
#32008=DIRECTION('ref_axis',(0.,-0.707106781186548,0.707106781186548));
#32009=DIRECTION('center_axis',(-1.,0.,0.));
#32010=DIRECTION('ref_axis',(0.,-0.707106781186548,0.707106781186548));
#32011=DIRECTION('center_axis',(-1.,0.,0.));
#32012=DIRECTION('ref_axis',(0.,0.,-1.));
#32013=DIRECTION('',(-1.,0.,0.));
#32014=DIRECTION('center_axis',(1.,0.,0.));
#32015=DIRECTION('ref_axis',(0.,0.707106781186548,-0.707106781186547));
#32016=DIRECTION('',(-1.,0.,0.));
#32017=DIRECTION('center_axis',(0.,1.,0.));
#32018=DIRECTION('ref_axis',(0.,0.,-1.));
#32019=DIRECTION('',(-1.,0.,0.));
#32020=DIRECTION('',(0.,0.,1.));
#32021=DIRECTION('center_axis',(-1.,0.,0.));
#32022=DIRECTION('ref_axis',(0.,1.,-2.22044604925032E-15));
#32023=DIRECTION('',(-1.,0.,0.));
#32024=DIRECTION('center_axis',(1.,0.,0.));
#32025=DIRECTION('ref_axis',(0.,0.707106781186548,0.707106781186547));
#32026=DIRECTION('center_axis',(0.,0.,1.));
#32027=DIRECTION('ref_axis',(0.,1.,0.));
#32028=DIRECTION('',(-1.,0.,0.));
#32029=DIRECTION('',(0.,-1.,0.));
#32030=DIRECTION('center_axis',(1.,0.,0.));
#32031=DIRECTION('ref_axis',(0.,0.,-1.));
#32032=DIRECTION('',(0.,0.,1.));
#32033=DIRECTION('',(0.,1.,0.));
#32034=DIRECTION('',(0.,1.,0.));
#32035=DIRECTION('center_axis',(0.,-1.,0.));
#32036=DIRECTION('ref_axis',(-0.707106781186546,0.,-0.707106781186549));
#32037=DIRECTION('center_axis',(0.,-1.,0.));
#32038=DIRECTION('ref_axis',(-1.,0.,0.));
#32039=DIRECTION('center_axis',(0.,1.,0.));
#32040=DIRECTION('ref_axis',(0.,0.,-1.));
#32041=DIRECTION('',(0.,1.,0.));
#32042=DIRECTION('center_axis',(1.,0.,0.));
#32043=DIRECTION('ref_axis',(0.,0.,-1.));
#32044=DIRECTION('center_axis',(0.,2.22044604925032E-15,1.));
#32045=DIRECTION('ref_axis',(0.,1.,-2.22044604925032E-15));
#32046=DIRECTION('center_axis',(-1.,0.,0.));
#32047=DIRECTION('ref_axis',(0.,-0.707106781186548,0.707106781186548));
#32048=DIRECTION('center_axis',(1.,0.,0.));
#32049=DIRECTION('ref_axis',(0.,-0.707106781186548,0.707106781186548));
#32050=DIRECTION('center_axis',(0.,0.,-1.));
#32051=DIRECTION('ref_axis',(-0.707106781186548,0.707106781186548,0.));
#32052=DIRECTION('center_axis',(0.,-2.22044604925032E-15,1.));
#32053=DIRECTION('ref_axis',(0.,1.,2.22044604925032E-15));
#32054=DIRECTION('',(0.,0.,1.));
#32055=DIRECTION('',(0.,0.,-1.));
#32056=DIRECTION('center_axis',(1.,0.,0.));
#32057=DIRECTION('ref_axis',(0.,0.,-1.));
#32058=DIRECTION('center_axis',(0.,-1.,0.));
#32059=DIRECTION('ref_axis',(0.,0.,1.));
#32060=DIRECTION('center_axis',(-1.,0.,0.));
#32061=DIRECTION('ref_axis',(0.,-0.707106781186547,-0.707106781186548));
#32062=DIRECTION('center_axis',(1.,0.,0.));
#32063=DIRECTION('ref_axis',(0.,-0.707106781186547,-0.707106781186548));
#32064=DIRECTION('center_axis',(0.,1.,0.));
#32065=DIRECTION('ref_axis',(-0.707106781186546,0.,0.707106781186549));
#32066=DIRECTION('center_axis',(0.,-1.,0.));
#32067=DIRECTION('ref_axis',(0.,0.,1.));
#32068=DIRECTION('',(0.,-1.,0.));
#32069=DIRECTION('',(0.,1.,0.));
#32070=DIRECTION('center_axis',(1.,0.,0.));
#32071=DIRECTION('ref_axis',(0.,0.,-1.));
#32072=DIRECTION('center_axis',(0.,2.22044604925032E-15,-1.));
#32073=DIRECTION('ref_axis',(0.,-1.,-2.22044604925032E-15));
#32074=DIRECTION('center_axis',(-1.,0.,0.));
#32075=DIRECTION('ref_axis',(0.,0.707106781186548,-0.707106781186547));
#32076=DIRECTION('center_axis',(0.,0.,1.));
#32077=DIRECTION('ref_axis',(-0.707106781186541,-0.707106781186554,0.));
#32078=DIRECTION('center_axis',(0.,0.,-1.));
#32079=DIRECTION('ref_axis',(0.,-1.,0.));
#32080=DIRECTION('',(0.,0.,-1.));
#32081=DIRECTION('center_axis',(1.,0.,0.));
#32082=DIRECTION('ref_axis',(0.,0.,-1.));
#32083=DIRECTION('center_axis',(-1.,0.,0.));
#32084=DIRECTION('ref_axis',(0.,0.707106781186548,0.707106781186547));
#32085=DIRECTION('center_axis',(-1.,0.,0.));
#32086=DIRECTION('ref_axis',(0.,-1.,-1.48029736616687E-15));
#32087=DIRECTION('',(-1.,0.,0.));
#32088=DIRECTION('',(-1.,0.,0.));
#32089=DIRECTION('center_axis',(0.,-1.,0.));
#32090=DIRECTION('ref_axis',(0.,0.,1.));
#32091=DIRECTION('',(-1.,0.,0.));
#32092=DIRECTION('center_axis',(-1.,0.,0.));
#32093=DIRECTION('ref_axis',(0.,0.,1.));
#32094=DIRECTION('center_axis',(1.,0.,0.));
#32095=DIRECTION('ref_axis',(0.,0.,-1.));
#32096=DIRECTION('',(0.,1.,0.));
#32097=DIRECTION('',(0.,1.,0.));
#32098=DIRECTION('center_axis',(0.,0.,-1.));
#32099=DIRECTION('ref_axis',(-0.707106781186551,-0.707106781186544,0.));
#32100=DIRECTION('center_axis',(4.44089209850062E-15,0.,-1.));
#32101=DIRECTION('ref_axis',(0.,-1.,0.));
#32102=DIRECTION('center_axis',(0.,0.,1.));
#32103=DIRECTION('ref_axis',(-1.,0.,0.));
#32104=DIRECTION('',(0.,0.,1.));
#32105=DIRECTION('center_axis',(0.,1.,0.));
#32106=DIRECTION('ref_axis',(0.,0.,1.));
#32107=DIRECTION('center_axis',(-1.,0.,0.));
#32108=DIRECTION('ref_axis',(0.,0.,-1.));
#32109=DIRECTION('center_axis',(0.,1.,0.));
#32110=DIRECTION('ref_axis',(-0.707106781186548,0.,-0.707106781186548));
#32111=DIRECTION('center_axis',(0.,-1.,0.));
#32112=DIRECTION('ref_axis',(-0.707106781186548,0.,-0.707106781186548));
#32113=DIRECTION('center_axis',(1.,0.,0.));
#32114=DIRECTION('ref_axis',(0.,-0.707106781186544,-0.707106781186551));
#32115=DIRECTION('center_axis',(-1.,0.,0.));
#32116=DIRECTION('ref_axis',(0.,0.,-1.));
#32117=DIRECTION('',(-1.,0.,0.));
#32118=DIRECTION('',(1.,0.,0.));
#32119=DIRECTION('center_axis',(0.,1.,0.));
#32120=DIRECTION('ref_axis',(0.,0.,1.));
#32121=DIRECTION('center_axis',(0.,0.,-1.));
#32122=DIRECTION('ref_axis',(1.,0.,0.));
#32123=DIRECTION('center_axis',(0.,1.,0.));
#32124=DIRECTION('ref_axis',(0.707106781186548,0.,-0.707106781186548));
#32125=DIRECTION('center_axis',(0.,-1.,0.));
#32126=DIRECTION('ref_axis',(0.707106781186548,0.,-0.707106781186548));
#32127=DIRECTION('center_axis',(0.,0.,1.));
#32128=DIRECTION('ref_axis',(0.707106781186551,-0.707106781186544,0.));
#32129=DIRECTION('center_axis',(0.,0.,-1.));
#32130=DIRECTION('ref_axis',(1.,0.,0.));
#32131=DIRECTION('',(0.,0.,-1.));
#32132=DIRECTION('center_axis',(0.,1.,0.));
#32133=DIRECTION('ref_axis',(0.,0.,1.));
#32134=DIRECTION('center_axis',(1.,0.,0.));
#32135=DIRECTION('ref_axis',(0.,0.,1.));
#32136=DIRECTION('center_axis',(0.,1.,0.));
#32137=DIRECTION('ref_axis',(0.707106781186548,0.,0.707106781186548));
#32138=DIRECTION('center_axis',(0.,-1.,0.));
#32139=DIRECTION('ref_axis',(0.707106781186548,0.,0.707106781186548));
#32140=DIRECTION('center_axis',(-1.,0.,0.));
#32141=DIRECTION('ref_axis',(0.,-0.707106781186544,0.707106781186551));
#32142=DIRECTION('center_axis',(1.,0.,0.));
#32143=DIRECTION('ref_axis',(0.,0.,1.));
#32144=DIRECTION('',(1.,0.,0.));
#32145=DIRECTION('',(-1.,0.,0.));
#32146=DIRECTION('center_axis',(0.,1.,0.));
#32147=DIRECTION('ref_axis',(0.,0.,1.));
#32148=DIRECTION('center_axis',(0.,-1.,0.));
#32149=DIRECTION('ref_axis',(-0.707106781186548,0.,0.707106781186548));
#32150=DIRECTION('center_axis',(0.,1.,0.));
#32151=DIRECTION('ref_axis',(-0.707106781186548,0.,0.707106781186548));
#32152=DIRECTION('center_axis',(0.,1.,0.));
#32153=DIRECTION('ref_axis',(1.,0.,0.));
#32154=DIRECTION('',(0.,1.,0.));
#32155=DIRECTION('center_axis',(0.,0.,-1.));
#32156=DIRECTION('ref_axis',(-1.,0.,0.));
#32157=DIRECTION('',(0.,1.,0.));
#32158=DIRECTION('center_axis',(0.,0.,1.));
#32159=DIRECTION('ref_axis',(4.44089209850064E-15,1.,0.));
#32160=DIRECTION('',(0.,-1.,0.));
#32161=DIRECTION('center_axis',(0.,0.,1.));
#32162=DIRECTION('ref_axis',(-1.,0.,0.));
#32163=DIRECTION('',(1.,0.,0.));
#32164=DIRECTION('center_axis',(0.,0.,1.));
#32165=DIRECTION('ref_axis',(-4.44089209850064E-15,-1.,0.));
#32166=DIRECTION('',(0.,1.,0.));
#32167=DIRECTION('center_axis',(0.,0.,1.));
#32168=DIRECTION('ref_axis',(1.,0.,0.));
#32169=DIRECTION('center_axis',(0.,1.,0.));
#32170=DIRECTION('ref_axis',(0.,0.,-1.));
#32171=DIRECTION('center_axis',(0.,1.,0.));
#32172=DIRECTION('ref_axis',(1.,0.,0.));
#32173=DIRECTION('center_axis',(0.,-1.,0.));
#32174=DIRECTION('ref_axis',(0.,0.,1.));
#32175=DIRECTION('center_axis',(0.,0.,1.));
#32176=DIRECTION('ref_axis',(-0.707106781186541,-0.707106781186554,0.));
#32177=DIRECTION('center_axis',(0.,0.,1.));
#32178=DIRECTION('ref_axis',(-1.,0.,0.));
#32179=DIRECTION('',(0.,0.,1.));
#32180=DIRECTION('center_axis',(0.,-2.22044604925032E-15,-1.));
#32181=DIRECTION('ref_axis',(0.,-1.,2.22044604925032E-15));
#32182=DIRECTION('center_axis',(1.,0.,0.));
#32183=DIRECTION('ref_axis',(0.,0.,-1.));
#32184=DIRECTION('center_axis',(0.,1.,0.));
#32185=DIRECTION('ref_axis',(0.,0.,-1.));
#32186=DIRECTION('center_axis',(1.,0.,0.));
#32187=DIRECTION('ref_axis',(0.,0.707106781186548,0.707106781186547));
#32188=DIRECTION('center_axis',(0.,-1.,0.));
#32189=DIRECTION('ref_axis',(-0.707106781186546,0.,-0.707106781186549));
#32190=DIRECTION('center_axis',(0.,1.,0.));
#32191=DIRECTION('ref_axis',(0.,0.,-1.));
#32192=DIRECTION('',(0.,-1.,0.));
#32193=DIRECTION('center_axis',(1.,0.,0.));
#32194=DIRECTION('ref_axis',(0.,0.,-1.));
#32195=DIRECTION('center_axis',(0.,2.22044604925032E-15,1.));
#32196=DIRECTION('ref_axis',(0.,1.,-2.22044604925032E-15));
#32197=DIRECTION('center_axis',(1.,0.,0.));
#32198=DIRECTION('ref_axis',(0.,-0.707106781186548,0.707106781186548));
#32199=DIRECTION('center_axis',(0.,0.,-1.));
#32200=DIRECTION('ref_axis',(-0.707106781186548,0.707106781186548,0.));
#32201=DIRECTION('center_axis',(0.,0.,1.));
#32202=DIRECTION('ref_axis',(0.,1.,0.));
#32203=DIRECTION('',(0.,0.,-1.));
#32204=DIRECTION('center_axis',(1.,0.,0.));
#32205=DIRECTION('ref_axis',(0.,0.,-1.));
#32206=DIRECTION('center_axis',(0.,-1.,0.));
#32207=DIRECTION('ref_axis',(0.,0.,1.));
#32208=DIRECTION('center_axis',(1.,0.,0.));
#32209=DIRECTION('ref_axis',(0.,-0.707106781186547,-0.707106781186548));
#32210=DIRECTION('center_axis',(0.,1.,0.));
#32211=DIRECTION('ref_axis',(-0.707106781186546,0.,0.707106781186549));
#32212=DIRECTION('center_axis',(0.,-1.,0.));
#32213=DIRECTION('ref_axis',(0.,0.,1.));
#32214=DIRECTION('',(0.,1.,0.));
#32215=DIRECTION('center_axis',(1.,0.,0.));
#32216=DIRECTION('ref_axis',(0.,0.,-1.));
#32217=DIRECTION('center_axis',(1.,0.,0.));
#32218=DIRECTION('ref_axis',(0.,0.707106781186548,-0.707106781186547));
#32219=DIRECTION('center_axis',(1.,0.,0.));
#32220=DIRECTION('ref_axis',(0.,0.,1.));
#32221=DIRECTION('',(1.,0.,0.));
#32222=DIRECTION('center_axis',(-1.,0.,0.));
#32223=DIRECTION('ref_axis',(0.,-0.707106781186548,0.707106781186548));
#32224=DIRECTION('',(1.,0.,0.));
#32225=DIRECTION('center_axis',(0.,0.,1.));
#32226=DIRECTION('ref_axis',(0.,-1.,0.));
#32227=DIRECTION('',(1.,0.,0.));
#32228=DIRECTION('',(0.,1.,0.));
#32229=DIRECTION('center_axis',(1.,0.,0.));
#32230=DIRECTION('ref_axis',(0.,1.,-2.22044604925032E-15));
#32231=DIRECTION('',(1.,0.,0.));
#32232=DIRECTION('center_axis',(-1.,0.,0.));
#32233=DIRECTION('ref_axis',(0.,0.707106781186548,0.707106781186547));
#32234=DIRECTION('center_axis',(0.,1.,0.));
#32235=DIRECTION('ref_axis',(0.,0.,1.));
#32236=DIRECTION('',(1.,0.,0.));
#32237=DIRECTION('',(0.,0.,-1.));
#32238=DIRECTION('center_axis',(0.,0.,-1.));
#32239=DIRECTION('ref_axis',(0.707106781186541,-0.707106781186554,0.));
#32240=DIRECTION('center_axis',(0.,2.22044604925032E-15,-1.));
#32241=DIRECTION('ref_axis',(1.,0.,0.));
#32242=DIRECTION('center_axis',(0.,0.,1.));
#32243=DIRECTION('ref_axis',(0.,-1.,0.));
#32244=DIRECTION('center_axis',(-1.,0.,0.));
#32245=DIRECTION('ref_axis',(0.,0.,1.));
#32246=DIRECTION('center_axis',(0.,1.,0.));
#32247=DIRECTION('ref_axis',(0.,0.,1.));
#32248=DIRECTION('center_axis',(-1.,0.,0.));
#32249=DIRECTION('ref_axis',(0.,0.707106781186548,-0.707106781186547));
#32250=DIRECTION('center_axis',(0.,-1.,0.));
#32251=DIRECTION('ref_axis',(0.707106781186546,0.,0.707106781186549));
#32252=DIRECTION('center_axis',(0.,1.,0.));
#32253=DIRECTION('ref_axis',(0.,0.,1.));
#32254=DIRECTION('',(0.,-1.,0.));
#32255=DIRECTION('center_axis',(-1.,0.,0.));
#32256=DIRECTION('ref_axis',(0.,0.,1.));
#32257=DIRECTION('center_axis',(0.,2.22044604925032E-15,-1.));
#32258=DIRECTION('ref_axis',(0.,1.,2.22044604925032E-15));
#32259=DIRECTION('center_axis',(-1.,0.,0.));
#32260=DIRECTION('ref_axis',(0.,-0.707106781186547,-0.707106781186548));
#32261=DIRECTION('center_axis',(0.,0.,1.));
#32262=DIRECTION('ref_axis',(0.707106781186548,0.707106781186548,0.));
#32263=DIRECTION('center_axis',(0.,-2.22044604925032E-15,-1.));
#32264=DIRECTION('ref_axis',(0.,1.,-2.22044604925032E-15));
#32265=DIRECTION('',(0.,0.,1.));
#32266=DIRECTION('center_axis',(-1.,0.,0.));
#32267=DIRECTION('ref_axis',(0.,0.,1.));
#32268=DIRECTION('center_axis',(0.,-1.,0.));
#32269=DIRECTION('ref_axis',(0.,0.,-1.));
#32270=DIRECTION('center_axis',(0.,1.,0.));
#32271=DIRECTION('ref_axis',(0.707106781186546,0.,-0.707106781186549));
#32272=DIRECTION('center_axis',(0.,-1.,0.));
#32273=DIRECTION('ref_axis',(0.,0.,-1.));
#32274=DIRECTION('center_axis',(-1.,0.,0.));
#32275=DIRECTION('ref_axis',(0.,0.,1.));
#32276=DIRECTION('center_axis',(1.,0.,0.));
#32277=DIRECTION('ref_axis',(0.,-1.,-1.48029736616687E-15));
#32278=DIRECTION('',(1.,0.,0.));
#32279=DIRECTION('',(1.,0.,0.));
#32280=DIRECTION('center_axis',(0.,0.,-1.));
#32281=DIRECTION('ref_axis',(0.,1.,0.));
#32282=DIRECTION('',(1.,0.,0.));
#32283=DIRECTION('center_axis',(1.,0.,0.));
#32284=DIRECTION('ref_axis',(0.,0.,-1.));
#32285=DIRECTION('center_axis',(0.,1.,0.));
#32286=DIRECTION('ref_axis',(1.,0.,0.));
#32287=DIRECTION('center_axis',(0.,1.,0.));
#32288=DIRECTION('ref_axis',(1.,0.,0.));
#32289=DIRECTION('center_axis',(0.,1.,0.));
#32290=DIRECTION('ref_axis',(1.,0.,0.));
#32291=DIRECTION('center_axis',(0.,1.,0.));
#32292=DIRECTION('ref_axis',(1.,0.,0.));
#32293=DIRECTION('center_axis',(0.,-1.,0.));
#32294=DIRECTION('ref_axis',(1.,0.,0.));
#32295=DIRECTION('',(0.,-1.,0.));
#32296=DIRECTION('center_axis',(0.,-1.,0.));
#32297=DIRECTION('ref_axis',(1.,0.,0.));
#32298=DIRECTION('',(0.,-1.,0.));
#32299=DIRECTION('center_axis',(0.,-1.,0.));
#32300=DIRECTION('ref_axis',(1.,0.,0.));
#32301=DIRECTION('',(0.,-1.,0.));
#32302=DIRECTION('center_axis',(0.,-1.,0.));
#32303=DIRECTION('ref_axis',(1.,0.,0.));
#32304=DIRECTION('',(0.,-1.,0.));
#32305=DIRECTION('center_axis',(0.,-1.,0.));
#32306=DIRECTION('ref_axis',(0.,0.,-1.));
#32307=DIRECTION('center_axis',(0.,0.,-1.));
#32308=DIRECTION('ref_axis',(0.,-1.,0.));
#32309=DIRECTION('center_axis',(0.,-1.,0.));
#32310=DIRECTION('ref_axis',(0.,0.,-1.));
#32311=DIRECTION('center_axis',(0.,1.,0.));
#32312=DIRECTION('ref_axis',(1.,0.,0.));
#32313=DIRECTION('center_axis',(0.,1.,0.));
#32314=DIRECTION('ref_axis',(0.,0.,1.));
#32315=DIRECTION('center_axis',(0.,1.,0.));
#32316=DIRECTION('ref_axis',(0.,0.,1.));
#32317=DIRECTION('',(0.,1.,0.));
#32318=DIRECTION('center_axis',(0.,-1.,0.));
#32319=DIRECTION('ref_axis',(0.,0.,-1.));
#32320=DIRECTION('center_axis',(0.,1.,0.));
#32321=DIRECTION('ref_axis',(1.,0.,0.));
#32322=DIRECTION('center_axis',(0.,1.,0.));
#32323=DIRECTION('ref_axis',(0.,0.,1.));
#32324=DIRECTION('center_axis',(0.,1.,0.));
#32325=DIRECTION('ref_axis',(0.,0.,1.));
#32326=DIRECTION('',(0.,1.,0.));
#32327=DIRECTION('center_axis',(0.,1.,0.));
#32328=DIRECTION('ref_axis',(2.96059473233374E-15,0.,1.));
#32329=DIRECTION('',(0.,1.,0.));
#32330=DIRECTION('center_axis',(0.,0.,1.));
#32331=DIRECTION('ref_axis',(1.,0.,0.));
#32332=DIRECTION('',(0.,1.,0.));
#32333=DIRECTION('center_axis',(0.,1.,0.));
#32334=DIRECTION('ref_axis',(-1.,0.,2.96059473233374E-15));
#32335=DIRECTION('center_axis',(0.,0.,-1.));
#32336=DIRECTION('ref_axis',(-1.,0.,0.));
#32337=DIRECTION('',(0.,1.,0.));
#32338=DIRECTION('center_axis',(0.,1.,0.));
#32339=DIRECTION('ref_axis',(1.,0.,-2.96059473233374E-15));
#32340=DIRECTION('center_axis',(1.,0.,0.));
#32341=DIRECTION('ref_axis',(0.,1.,0.));
#32342=DIRECTION('',(0.,0.,1.));
#32343=DIRECTION('center_axis',(0.,0.,1.));
#32344=DIRECTION('ref_axis',(0.,-1.,0.));
#32345=DIRECTION('',(0.,0.,1.));
#32346=DIRECTION('center_axis',(0.,-1.,0.));
#32347=DIRECTION('ref_axis',(1.,0.,0.));
#32348=DIRECTION('',(0.,0.,1.));
#32349=DIRECTION('center_axis',(0.,0.,1.));
#32350=DIRECTION('ref_axis',(-1.,0.,0.));
#32351=DIRECTION('center_axis',(0.,-1.,0.));
#32352=DIRECTION('ref_axis',(1.,0.,0.));
#32353=DIRECTION('',(0.,0.,1.));
#32354=DIRECTION('',(0.,0.,1.));
#32355=DIRECTION('center_axis',(0.,0.,1.));
#32356=DIRECTION('ref_axis',(-1.,0.,0.));
#32357=DIRECTION('',(0.,0.,1.));
#32358=DIRECTION('center_axis',(-1.,0.,0.));
#32359=DIRECTION('ref_axis',(0.,-1.,0.));
#32360=DIRECTION('',(0.,0.,1.));
#32361=DIRECTION('center_axis',(0.,0.,1.));
#32362=DIRECTION('ref_axis',(4.44089209850064E-15,1.,0.));
#32363=DIRECTION('',(0.,0.,1.));
#32364=DIRECTION('center_axis',(0.,1.,0.));
#32365=DIRECTION('ref_axis',(-1.,0.,0.));
#32366=DIRECTION('',(0.,0.,1.));
#32367=DIRECTION('center_axis',(0.,0.,1.));
#32368=DIRECTION('ref_axis',(1.,0.,0.));
#32369=DIRECTION('',(0.,0.,1.));
#32370=DIRECTION('center_axis',(1.,0.,0.));
#32371=DIRECTION('ref_axis',(0.,1.,0.));
#32372=DIRECTION('',(0.,0.,1.));
#32373=DIRECTION('center_axis',(0.,0.,1.));
#32374=DIRECTION('ref_axis',(-4.44089209850064E-15,-1.,0.));
#32375=DIRECTION('center_axis',(0.,0.,1.));
#32376=DIRECTION('ref_axis',(1.,0.,0.));
#32377=DIRECTION('',(0.,1.,0.));
#32378=DIRECTION('',(0.,1.,0.));
#32379=DIRECTION('center_axis',(0.,1.,0.));
#32380=DIRECTION('ref_axis',(-1.,0.,0.));
#32381=DIRECTION('center_axis',(0.,1.,0.));
#32382=DIRECTION('ref_axis',(0.,0.,1.));
#32383=DIRECTION('center_axis',(0.,1.,0.));
#32384=DIRECTION('ref_axis',(0.,0.,1.));
#32385=DIRECTION('',(0.,-1.,0.));
#32386=DIRECTION('center_axis',(0.,-1.,0.));
#32387=DIRECTION('ref_axis',(0.,0.,1.));
#32388=DIRECTION('',(-8.48405894740086E-18,-0.99759742096768,-0.0692775986783111));
#32389=DIRECTION('axis',(0.,0.,1.));
#32390=DIRECTION('refdir',(1.,0.,0.));
#32391=DIRECTION('center_axis',(-0.612372435695795,0.707106781186547,0.353553390593274));
#32392=DIRECTION('ref_axis',(0.5,0.,0.866025403784439));
#32393=DIRECTION('center_axis',(-0.612372435695795,0.707106781186547,0.353553390593274));
#32394=DIRECTION('ref_axis',(-0.612372435695794,-0.707106781186548,0.353553390593273));
#32395=DIRECTION('',(0.5,0.,0.866025403784439));
#32396=DIRECTION('',(-0.788675134594812,-0.577350269189626,-0.211324865405189));
#32397=DIRECTION('',(-0.5,0.,-0.866025403784439));
#32398=DIRECTION('center_axis',(0.866025403784439,0.,-0.5));
#32399=DIRECTION('ref_axis',(0.5,0.,0.866025403784439));
#32400=DIRECTION('',(0.,1.,0.));
#32401=DIRECTION('',(0.5,0.,0.866025403784439));
#32402=DIRECTION('',(0.,-1.,0.));
#32403=DIRECTION('center_axis',(0.,1.,0.));
#32404=DIRECTION('ref_axis',(0.,0.,1.));
#32405=DIRECTION('center_axis',(0.,1.,0.));
#32406=DIRECTION('ref_axis',(1.,0.,0.));
#32407=DIRECTION('center_axis',(0.672498511963959,0.707106781186546,-0.218508012224411));
#32408=DIRECTION('ref_axis',(-0.672498511963956,0.707106781186549,0.21850801222441));
#32409=DIRECTION('',(0.,-1.,0.));
#32410=DIRECTION('center_axis',(0.,-1.,0.));
#32411=DIRECTION('ref_axis',(0.,0.,1.));
#32412=DIRECTION('',(0.,1.,0.));
#32413=DIRECTION('center_axis',(-0.672498511963953,0.707106781186552,0.218508012224409));
#32414=DIRECTION('ref_axis',(-0.672498511963962,-0.707106781186543,0.218508012224412));
#32415=DIRECTION('center_axis',(0.,1.,0.));
#32416=DIRECTION('ref_axis',(1.,0.,0.));
#32417=DIRECTION('center_axis',(0.703233176253404,0.707106781186548,-0.0739127852035666));
#32418=DIRECTION('ref_axis',(-0.703233176253404,0.707106781186547,0.0739127852035666));
#32419=DIRECTION('',(0.,-1.,0.));
#32420=DIRECTION('center_axis',(0.,-1.,0.));
#32421=DIRECTION('ref_axis',(0.,0.,1.));
#32422=DIRECTION('',(0.,1.,0.));
#32423=DIRECTION('center_axis',(-0.703233176253404,0.707106781186547,0.0739127852035666));
#32424=DIRECTION('ref_axis',(-0.703233176253404,-0.707106781186548,0.0739127852035665));
#32425=DIRECTION('center_axis',(0.,1.,0.));
#32426=DIRECTION('ref_axis',(1.,0.,0.));
#32427=DIRECTION('',(0.,-1.,0.));
#32428=DIRECTION('center_axis',(0.,1.,0.));
#32429=DIRECTION('ref_axis',(1.,0.,0.));
#32430=DIRECTION('center_axis',(-0.703233176253403,-0.707106781186549,0.0739127852035665));
#32431=DIRECTION('ref_axis',(-0.703233176253406,0.707106781186546,0.0739127852035667));
#32432=DIRECTION('',(0.,1.,0.));
#32433=DIRECTION('center_axis',(0.,1.,0.));
#32434=DIRECTION('ref_axis',(0.,0.,1.));
#32435=DIRECTION('',(0.,-1.,0.));
#32436=DIRECTION('center_axis',(0.703233176253405,-0.707106781186546,-0.0739127852035667));
#32437=DIRECTION('ref_axis',(-0.703233176253403,-0.707106781186549,0.0739127852035666));
#32438=DIRECTION('center_axis',(0.,1.,0.));
#32439=DIRECTION('ref_axis',(1.,0.,0.));
#32440=DIRECTION('center_axis',(-0.672498511963956,-0.70710678118655,0.21850801222441));
#32441=DIRECTION('ref_axis',(-0.672498511963959,0.707106781186545,0.218508012224411));
#32442=DIRECTION('',(0.,1.,0.));
#32443=DIRECTION('center_axis',(0.,1.,0.));
#32444=DIRECTION('ref_axis',(0.,0.,1.));
#32445=DIRECTION('',(0.,-1.,0.));
#32446=DIRECTION('center_axis',(0.672498511963956,-0.707106781186549,-0.21850801222441));
#32447=DIRECTION('ref_axis',(-0.672498511963959,-0.707106781186546,0.218508012224411));
#32448=DIRECTION('center_axis',(0.,1.,0.));
#32449=DIRECTION('ref_axis',(1.,0.,0.));
#32450=DIRECTION('center_axis',(-0.612372435695791,-0.707106781186552,0.353553390593272));
#32451=DIRECTION('ref_axis',(-0.612372435695798,0.707106781186543,0.353553390593276));
#32452=DIRECTION('',(0.,1.,0.));
#32453=DIRECTION('center_axis',(0.,1.,0.));
#32454=DIRECTION('ref_axis',(0.,0.,1.));
#32455=DIRECTION('',(0.,-1.,0.));
#32456=DIRECTION('center_axis',(0.612372435695794,-0.707106781186548,-0.353553390593274));
#32457=DIRECTION('ref_axis',(-0.612372435695795,-0.707106781186547,0.353553390593274));
#32458=DIRECTION('center_axis',(0.,1.,0.));
#32459=DIRECTION('ref_axis',(1.,0.,0.));
#32460=DIRECTION('center_axis',(-0.525482745498768,-0.707106781186536,0.473146789255823));
#32461=DIRECTION('ref_axis',(-0.52548274549875,0.707106781186559,0.473146789255807));
#32462=DIRECTION('',(0.,1.,0.));
#32463=DIRECTION('center_axis',(0.,1.,0.));
#32464=DIRECTION('ref_axis',(0.,0.,1.));
#32465=DIRECTION('',(0.,-1.,0.));
#32466=DIRECTION('center_axis',(0.525482745498765,-0.70710678118654,-0.47314678925582));
#32467=DIRECTION('ref_axis',(-0.525482745498753,-0.707106781186555,0.47314678925581));
#32468=DIRECTION('center_axis',(0.,1.,0.));
#32469=DIRECTION('ref_axis',(1.,0.,0.));
#32470=DIRECTION('center_axis',(-0.415626937777454,-0.707106781186547,0.572061402817684));
#32471=DIRECTION('ref_axis',(-0.415626937777453,0.707106781186548,0.572061402817684));
#32472=DIRECTION('',(0.,1.,0.));
#32473=DIRECTION('center_axis',(0.,1.,0.));
#32474=DIRECTION('ref_axis',(0.,0.,1.));
#32475=DIRECTION('',(0.,-1.,0.));
#32476=DIRECTION('center_axis',(0.415626937777452,-0.707106781186551,-0.572061402817682));
#32477=DIRECTION('ref_axis',(-0.415626937777455,-0.707106781186544,0.572061402817687));
#32478=DIRECTION('center_axis',(0.,1.,0.));
#32479=DIRECTION('ref_axis',(1.,0.,0.));
#32480=DIRECTION('center_axis',(-0.287606238475956,-0.707106781186536,0.645974188021262));
#32481=DIRECTION('ref_axis',(-0.287606238475946,0.707106781186559,0.64597418802124));
#32482=DIRECTION('',(0.,1.,0.));
#32483=DIRECTION('center_axis',(0.,1.,0.));
#32484=DIRECTION('ref_axis',(0.,0.,1.));
#32485=DIRECTION('',(0.,-1.,0.));
#32486=DIRECTION('center_axis',(0.287606238475952,-0.707106781186546,-0.645974188021253));
#32487=DIRECTION('ref_axis',(-0.28760623847595,-0.707106781186549,0.645974188021249));
#32488=DIRECTION('center_axis',(0.,1.,0.));
#32489=DIRECTION('ref_axis',(1.,0.,0.));
#32490=DIRECTION('center_axis',(-0.147015766465198,-0.707106781186553,0.69165480148022));
#32491=DIRECTION('ref_axis',(-0.1470157664652,0.707106781186542,0.691654801480231));
#32492=DIRECTION('',(0.,1.,0.));
#32493=DIRECTION('center_axis',(0.,1.,0.));
#32494=DIRECTION('ref_axis',(0.,0.,1.));
#32495=DIRECTION('',(0.,-1.,0.));
#32496=DIRECTION('center_axis',(0.1470157664652,-0.707106781186543,-0.69165480148023));
#32497=DIRECTION('ref_axis',(-0.147015766465198,-0.707106781186552,0.691654801480221));
#32498=DIRECTION('center_axis',(0.,1.,0.));
#32499=DIRECTION('ref_axis',(1.,0.,0.));
#32500=DIRECTION('center_axis',(-8.65956056235491E-17,-0.707106781186549,
0.707106781186546));
#32501=DIRECTION('ref_axis',(0.,0.707106781186546,0.70710678118655));
#32502=DIRECTION('',(0.,1.,0.));
#32503=DIRECTION('center_axis',(0.,1.,0.));
#32504=DIRECTION('ref_axis',(0.,0.,1.));
#32505=DIRECTION('',(0.,-1.,0.));
#32506=DIRECTION('center_axis',(8.65956056235492E-17,-0.707106781186549,
-0.707106781186546));
#32507=DIRECTION('ref_axis',(0.,-0.707106781186546,0.707106781186549));
#32508=DIRECTION('center_axis',(0.,1.,0.));
#32509=DIRECTION('ref_axis',(1.,0.,0.));
#32510=DIRECTION('center_axis',(0.147015766465198,-0.707106781186549,0.691654801480225));
#32511=DIRECTION('ref_axis',(0.147015766465198,0.707106781186547,0.691654801480227));
#32512=DIRECTION('',(0.,1.,0.));
#32513=DIRECTION('center_axis',(0.,1.,0.));
#32514=DIRECTION('ref_axis',(0.,0.,1.));
#32515=DIRECTION('',(0.,-1.,0.));
#32516=DIRECTION('center_axis',(-0.147015766465198,-0.707106781186548,-0.691654801480226));
#32517=DIRECTION('ref_axis',(0.147015766465198,-0.707106781186547,0.691654801480226));
#32518=DIRECTION('center_axis',(0.,1.,0.));
#32519=DIRECTION('ref_axis',(1.,0.,0.));
#32520=DIRECTION('center_axis',(0.287606238475948,-0.707106781186554,0.645974188021245));
#32521=DIRECTION('ref_axis',(0.287606238475953,0.707106781186541,0.645974188021257));
#32522=DIRECTION('',(0.,1.,0.));
#32523=DIRECTION('center_axis',(0.,1.,0.));
#32524=DIRECTION('ref_axis',(0.,0.,1.));
#32525=DIRECTION('',(0.,-1.,0.));
#32526=DIRECTION('center_axis',(-0.28760623847595,-0.707106781186549,-0.64597418802125));
#32527=DIRECTION('ref_axis',(0.287606238475951,-0.707106781186546,0.645974188021252));
#32528=DIRECTION('center_axis',(0.,1.,0.));
#32529=DIRECTION('ref_axis',(1.,0.,0.));
#32530=DIRECTION('center_axis',(0.415626937777451,-0.707106781186552,0.572061402817681));
#32531=DIRECTION('ref_axis',(0.415626937777456,0.707106781186543,0.572061402817688));
#32532=DIRECTION('',(0.,1.,0.));
#32533=DIRECTION('center_axis',(0.,1.,0.));
#32534=DIRECTION('ref_axis',(0.,0.,1.));
#32535=DIRECTION('',(0.,-1.,0.));
#32536=DIRECTION('center_axis',(-0.415626937777457,-0.707106781186541,-0.57206140281769));
#32537=DIRECTION('ref_axis',(0.415626937777449,-0.707106781186554,0.572061402817679));
#32538=DIRECTION('center_axis',(0.,1.,0.));
#32539=DIRECTION('ref_axis',(1.,0.,0.));
#32540=DIRECTION('center_axis',(0.525482745498763,-0.707106781186542,0.473146789255819));
#32541=DIRECTION('ref_axis',(0.525482745498754,0.707106781186554,0.473146789255811));
#32542=DIRECTION('',(0.,1.,0.));
#32543=DIRECTION('center_axis',(0.,1.,0.));
#32544=DIRECTION('ref_axis',(0.,0.,1.));
#32545=DIRECTION('',(0.,-1.,0.));
#32546=DIRECTION('center_axis',(-0.525482745498763,-0.707106781186542,-0.473146789255819));
#32547=DIRECTION('ref_axis',(0.525482745498754,-0.707106781186554,0.473146789255811));
#32548=DIRECTION('center_axis',(0.,1.,0.));
#32549=DIRECTION('ref_axis',(1.,0.,0.));
#32550=DIRECTION('center_axis',(0.612372435695789,-0.707106781186554,0.353553390593271));
#32551=DIRECTION('ref_axis',(0.6123724356958,0.707106781186541,0.353553390593277));
#32552=DIRECTION('',(0.,1.,0.));
#32553=DIRECTION('center_axis',(0.,1.,0.));
#32554=DIRECTION('ref_axis',(0.,0.,1.));
#32555=DIRECTION('',(0.,-1.,0.));
#32556=DIRECTION('center_axis',(-0.612372435695789,-0.707106781186554,-0.353553390593271));
#32557=DIRECTION('ref_axis',(0.6123724356958,-0.707106781186541,0.353553390593277));
#32558=DIRECTION('center_axis',(0.,1.,0.));
#32559=DIRECTION('ref_axis',(1.,0.,0.));
#32560=DIRECTION('center_axis',(0.672498511963956,-0.707106781186549,0.21850801222441));
#32561=DIRECTION('ref_axis',(0.672498511963959,0.707106781186546,0.218508012224411));
#32562=DIRECTION('',(0.,1.,0.));
#32563=DIRECTION('center_axis',(0.,1.,0.));
#32564=DIRECTION('ref_axis',(0.,0.,1.));
#32565=DIRECTION('',(0.,-1.,0.));
#32566=DIRECTION('center_axis',(-0.672498511963956,-0.707106781186549,-0.21850801222441));
#32567=DIRECTION('ref_axis',(0.672498511963959,-0.707106781186546,0.218508012224411));
#32568=DIRECTION('center_axis',(0.,1.,0.));
#32569=DIRECTION('ref_axis',(1.,0.,0.));
#32570=DIRECTION('center_axis',(0.703233176253405,-0.707106781186547,0.0739127852035674));
#32571=DIRECTION('ref_axis',(0.703233176253403,0.707106781186548,0.0739127852035672));
#32572=DIRECTION('',(0.,1.,0.));
#32573=DIRECTION('center_axis',(0.,1.,0.));
#32574=DIRECTION('ref_axis',(0.,0.,1.));
#32575=DIRECTION('',(0.,-1.,0.));
#32576=DIRECTION('center_axis',(-0.703233176253405,-0.707106781186547,-0.0739127852035674));
#32577=DIRECTION('ref_axis',(0.703233176253403,-0.707106781186548,0.0739127852035672));
#32578=DIRECTION('center_axis',(0.,1.,0.));
#32579=DIRECTION('ref_axis',(1.,0.,0.));
#32580=DIRECTION('center_axis',(0.703233176253406,-0.707106781186546,-0.0739127852035666));
#32581=DIRECTION('ref_axis',(-0.703233176253402,-0.707106781186549,0.0739127852035662));
#32582=DIRECTION('',(0.,1.,0.));
#32583=DIRECTION('center_axis',(0.,1.,0.));
#32584=DIRECTION('ref_axis',(0.,0.,1.));
#32585=DIRECTION('',(0.,-1.,0.));
#32586=DIRECTION('center_axis',(-0.703233176253405,-0.707106781186547,0.0739127852035665));
#32587=DIRECTION('ref_axis',(-0.703233176253403,0.707106781186548,0.0739127852035663));
#32588=DIRECTION('center_axis',(0.,1.,0.));
#32589=DIRECTION('ref_axis',(1.,0.,0.));
#32590=DIRECTION('center_axis',(0.672498511963956,-0.707106781186549,-0.21850801222441));
#32591=DIRECTION('ref_axis',(-0.672498511963959,-0.707106781186546,0.218508012224411));
#32592=DIRECTION('',(0.,1.,0.));
#32593=DIRECTION('center_axis',(0.,1.,0.));
#32594=DIRECTION('ref_axis',(0.,0.,1.));
#32595=DIRECTION('',(0.,-1.,0.));
#32596=DIRECTION('center_axis',(-0.672498511963959,-0.707106781186545,0.218508012224411));
#32597=DIRECTION('ref_axis',(-0.672498511963955,0.70710678118655,0.21850801222441));
#32598=DIRECTION('center_axis',(0.,1.,0.));
#32599=DIRECTION('ref_axis',(1.,0.,0.));
#32600=DIRECTION('center_axis',(0.612372435695792,-0.707106781186551,-0.353553390593272));
#32601=DIRECTION('ref_axis',(-0.612372435695797,-0.707106781186545,0.353553390593275));
#32602=DIRECTION('',(0.,1.,0.));
#32603=DIRECTION('center_axis',(0.,1.,0.));
#32604=DIRECTION('ref_axis',(0.,0.,1.));
#32605=DIRECTION('',(0.,-1.,0.));
#32606=DIRECTION('center_axis',(-0.612372435695802,-0.70710678118654,0.353553390593277));
#32607=DIRECTION('ref_axis',(-0.612372435695788,0.707106781186555,0.353553390593269));
#32608=DIRECTION('center_axis',(0.,1.,0.));
#32609=DIRECTION('ref_axis',(1.,0.,0.));
#32610=DIRECTION('center_axis',(0.525482745498764,-0.707106781186541,-0.473146789255819));
#32611=DIRECTION('ref_axis',(-0.525482745498755,-0.707106781186554,0.473146789255811));
#32612=DIRECTION('',(0.,1.,0.));
#32613=DIRECTION('center_axis',(0.,1.,0.));
#32614=DIRECTION('ref_axis',(0.,0.,1.));
#32615=DIRECTION('',(0.,-1.,0.));
#32616=DIRECTION('center_axis',(-0.525482745498762,-0.707106781186544,0.473146789255817));
#32617=DIRECTION('ref_axis',(-0.525482745498757,0.707106781186551,0.473146789255813));
#32618=DIRECTION('center_axis',(0.,1.,0.));
#32619=DIRECTION('ref_axis',(1.,0.,0.));
#32620=DIRECTION('center_axis',(0.415626937777451,-0.707106781186552,-0.572061402817681));
#32621=DIRECTION('ref_axis',(-0.415626937777456,-0.707106781186543,0.572061402817688));
#32622=DIRECTION('',(0.,1.,0.));
#32623=DIRECTION('center_axis',(0.,1.,0.));
#32624=DIRECTION('ref_axis',(0.,0.,1.));
#32625=DIRECTION('',(0.,-1.,0.));
#32626=DIRECTION('center_axis',(-0.415626937777453,-0.707106781186549,0.572061402817683));
#32627=DIRECTION('ref_axis',(-0.415626937777454,0.707106781186547,0.572061402817685));
#32628=DIRECTION('center_axis',(0.,1.,0.));
#32629=DIRECTION('ref_axis',(1.,0.,0.));
#32630=DIRECTION('center_axis',(0.287606238475947,-0.707106781186558,-0.645974188021242));
#32631=DIRECTION('ref_axis',(-0.287606238475955,-0.707106781186537,0.64597418802126));
#32632=DIRECTION('',(0.,1.,0.));
#32633=DIRECTION('center_axis',(0.,1.,0.));
#32634=DIRECTION('ref_axis',(0.,0.,1.));
#32635=DIRECTION('',(0.,-1.,0.));
#32636=DIRECTION('center_axis',(-0.287606238475954,-0.70710678118654,0.645974188021258));
#32637=DIRECTION('ref_axis',(-0.287606238475948,0.707106781186555,0.645974188021244));
#32638=DIRECTION('center_axis',(0.,1.,0.));
#32639=DIRECTION('ref_axis',(1.,0.,0.));
#32640=DIRECTION('center_axis',(0.147015766465199,-0.707106781186549,-0.691654801480225));
#32641=DIRECTION('ref_axis',(-0.147015766465199,-0.707106781186547,0.691654801480227));
#32642=DIRECTION('',(0.,1.,0.));
#32643=DIRECTION('center_axis',(0.,1.,0.));
#32644=DIRECTION('ref_axis',(0.,0.,1.));
#32645=DIRECTION('',(0.,-1.,0.));
#32646=DIRECTION('center_axis',(-0.1470157664652,-0.707106781186542,0.69165480148023));
#32647=DIRECTION('ref_axis',(-0.147015766465198,0.707106781186553,0.691654801480221));
#32648=DIRECTION('center_axis',(0.,1.,0.));
#32649=DIRECTION('ref_axis',(1.,0.,0.));
#32650=DIRECTION('center_axis',(0.,-0.707106781186549,-0.707106781186546));
#32651=DIRECTION('ref_axis',(0.,-0.707106781186546,0.707106781186549));
#32652=DIRECTION('',(0.,1.,0.));
#32653=DIRECTION('center_axis',(0.,1.,0.));
#32654=DIRECTION('ref_axis',(0.,0.,1.));
#32655=DIRECTION('',(0.,-1.,0.));
#32656=DIRECTION('center_axis',(0.,-0.707106781186549,0.707106781186546));
#32657=DIRECTION('ref_axis',(0.,0.707106781186546,0.707106781186549));
#32658=DIRECTION('center_axis',(0.,1.,0.));
#32659=DIRECTION('ref_axis',(1.,0.,0.));
#32660=DIRECTION('center_axis',(-0.147015766465198,-0.70710678118655,-0.691654801480224));
#32661=DIRECTION('ref_axis',(0.147015766465199,-0.707106781186545,0.691654801480228));
#32662=DIRECTION('',(0.,1.,0.));
#32663=DIRECTION('center_axis',(0.,1.,0.));
#32664=DIRECTION('ref_axis',(0.,0.,1.));
#32665=DIRECTION('',(0.,-1.,0.));
#32666=DIRECTION('center_axis',(0.147015766465198,-0.707106781186549,0.691654801480225));
#32667=DIRECTION('ref_axis',(0.147015766465199,0.707106781186547,0.691654801480227));
#32668=DIRECTION('center_axis',(0.,1.,0.));
#32669=DIRECTION('ref_axis',(1.,0.,0.));
#32670=DIRECTION('center_axis',(-0.287606238475955,-0.707106781186538,-0.64597418802126));
#32671=DIRECTION('ref_axis',(0.287606238475947,-0.707106781186557,0.645974188021242));
#32672=DIRECTION('',(0.,1.,0.));
#32673=DIRECTION('center_axis',(0.,1.,0.));
#32674=DIRECTION('ref_axis',(0.,0.,1.));
#32675=DIRECTION('',(0.,-1.,0.));
#32676=DIRECTION('center_axis',(0.287606238475944,-0.707106781186565,0.645974188021235));
#32677=DIRECTION('ref_axis',(0.287606238475958,0.70710678118653,0.645974188021267));
#32678=DIRECTION('center_axis',(0.,1.,0.));
#32679=DIRECTION('ref_axis',(1.,0.,0.));
#32680=DIRECTION('center_axis',(-0.415626937777456,-0.707106781186543,-0.572061402817688));
#32681=DIRECTION('ref_axis',(0.415626937777451,-0.707106781186551,0.572061402817681));
#32682=DIRECTION('',(0.,1.,0.));
#32683=DIRECTION('center_axis',(0.,1.,0.));
#32684=DIRECTION('ref_axis',(0.,0.,1.));
#32685=DIRECTION('',(0.,-1.,0.));
#32686=DIRECTION('center_axis',(0.415626937777451,-0.707106781186551,0.572061402817681));
#32687=DIRECTION('ref_axis',(0.415626937777455,0.707106781186544,0.572061402817687));
#32688=DIRECTION('center_axis',(0.,1.,0.));
#32689=DIRECTION('ref_axis',(1.,0.,0.));
#32690=DIRECTION('center_axis',(-0.525482745498762,-0.707106781186544,-0.473146789255818));
#32691=DIRECTION('ref_axis',(0.525482745498756,-0.707106781186551,0.473146789255813));
#32692=DIRECTION('',(0.,1.,0.));
#32693=DIRECTION('center_axis',(0.,1.,0.));
#32694=DIRECTION('ref_axis',(0.,0.,1.));
#32695=DIRECTION('',(0.,-1.,0.));
#32696=DIRECTION('center_axis',(0.525482745498748,-0.707106781186563,0.473146789255805));
#32697=DIRECTION('ref_axis',(0.52548274549877,0.707106781186532,0.473146789255825));
#32698=DIRECTION('center_axis',(0.,1.,0.));
#32699=DIRECTION('ref_axis',(1.,0.,0.));
#32700=DIRECTION('center_axis',(-0.612372435695801,-0.70710678118654,-0.353553390593278));
#32701=DIRECTION('ref_axis',(0.612372435695788,-0.707106781186555,0.35355339059327));
#32702=DIRECTION('',(0.,1.,0.));
#32703=DIRECTION('center_axis',(0.,1.,0.));
#32704=DIRECTION('ref_axis',(0.,0.,1.));
#32705=DIRECTION('',(0.,-1.,0.));
#32706=DIRECTION('center_axis',(0.612372435695798,-0.707106781186544,0.353553390593276));
#32707=DIRECTION('ref_axis',(0.612372435695791,0.707106781186551,0.353553390593272));
#32708=DIRECTION('center_axis',(0.,1.,0.));
#32709=DIRECTION('ref_axis',(1.,0.,0.));
#32710=DIRECTION('center_axis',(-0.672498511963955,-0.707106781186549,-0.21850801222441));
#32711=DIRECTION('ref_axis',(0.672498511963959,-0.707106781186546,0.218508012224411));
#32712=DIRECTION('',(0.,1.,0.));
#32713=DIRECTION('center_axis',(0.,1.,0.));
#32714=DIRECTION('ref_axis',(0.,0.,1.));
#32715=DIRECTION('',(0.,-1.,0.));
#32716=DIRECTION('center_axis',(0.672498511963958,-0.707106781186547,0.218508012224411));
#32717=DIRECTION('ref_axis',(0.672498511963957,0.707106781186548,0.218508012224411));
#32718=DIRECTION('center_axis',(0.,1.,0.));
#32719=DIRECTION('ref_axis',(1.,0.,0.));
#32720=DIRECTION('center_axis',(-0.703233176253405,-0.707106781186547,-0.0739127852035669));
#32721=DIRECTION('ref_axis',(0.703233176253403,-0.707106781186548,0.0739127852035668));
#32722=DIRECTION('',(0.,1.,0.));
#32723=DIRECTION('center_axis',(0.,1.,0.));
#32724=DIRECTION('ref_axis',(0.,0.,1.));
#32725=DIRECTION('',(0.,-1.,0.));
#32726=DIRECTION('center_axis',(0.703233176253404,-0.707106781186547,0.0739127852035669));
#32727=DIRECTION('ref_axis',(0.703233176253404,0.707106781186548,0.0739127852035668));
#32728=DIRECTION('center_axis',(0.,1.,0.));
#32729=DIRECTION('ref_axis',(1.,0.,0.));
#32730=DIRECTION('center_axis',(0.,1.,0.));
#32731=DIRECTION('ref_axis',(1.,0.,0.));
#32732=DIRECTION('center_axis',(0.703233176253406,0.707106781186546,0.073912785203567));
#32733=DIRECTION('ref_axis',(0.703233176253403,-0.707106781186549,0.0739127852035667));
#32734=DIRECTION('',(0.,-1.,0.));
#32735=DIRECTION('center_axis',(0.,-1.,0.));
#32736=DIRECTION('ref_axis',(0.,0.,1.));
#32737=DIRECTION('',(0.,1.,0.));
#32738=DIRECTION('center_axis',(-0.703233176253405,0.707106781186547,-0.0739127852035669));
#32739=DIRECTION('ref_axis',(0.703233176253403,0.707106781186548,0.0739127852035668));
#32740=DIRECTION('center_axis',(0.,1.,0.));
#32741=DIRECTION('ref_axis',(1.,0.,0.));
#32742=DIRECTION('center_axis',(0.672498511963959,0.707106781186546,0.218508012224411));
#32743=DIRECTION('ref_axis',(0.672498511963955,-0.707106781186549,0.21850801222441));
#32744=DIRECTION('',(0.,-1.,0.));
#32745=DIRECTION('center_axis',(0.,-1.,0.));
#32746=DIRECTION('ref_axis',(0.,0.,1.));
#32747=DIRECTION('',(0.,1.,0.));
#32748=DIRECTION('center_axis',(-0.672498511963952,0.707106781186553,-0.218508012224409));
#32749=DIRECTION('ref_axis',(0.672498511963962,0.707106781186542,0.218508012224412));
#32750=DIRECTION('center_axis',(0.,1.,0.));
#32751=DIRECTION('ref_axis',(1.,0.,0.));
#32752=DIRECTION('center_axis',(0.612372435695797,0.707106781186544,0.353553390593275));
#32753=DIRECTION('ref_axis',(0.612372435695792,-0.707106781186551,0.353553390593272));
#32754=DIRECTION('',(0.,-1.,0.));
#32755=DIRECTION('center_axis',(0.,-1.,0.));
#32756=DIRECTION('ref_axis',(0.,0.,1.));
#32757=DIRECTION('',(0.,1.,0.));
#32758=DIRECTION('center_axis',(-0.612372435695796,0.707106781186545,-0.353553390593275));
#32759=DIRECTION('ref_axis',(0.612372435695792,0.70710678118655,0.353553390593273));
#32760=DIRECTION('center_axis',(0.,1.,0.));
#32761=DIRECTION('ref_axis',(1.,0.,0.));
#32762=DIRECTION('center_axis',(0.525482745498763,0.707106781186542,0.473146789255819));
#32763=DIRECTION('ref_axis',(0.525482745498754,-0.707106781186553,0.473146789255811));
#32764=DIRECTION('',(0.,-1.,0.));
#32765=DIRECTION('center_axis',(0.,-1.,0.));
#32766=DIRECTION('ref_axis',(0.,0.,1.));
#32767=DIRECTION('',(0.,1.,0.));
#32768=DIRECTION('center_axis',(-0.525482745498759,0.707106781186547,-0.473146789255815));
#32769=DIRECTION('ref_axis',(0.525482745498758,0.707106781186548,0.473146789255815));
#32770=DIRECTION('center_axis',(0.,1.,0.));
#32771=DIRECTION('ref_axis',(1.,0.,0.));
#32772=DIRECTION('center_axis',(0.415626937777452,0.707106781186551,0.572061402817682));
#32773=DIRECTION('ref_axis',(0.415626937777455,-0.707106781186544,0.572061402817687));
#32774=DIRECTION('',(0.,-1.,0.));
#32775=DIRECTION('center_axis',(0.,-1.,0.));
#32776=DIRECTION('ref_axis',(0.,0.,1.));
#32777=DIRECTION('',(0.,1.,0.));
#32778=DIRECTION('center_axis',(-0.41562693777745,0.707106781186553,-0.57206140281768));
#32779=DIRECTION('ref_axis',(0.415626937777457,0.707106781186542,0.572061402817689));
#32780=DIRECTION('center_axis',(0.,1.,0.));
#32781=DIRECTION('ref_axis',(1.,0.,0.));
#32782=DIRECTION('center_axis',(0.28760623847595,0.707106781186549,0.64597418802125));
#32783=DIRECTION('ref_axis',(0.287606238475951,-0.707106781186546,0.645974188021252));
#32784=DIRECTION('',(0.,-1.,0.));
#32785=DIRECTION('center_axis',(0.,-1.,0.));
#32786=DIRECTION('ref_axis',(0.,0.,1.));
#32787=DIRECTION('',(0.,1.,0.));
#32788=DIRECTION('center_axis',(-0.28760623847595,0.707106781186549,-0.64597418802125));
#32789=DIRECTION('ref_axis',(0.287606238475951,0.707106781186546,0.645974188021252));
#32790=DIRECTION('center_axis',(0.,1.,0.));
#32791=DIRECTION('ref_axis',(1.,0.,0.));
#32792=DIRECTION('center_axis',(0.147015766465199,0.707106781186544,0.691654801480229));
#32793=DIRECTION('ref_axis',(0.147015766465198,-0.707106781186551,0.691654801480222));
#32794=DIRECTION('',(0.,-1.,0.));
#32795=DIRECTION('center_axis',(0.,-1.,0.));
#32796=DIRECTION('ref_axis',(0.,0.,1.));
#32797=DIRECTION('',(0.,1.,0.));
#32798=DIRECTION('center_axis',(-0.147015766465199,0.707106781186546,-0.691654801480227));
#32799=DIRECTION('ref_axis',(0.147015766465198,0.707106781186549,0.691654801480224));
#32800=DIRECTION('center_axis',(0.,1.,0.));
#32801=DIRECTION('ref_axis',(1.,0.,0.));
#32802=DIRECTION('center_axis',(0.,0.707106781186547,0.707106781186548));
#32803=DIRECTION('ref_axis',(0.,-0.707106781186548,0.707106781186547));
#32804=DIRECTION('',(0.,-1.,0.));
#32805=DIRECTION('center_axis',(0.,-1.,0.));
#32806=DIRECTION('ref_axis',(0.,0.,1.));
#32807=DIRECTION('',(0.,1.,0.));
#32808=DIRECTION('center_axis',(0.,0.707106781186547,-0.707106781186548));
#32809=DIRECTION('ref_axis',(0.,0.707106781186548,0.707106781186547));
#32810=DIRECTION('center_axis',(0.,1.,0.));
#32811=DIRECTION('ref_axis',(1.,0.,0.));
#32812=DIRECTION('center_axis',(-0.147015766465199,0.707106781186546,0.691654801480227));
#32813=DIRECTION('ref_axis',(-0.147015766465199,-0.707106781186549,0.691654801480224));
#32814=DIRECTION('',(0.,-1.,0.));
#32815=DIRECTION('center_axis',(0.,-1.,0.));
#32816=DIRECTION('ref_axis',(0.,0.,1.));
#32817=DIRECTION('',(0.,1.,0.));
#32818=DIRECTION('center_axis',(0.147015766465199,0.707106781186547,-0.691654801480226));
#32819=DIRECTION('ref_axis',(-0.147015766465199,0.707106781186549,0.691654801480225));
#32820=DIRECTION('center_axis',(0.,1.,0.));
#32821=DIRECTION('ref_axis',(1.,0.,0.));
#32822=DIRECTION('center_axis',(-0.287606238475952,0.707106781186546,0.645974188021252));
#32823=DIRECTION('ref_axis',(-0.287606238475951,-0.707106781186549,0.64597418802125));
#32824=DIRECTION('',(0.,-1.,0.));
#32825=DIRECTION('center_axis',(0.,-1.,0.));
#32826=DIRECTION('ref_axis',(0.,0.,1.));
#32827=DIRECTION('',(0.,1.,0.));
#32828=DIRECTION('center_axis',(0.287606238475951,0.707106781186549,-0.64597418802125));
#32829=DIRECTION('ref_axis',(-0.287606238475952,0.707106781186546,0.645974188021252));
#32830=DIRECTION('center_axis',(0.,1.,0.));
#32831=DIRECTION('ref_axis',(1.,0.,0.));
#32832=DIRECTION('center_axis',(-0.415626937777453,0.707106781186548,0.572061402817684));
#32833=DIRECTION('ref_axis',(-0.415626937777454,-0.707106781186547,0.572061402817684));
#32834=DIRECTION('',(0.,-1.,0.));
#32835=DIRECTION('center_axis',(0.,-1.,0.));
#32836=DIRECTION('ref_axis',(0.,0.,1.));
#32837=DIRECTION('',(0.,1.,0.));
#32838=DIRECTION('center_axis',(0.415626937777454,0.707106781186546,-0.572061402817685));
#32839=DIRECTION('ref_axis',(-0.415626937777453,0.707106781186549,0.572061402817683));
#32840=DIRECTION('center_axis',(0.,1.,0.));
#32841=DIRECTION('ref_axis',(1.,0.,0.));
#32842=DIRECTION('center_axis',(-0.525482745498764,0.707106781186541,0.473146789255819));
#32843=DIRECTION('ref_axis',(-0.525482745498755,-0.707106781186554,0.473146789255811));
#32844=DIRECTION('',(0.,-1.,0.));
#32845=DIRECTION('center_axis',(0.,-1.,0.));
#32846=DIRECTION('ref_axis',(0.,0.,1.));
#32847=DIRECTION('',(0.,1.,0.));
#32848=DIRECTION('center_axis',(0.52548274549876,0.707106781186547,-0.473146789255815));
#32849=DIRECTION('ref_axis',(-0.525482745498759,0.707106781186548,0.473146789255814));
#32850=DIRECTION('center_axis',(0.,1.,0.));
#32851=DIRECTION('ref_axis',(1.,0.,0.));
#32852=DIRECTION('center_axis',(-0.612372435695797,0.707106781186545,0.353553390593274));
#32853=DIRECTION('ref_axis',(-0.612372435695793,-0.70710678118655,0.353553390593272));
#32854=DIRECTION('',(0.,-1.,0.));
#32855=DIRECTION('center_axis',(0.,-1.,0.));
#32856=DIRECTION('ref_axis',(0.,0.,1.));
#32857=DIRECTION('',(0.,1.,0.));
#32858=DIRECTION('center_axis',(0.612372435695795,0.707106781186547,-0.353553390593274));
#32859=DIRECTION('ref_axis',(-0.612372435695794,0.707106781186548,0.353553390593273));
#32860=DIRECTION('center_axis',(0.,1.,0.));
#32861=DIRECTION('ref_axis',(1.,0.,0.));
#32862=DIRECTION('center_axis',(-0.672498511963955,0.70710678118655,0.21850801222441));
#32863=DIRECTION('ref_axis',(-0.672498511963959,-0.707106781186545,0.218508012224411));
#32864=DIRECTION('',(0.,-1.,0.));
#32865=DIRECTION('center_axis',(0.,-1.,0.));
#32866=DIRECTION('ref_axis',(0.,0.,1.));
#32867=DIRECTION('',(0.,1.,0.));
#32868=DIRECTION('center_axis',(0.672498511963957,0.707106781186548,-0.21850801222441));
#32869=DIRECTION('ref_axis',(-0.672498511963958,0.707106781186547,0.218508012224411));
#32870=DIRECTION('center_axis',(0.,1.,0.));
#32871=DIRECTION('ref_axis',(1.,0.,0.));
#32872=DIRECTION('center_axis',(-0.703233176253405,0.707106781186547,0.0739127852035665));
#32873=DIRECTION('ref_axis',(-0.703233176253403,-0.707106781186548,0.0739127852035663));
#32874=DIRECTION('',(0.,-1.,0.));
#32875=DIRECTION('center_axis',(0.,-1.,0.));
#32876=DIRECTION('ref_axis',(0.,0.,1.));
#32877=DIRECTION('',(0.,1.,0.));
#32878=DIRECTION('center_axis',(0.703233176253404,0.707106781186547,-0.0739127852035664));
#32879=DIRECTION('ref_axis',(-0.703233176253404,0.707106781186548,0.0739127852035664));
#32880=DIRECTION('center_axis',(0.,1.,0.));
#32881=DIRECTION('ref_axis',(1.,0.,0.));
#32882=DIRECTION('center_axis',(-0.703233176253405,0.707106781186547,-0.0739127852035674));
#32883=DIRECTION('ref_axis',(0.703233176253403,0.707106781186548,0.0739127852035672));
#32884=DIRECTION('',(0.,-1.,0.));
#32885=DIRECTION('center_axis',(0.,-1.,0.));
#32886=DIRECTION('ref_axis',(0.,0.,1.));
#32887=DIRECTION('',(0.,1.,0.));
#32888=DIRECTION('center_axis',(0.703233176253406,0.707106781186546,0.0739127852035675));
#32889=DIRECTION('ref_axis',(0.703233176253402,-0.707106781186549,0.0739127852035671));
#32890=DIRECTION('center_axis',(0.,1.,0.));
#32891=DIRECTION('ref_axis',(1.,0.,0.));
#32892=DIRECTION('center_axis',(-0.672498511963957,0.707106781186548,-0.218508012224411));
#32893=DIRECTION('ref_axis',(0.672498511963958,0.707106781186547,0.218508012224411));
#32894=DIRECTION('',(0.,-1.,0.));
#32895=DIRECTION('center_axis',(0.,-1.,0.));
#32896=DIRECTION('ref_axis',(0.,0.,1.));
#32897=DIRECTION('',(0.,1.,0.));
#32898=DIRECTION('center_axis',(0.672498511963954,0.707106781186551,0.21850801222441));
#32899=DIRECTION('ref_axis',(0.672498511963961,-0.707106781186544,0.218508012224412));
#32900=DIRECTION('center_axis',(0.,1.,0.));
#32901=DIRECTION('ref_axis',(1.,0.,0.));
#32902=DIRECTION('center_axis',(-0.612372435695796,0.707106781186545,-0.353553390593275));
#32903=DIRECTION('ref_axis',(0.612372435695792,0.70710678118655,0.353553390593273));
#32904=DIRECTION('',(0.,-1.,0.));
#32905=DIRECTION('center_axis',(0.,-1.,0.));
#32906=DIRECTION('ref_axis',(0.,0.,1.));
#32907=DIRECTION('',(0.,1.,0.));
#32908=DIRECTION('center_axis',(0.612372435695793,0.707106781186549,0.353553390593274));
#32909=DIRECTION('ref_axis',(0.612372435695795,-0.707106781186547,0.353553390593275));
#32910=DIRECTION('center_axis',(0.,1.,0.));
#32911=DIRECTION('ref_axis',(1.,0.,0.));
#32912=DIRECTION('center_axis',(-0.525482745498762,0.707106781186543,-0.473146789255818));
#32913=DIRECTION('ref_axis',(0.525482745498755,0.707106781186552,0.473146789255812));
#32914=DIRECTION('',(0.,-1.,0.));
#32915=DIRECTION('center_axis',(0.,-1.,0.));
#32916=DIRECTION('ref_axis',(0.,0.,1.));
#32917=DIRECTION('',(0.,1.,0.));
#32918=DIRECTION('center_axis',(0.525482745498759,0.707106781186547,0.473146789255815));
#32919=DIRECTION('ref_axis',(0.525482745498758,-0.707106781186548,0.473146789255815));
#32920=DIRECTION('center_axis',(0.,1.,0.));
#32921=DIRECTION('ref_axis',(1.,0.,0.));
#32922=DIRECTION('center_axis',(-0.415626937777449,0.707106781186555,-0.572061402817678));
#32923=DIRECTION('ref_axis',(0.415626937777458,0.70710678118654,0.57206140281769));
#32924=DIRECTION('',(0.,-1.,0.));
#32925=DIRECTION('center_axis',(0.,-1.,0.));
#32926=DIRECTION('ref_axis',(0.,0.,1.));
#32927=DIRECTION('',(0.,1.,0.));
#32928=DIRECTION('center_axis',(0.415626937777453,0.707106781186548,0.572061402817684));
#32929=DIRECTION('ref_axis',(0.415626937777453,-0.707106781186547,0.572061402817684));
#32930=DIRECTION('center_axis',(0.,1.,0.));
#32931=DIRECTION('ref_axis',(1.,0.,0.));
#32932=DIRECTION('center_axis',(-0.28760623847595,0.707106781186549,-0.64597418802125));
#32933=DIRECTION('ref_axis',(0.287606238475951,0.707106781186546,0.645974188021252));
#32934=DIRECTION('',(0.,-1.,0.));
#32935=DIRECTION('center_axis',(0.,-1.,0.));
#32936=DIRECTION('ref_axis',(0.,0.,1.));
#32937=DIRECTION('',(0.,1.,0.));
#32938=DIRECTION('center_axis',(0.287606238475948,0.707106781186554,0.645974188021245));
#32939=DIRECTION('ref_axis',(0.287606238475953,-0.707106781186541,0.645974188021257));
#32940=DIRECTION('center_axis',(0.,1.,0.));
#32941=DIRECTION('ref_axis',(1.,0.,0.));
#32942=DIRECTION('center_axis',(-0.147015766465198,0.707106781186547,-0.691654801480227));
#32943=DIRECTION('ref_axis',(0.147015766465198,0.707106781186548,0.691654801480225));
#32944=DIRECTION('',(0.,-1.,0.));
#32945=DIRECTION('center_axis',(0.,-1.,0.));
#32946=DIRECTION('ref_axis',(0.,0.,1.));
#32947=DIRECTION('',(0.,1.,0.));
#32948=DIRECTION('center_axis',(0.147015766465198,0.707106781186547,0.691654801480226));
#32949=DIRECTION('ref_axis',(0.147015766465198,-0.707106781186548,0.691654801480225));
#32950=DIRECTION('center_axis',(0.,1.,0.));
#32951=DIRECTION('ref_axis',(1.,0.,0.));
#32952=DIRECTION('center_axis',(8.65956056235494E-17,0.707106781186547,
-0.707106781186548));
#32953=DIRECTION('ref_axis',(0.,0.707106781186548,0.707106781186547));
#32954=DIRECTION('',(0.,-1.,0.));
#32955=DIRECTION('center_axis',(0.,-1.,0.));
#32956=DIRECTION('ref_axis',(0.,0.,1.));
#32957=DIRECTION('',(0.,1.,0.));
#32958=DIRECTION('center_axis',(-8.65956056235494E-17,0.707106781186547,
0.707106781186548));
#32959=DIRECTION('ref_axis',(0.,-0.707106781186548,0.707106781186547));
#32960=DIRECTION('center_axis',(0.,1.,0.));
#32961=DIRECTION('ref_axis',(1.,0.,0.));
#32962=DIRECTION('center_axis',(0.147015766465199,0.707106781186547,-0.691654801480226));
#32963=DIRECTION('ref_axis',(-0.147015766465199,0.707106781186548,0.691654801480225));
#32964=DIRECTION('',(0.,-1.,0.));
#32965=DIRECTION('center_axis',(0.,-1.,0.));
#32966=DIRECTION('ref_axis',(0.,0.,1.));
#32967=DIRECTION('',(0.,1.,0.));
#32968=DIRECTION('center_axis',(-0.147015766465199,0.707106781186549,0.691654801480225));
#32969=DIRECTION('ref_axis',(-0.147015766465199,-0.707106781186547,0.691654801480227));
#32970=DIRECTION('center_axis',(0.,1.,0.));
#32971=DIRECTION('ref_axis',(1.,0.,0.));
#32972=DIRECTION('center_axis',(0.287606238475951,0.707106781186546,-0.645974188021252));
#32973=DIRECTION('ref_axis',(-0.28760623847595,0.707106781186549,0.64597418802125));
#32974=DIRECTION('',(0.,-1.,0.));
#32975=DIRECTION('center_axis',(0.,-1.,0.));
#32976=DIRECTION('ref_axis',(0.,0.,1.));
#32977=DIRECTION('',(0.,1.,0.));
#32978=DIRECTION('center_axis',(-0.287606238475952,0.707106781186545,0.645974188021253));
#32979=DIRECTION('ref_axis',(-0.28760623847595,-0.70710678118655,0.645974188021249));
#32980=DIRECTION('center_axis',(0.,1.,0.));
#32981=DIRECTION('ref_axis',(1.,0.,0.));
#32982=DIRECTION('center_axis',(0.415626937777453,0.707106781186548,-0.572061402817684));
#32983=DIRECTION('ref_axis',(-0.415626937777454,0.707106781186547,0.572061402817684));
#32984=DIRECTION('',(0.,-1.,0.));
#32985=DIRECTION('center_axis',(0.,-1.,0.));
#32986=DIRECTION('ref_axis',(0.,0.,1.));
#32987=DIRECTION('',(0.,1.,0.));
#32988=DIRECTION('center_axis',(-0.415626937777449,0.707106781186555,0.572061402817678));
#32989=DIRECTION('ref_axis',(-0.415626937777458,-0.70710678118654,0.57206140281769));
#32990=DIRECTION('center_axis',(0.,1.,0.));
#32991=DIRECTION('ref_axis',(1.,0.,0.));
#32992=DIRECTION('center_axis',(0.525482745498762,0.707106781186544,-0.473146789255817));
#32993=DIRECTION('ref_axis',(-0.525482745498757,0.707106781186551,0.473146789255813));
#32994=DIRECTION('',(0.,-1.,0.));
#32995=DIRECTION('center_axis',(0.,-1.,0.));
#32996=DIRECTION('ref_axis',(0.,0.,1.));
#32997=DIRECTION('',(0.,1.,0.));
#32998=DIRECTION('center_axis',(-0.525482745498759,0.707106781186547,0.473146789255815));
#32999=DIRECTION('ref_axis',(-0.525482745498759,-0.707106781186548,0.473146789255814));
#33000=DIRECTION('center_axis',(0.,1.,0.));
#33001=DIRECTION('ref_axis',(1.,0.,0.));
#33002=DIRECTION('center_axis',(0.612372435695796,0.707106781186546,-0.353553390593274));
#33003=DIRECTION('ref_axis',(-0.612372435695793,0.707106781186549,0.353553390593273));
#33004=DIRECTION('',(0.,-1.,0.));
#33005=DIRECTION('center_axis',(0.,-1.,0.));
#33006=DIRECTION('ref_axis',(0.,0.,1.));
#33007=DIRECTION('center_axis',(0.672498511963959,0.707106781186546,-0.218508012224411));
#33008=DIRECTION('ref_axis',(-0.309016994374947,0.,-0.951056516295154));
#33009=DIRECTION('',(-0.309016994374947,0.,-0.951056516295154));
#33010=DIRECTION('',(0.309016994374947,0.,0.951056516295154));
#33011=DIRECTION('',(0.370681690811013,-0.577350269189625,-0.727503780584098));
#33012=DIRECTION('center_axis',(-0.218508012224414,0.707106781186536,-0.672498511963968));
#33013=DIRECTION('ref_axis',(-0.951056516295154,0.,0.309016994374947));
#33014=DIRECTION('',(0.951056516295154,0.,-0.309016994374947));
#33015=DIRECTION('',(-0.727503780584107,-0.57735026918963,-0.37068169081099));
#33016=DIRECTION('',(-0.951056516295154,0.,0.309016994374947));
#33017=DIRECTION('center_axis',(-0.672498511963953,0.707106781186552,0.218508012224409));
#33018=DIRECTION('ref_axis',(0.309016994374947,0.,0.951056516295154));
#33019=DIRECTION('',(-0.309016994374947,0.,-0.951056516295154));
#33020=DIRECTION('',(0.309016994374947,0.,0.951056516295154));
#33021=DIRECTION('center_axis',(-0.951056516295154,0.,0.309016994374947));
#33022=DIRECTION('ref_axis',(-0.309016994374947,0.,-0.951056516295154));
#33023=DIRECTION('',(0.,-1.,0.));
#33024=DIRECTION('',(-0.309016994374947,0.,-0.951056516295154));
#33025=DIRECTION('center_axis',(0.309016994374947,0.,0.951056516295154));
#33026=DIRECTION('ref_axis',(-0.951056516295154,0.,0.309016994374947));
#33027=DIRECTION('',(0.,-1.,0.));
#33028=DIRECTION('',(-0.951056516295154,0.,0.309016994374947));
#33029=DIRECTION('center_axis',(0.951056516295154,0.,-0.309016994374947));
#33030=DIRECTION('ref_axis',(0.309016994374947,0.,0.951056516295154));
#33031=DIRECTION('',(0.309016994374947,0.,0.951056516295154));
#33032=DIRECTION('center_axis',(0.703233176253404,0.707106781186548,-0.0739127852035666));
#33033=DIRECTION('ref_axis',(-0.104528463267653,0.,-0.994521895368273));
#33034=DIRECTION('',(-0.104528463267653,0.,-0.994521895368273));
#33035=DIRECTION('',(0.104528463267653,0.,0.994521895368273));
#33036=DIRECTION('',(0.513837947600291,-0.577350269189624,-0.634537020411409));
#33037=DIRECTION('center_axis',(-0.0739127852035671,0.707106781186543,-0.703233176253409));
#33038=DIRECTION('ref_axis',(-0.994521895368273,0.,0.104528463267653));
#33039=DIRECTION('',(0.994521895368273,0.,-0.104528463267653));
#33040=DIRECTION('',(-0.634537020411409,-0.577350269189628,-0.513837947600288));
#33041=DIRECTION('',(-0.994521895368273,0.,0.104528463267653));
#33042=DIRECTION('center_axis',(-0.703233176253404,0.707106781186547,0.0739127852035666));
#33043=DIRECTION('ref_axis',(0.104528463267653,0.,0.994521895368273));
#33044=DIRECTION('',(-0.104528463267653,0.,-0.994521895368273));
#33045=DIRECTION('',(0.104528463267653,0.,0.994521895368273));
#33046=DIRECTION('center_axis',(-0.994521895368273,0.,0.104528463267653));
#33047=DIRECTION('ref_axis',(-0.104528463267653,0.,-0.994521895368273));
#33048=DIRECTION('',(0.,-1.,0.));
#33049=DIRECTION('',(-0.104528463267653,0.,-0.994521895368273));
#33050=DIRECTION('center_axis',(0.104528463267653,0.,0.994521895368273));
#33051=DIRECTION('ref_axis',(-0.994521895368273,0.,0.104528463267653));
#33052=DIRECTION('',(0.,-1.,0.));
#33053=DIRECTION('',(-0.994521895368273,0.,0.104528463267653));
#33054=DIRECTION('center_axis',(0.994521895368273,0.,-0.104528463267653));
#33055=DIRECTION('ref_axis',(0.104528463267653,0.,0.994521895368273));
#33056=DIRECTION('',(0.104528463267653,0.,0.994521895368273));
#33057=DIRECTION('center_axis',(0.703233176253406,0.707106781186546,0.073912785203567));
#33058=DIRECTION('ref_axis',(0.104528463267654,0.,-0.994521895368273));
#33059=DIRECTION('',(0.104528463267654,0.,-0.994521895368273));
#33060=DIRECTION('',(-0.104528463267654,0.,0.994521895368273));
#33061=DIRECTION('',(0.634537020411404,-0.577350269189624,-0.513837947600297));
#33062=DIRECTION('center_axis',(0.0739127852035657,0.707106781186559,-0.703233176253393));
#33063=DIRECTION('ref_axis',(-0.994521895368273,0.,-0.104528463267654));
#33064=DIRECTION('',(0.994521895368273,0.,0.104528463267654));
#33065=DIRECTION('',(-0.513837947600281,-0.577350269189616,-0.634537020411425));
#33066=DIRECTION('',(-0.994521895368273,0.,-0.104528463267654));
#33067=DIRECTION('center_axis',(-0.703233176253405,0.707106781186547,-0.0739127852035669));
#33068=DIRECTION('ref_axis',(-0.104528463267654,0.,0.994521895368273));
#33069=DIRECTION('',(0.104528463267654,0.,-0.994521895368273));
#33070=DIRECTION('',(-0.104528463267654,0.,0.994521895368273));
#33071=DIRECTION('center_axis',(-0.994521895368273,0.,-0.104528463267654));
#33072=DIRECTION('ref_axis',(0.104528463267654,0.,-0.994521895368273));
#33073=DIRECTION('',(0.,-1.,0.));
#33074=DIRECTION('',(0.104528463267654,0.,-0.994521895368273));
#33075=DIRECTION('center_axis',(-0.104528463267654,0.,0.994521895368273));
#33076=DIRECTION('ref_axis',(-0.994521895368273,0.,-0.104528463267654));
#33077=DIRECTION('',(0.,-1.,0.));
#33078=DIRECTION('',(-0.994521895368273,0.,-0.104528463267654));
#33079=DIRECTION('center_axis',(0.994521895368273,0.,0.104528463267654));
#33080=DIRECTION('ref_axis',(-0.104528463267654,0.,0.994521895368273));
#33081=DIRECTION('',(-0.104528463267654,0.,0.994521895368273));
#33082=DIRECTION('center_axis',(0.672498511963959,0.707106781186546,0.218508012224411));
#33083=DIRECTION('ref_axis',(0.309016994374947,0.,-0.951056516295153));
#33084=DIRECTION('',(0.309016994374948,0.,-0.951056516295154));
#33085=DIRECTION('',(-0.309016994374948,0.,0.951056516295154));
#33086=DIRECTION('',(0.727503780584104,-0.577350269189638,-0.370681690810982));
#33087=DIRECTION('center_axis',(0.218508012224414,0.707106781186536,-0.672498511963969));
#33088=DIRECTION('ref_axis',(-0.951056516295153,0.,-0.309016994374947));
#33089=DIRECTION('',(0.951056516295153,0.,0.309016994374947));
#33090=DIRECTION('',(0.370681690811026,0.577350269189629,0.727503780584088));
#33091=DIRECTION('',(-0.951056516295154,0.,-0.309016994374948));
#33092=DIRECTION('center_axis',(-0.951056516295154,0.,-0.309016994374948));
#33093=DIRECTION('ref_axis',(0.309016994374948,0.,-0.951056516295154));
#33094=DIRECTION('',(0.,-1.,0.));
#33095=DIRECTION('',(0.309016994374948,0.,-0.951056516295154));
#33096=DIRECTION('center_axis',(-0.309016994374948,0.,0.951056516295154));
#33097=DIRECTION('ref_axis',(-0.951056516295154,0.,-0.309016994374948));
#33098=DIRECTION('',(0.,-1.,0.));
#33099=DIRECTION('',(-0.951056516295154,0.,-0.309016994374948));
#33100=DIRECTION('center_axis',(-0.672498511963952,0.707106781186553,-0.218508012224409));
#33101=DIRECTION('ref_axis',(-0.309016994374948,0.,0.951056516295154));
#33102=DIRECTION('',(-0.309016994374948,0.,0.951056516295154));
#33103=DIRECTION('',(0.309016994374948,0.,-0.951056516295154));
#33104=DIRECTION('center_axis',(0.,1.,0.));
#33105=DIRECTION('ref_axis',(0.,0.,1.));
#33106=DIRECTION('',(0.866025403784439,0.,-0.5));
#33107=DIRECTION('',(0.5,0.,0.866025403784439));
#33108=DIRECTION('',(-0.669130606358858,0.,-0.743144825477394));
#33109=DIRECTION('',(0.743144825477394,0.,-0.669130606358858));
#33110=DIRECTION('',(0.669130606358858,0.,0.743144825477394));
#33111=DIRECTION('',(-0.809016994374947,0.,-0.587785252292473));
#33112=DIRECTION('',(0.587785252292473,0.,-0.809016994374947));
#33113=DIRECTION('',(0.809016994374947,0.,0.587785252292473));
#33114=DIRECTION('',(-0.913545457642601,0.,-0.4067366430758));
#33115=DIRECTION('',(0.4067366430758,0.,-0.913545457642601));
#33116=DIRECTION('',(0.913545457642601,0.,0.4067366430758));
#33117=DIRECTION('',(-0.978147600733805,0.,-0.20791169081776));
#33118=DIRECTION('',(0.20791169081776,0.,-0.978147600733805));
#33119=DIRECTION('',(0.978147600733805,0.,0.20791169081776));
#33120=DIRECTION('',(-1.,0.,-1.22464679914735E-16));
#33121=DIRECTION('',(1.22464679914735E-16,0.,-1.));
#33122=DIRECTION('',(1.,0.,1.22464679914735E-16));
#33123=DIRECTION('',(-0.978147600733806,0.,0.207911690817759));
#33124=DIRECTION('',(-0.207911690817759,0.,-0.978147600733806));
#33125=DIRECTION('',(0.978147600733806,0.,-0.207911690817759));
#33126=DIRECTION('',(-0.913545457642601,0.,0.4067366430758));
#33127=DIRECTION('',(-0.4067366430758,0.,-0.913545457642601));
#33128=DIRECTION('',(0.913545457642601,0.,-0.4067366430758));
#33129=DIRECTION('',(-0.809016994374947,0.,0.587785252292473));
#33130=DIRECTION('',(-0.587785252292473,0.,-0.809016994374947));
#33131=DIRECTION('',(0.809016994374947,0.,-0.587785252292473));
#33132=DIRECTION('',(-0.669130606358858,0.,0.743144825477394));
#33133=DIRECTION('',(-0.743144825477394,0.,-0.669130606358858));
#33134=DIRECTION('',(0.669130606358858,0.,-0.743144825477394));
#33135=DIRECTION('',(-0.5,0.,0.866025403784438));
#33136=DIRECTION('',(-0.866025403784438,0.,-0.5));
#33137=DIRECTION('',(0.5,0.,-0.866025403784438));
#33138=DIRECTION('',(-0.309016994374948,0.,0.951056516295153));
#33139=DIRECTION('',(-0.951056516295153,0.,-0.309016994374948));
#33140=DIRECTION('',(0.309016994374948,0.,-0.951056516295153));
#33141=DIRECTION('',(-0.104528463267654,0.,0.994521895368273));
#33142=DIRECTION('',(-0.994521895368273,0.,-0.104528463267654));
#33143=DIRECTION('',(0.104528463267654,0.,-0.994521895368273));
#33144=DIRECTION('',(0.104528463267653,0.,0.994521895368273));
#33145=DIRECTION('',(-0.994521895368273,0.,0.104528463267653));
#33146=DIRECTION('',(-0.104528463267653,0.,-0.994521895368273));
#33147=DIRECTION('',(0.309016994374947,0.,0.951056516295154));
#33148=DIRECTION('',(-0.951056516295154,0.,0.309016994374947));
#33149=DIRECTION('',(-0.309016994374947,0.,-0.951056516295154));
#33150=DIRECTION('',(0.499999999999999,0.,0.866025403784439));
#33151=DIRECTION('',(-0.866025403784439,0.,0.499999999999999));
#33152=DIRECTION('',(-0.499999999999999,0.,-0.866025403784439));
#33153=DIRECTION('',(0.669130606358858,0.,0.743144825477395));
#33154=DIRECTION('',(-0.743144825477395,0.,0.669130606358858));
#33155=DIRECTION('',(-0.669130606358858,0.,-0.743144825477395));
#33156=DIRECTION('',(0.809016994374947,0.,0.587785252292473));
#33157=DIRECTION('',(-0.587785252292473,0.,0.809016994374947));
#33158=DIRECTION('',(-0.809016994374947,0.,-0.587785252292473));
#33159=DIRECTION('',(0.913545457642601,0.,0.406736643075801));
#33160=DIRECTION('',(-0.406736643075801,0.,0.913545457642601));
#33161=DIRECTION('',(-0.913545457642601,0.,-0.406736643075801));
#33162=DIRECTION('',(0.978147600733805,0.,0.20791169081776));
#33163=DIRECTION('',(-0.20791169081776,0.,0.978147600733805));
#33164=DIRECTION('',(-0.978147600733805,0.,-0.20791169081776));
#33165=DIRECTION('',(1.,0.,0.));
#33166=DIRECTION('',(0.,0.,1.));
#33167=DIRECTION('',(-1.,0.,0.));
#33168=DIRECTION('',(0.978147600733806,0.,-0.207911690817759));
#33169=DIRECTION('',(0.207911690817759,0.,0.978147600733806));
#33170=DIRECTION('',(-0.978147600733806,0.,0.207911690817759));
#33171=DIRECTION('',(0.913545457642601,0.,-0.4067366430758));
#33172=DIRECTION('',(0.4067366430758,0.,0.913545457642601));
#33173=DIRECTION('',(-0.913545457642601,0.,0.4067366430758));
#33174=DIRECTION('',(0.809016994374947,0.,-0.587785252292473));
#33175=DIRECTION('',(0.587785252292473,0.,0.809016994374947));
#33176=DIRECTION('',(-0.809016994374947,0.,0.587785252292473));
#33177=DIRECTION('',(0.669130606358858,0.,-0.743144825477394));
#33178=DIRECTION('',(0.743144825477394,0.,0.669130606358858));
#33179=DIRECTION('',(-0.669130606358858,0.,0.743144825477394));
#33180=DIRECTION('',(0.5,0.,-0.866025403784439));
#33181=DIRECTION('',(0.866025403784439,0.,0.5));
#33182=DIRECTION('',(-0.5,0.,0.866025403784439));
#33183=DIRECTION('',(-1.,0.,0.));
#33184=DIRECTION('center_axis',(0.,1.,0.));
#33185=DIRECTION('ref_axis',(1.,0.,0.));
#33186=DIRECTION('',(-1.,0.,0.));
#33187=DIRECTION('',(0.,0.,-1.));
#33188=DIRECTION('',(1.,0.,0.));
#33189=DIRECTION('center_axis',(0.,1.,0.));
#33190=DIRECTION('ref_axis',(1.,0.,0.));
#33191=DIRECTION('',(1.,0.,0.));
#33192=DIRECTION('',(0.,0.,1.));
#33193=DIRECTION('center_axis',(0.612372435695797,0.707106781186544,0.353553390593275));
#33194=DIRECTION('ref_axis',(0.5,0.,-0.866025403784439));
#33195=DIRECTION('',(0.5,0.,-0.866025403784439));
#33196=DIRECTION('',(0.788675134594807,-0.577350269189639,-0.211324865405175));
#33197=DIRECTION('center_axis',(0.353553390593278,0.70710678118654,-0.612372435695801));
#33198=DIRECTION('ref_axis',(-0.866025403784439,0.,-0.5));
#33199=DIRECTION('',(-0.211324865405192,-0.577350269189633,-0.788675134594806));
#33200=DIRECTION('',(-0.866025403784439,0.,-0.5));
#33201=DIRECTION('center_axis',(-0.612372435695796,0.707106781186545,-0.353553390593275));
#33202=DIRECTION('ref_axis',(-0.5,0.,0.866025403784439));
#33203=DIRECTION('',(-0.5,0.,0.866025403784439));
#33204=DIRECTION('center_axis',(0.525482745498763,0.707106781186542,0.473146789255819));
#33205=DIRECTION('ref_axis',(0.669130606358858,0.,-0.743144825477394));
#33206=DIRECTION('',(0.669130606358858,0.,-0.743144825477394));
#33207=DIRECTION('',(0.815377600740549,-0.577350269189636,-0.0427321293319401));
#33208=DIRECTION('center_axis',(0.473146789255821,0.707106781186539,-0.525482745498766));
#33209=DIRECTION('ref_axis',(-0.743144825477394,0.,-0.669130606358858));
#33210=DIRECTION('',(-0.0427321293319529,-0.577350269189635,-0.815377600740548));
#33211=DIRECTION('',(-0.743144825477394,0.,-0.669130606358858));
#33212=DIRECTION('center_axis',(-0.525482745498759,0.707106781186547,-0.473146789255815));
#33213=DIRECTION('ref_axis',(-0.669130606358858,0.,0.743144825477394));
#33214=DIRECTION('',(-0.669130606358858,0.,0.743144825477394));
#33215=DIRECTION('center_axis',(0.415626937777452,0.707106781186551,0.572061402817682));
#33216=DIRECTION('ref_axis',(0.809016994374947,0.,-0.587785252292473));
#33217=DIRECTION('',(0.809016994374947,0.,-0.587785252292473));
#33218=DIRECTION('',(0.806444153118105,-0.577350269189629,0.127728205844619));
#33219=DIRECTION('center_axis',(0.572061402817692,0.707106781186538,-0.415626937777459));
#33220=DIRECTION('ref_axis',(-0.587785252292473,0.,-0.809016994374947));
#33221=DIRECTION('',(0.127728205844585,-0.577350269189623,-0.806444153118115));
#33222=DIRECTION('',(-0.587785252292473,0.,-0.809016994374947));
#33223=DIRECTION('center_axis',(-0.41562693777745,0.707106781186553,-0.57206140281768));
#33224=DIRECTION('ref_axis',(-0.809016994374947,0.,0.587785252292473));
#33225=DIRECTION('',(-0.809016994374947,0.,0.587785252292473));
#33226=DIRECTION('center_axis',(0.28760623847595,0.707106781186549,0.64597418802125));
#33227=DIRECTION('ref_axis',(0.913545457642601,0.,-0.4067366430758));
#33228=DIRECTION('',(0.913545457642601,0.,-0.4067366430758));
#33229=DIRECTION('',(0.76226522625601,-0.577350269189626,0.292606205517827));
#33230=DIRECTION('center_axis',(0.645974188021254,0.707106781186545,-0.287606238475952));
#33231=DIRECTION('ref_axis',(-0.4067366430758,0.,-0.913545457642601));
#33232=DIRECTION('',(0.292606205517814,-0.577350269189627,-0.762265226256014));
#33233=DIRECTION('',(-0.4067366430758,0.,-0.913545457642601));
#33234=DIRECTION('center_axis',(-0.28760623847595,0.707106781186549,-0.64597418802125));
#33235=DIRECTION('ref_axis',(-0.913545457642601,0.,0.4067366430758));
#33236=DIRECTION('',(-0.913545457642601,0.,0.4067366430758));
#33237=DIRECTION('center_axis',(0.147015766465199,0.707106781186544,0.691654801480229));
#33238=DIRECTION('ref_axis',(0.978147600733806,0.,-0.207911690817759));
#33239=DIRECTION('',(0.978147600733806,0.,-0.207911690817759));
#33240=DIRECTION('',(0.68477165125216,-0.577350269189626,0.444695909929535));
#33241=DIRECTION('center_axis',(0.691654801480227,0.707106781186546,-0.147015766465199));
#33242=DIRECTION('ref_axis',(-0.207911690817759,0.,-0.978147600733806));
#33243=DIRECTION('',(0.444695909929538,-0.57735026918963,-0.684771651252155));
#33244=DIRECTION('',(-0.207911690817759,0.,-0.978147600733806));
#33245=DIRECTION('center_axis',(-0.147015766465199,0.707106781186546,-0.691654801480227));
#33246=DIRECTION('ref_axis',(-0.978147600733806,0.,0.207911690817759));
#33247=DIRECTION('',(-0.978147600733806,0.,0.207911690817759));
#33248=DIRECTION('center_axis',(0.,0.707106781186547,0.707106781186548));
#33249=DIRECTION('ref_axis',(1.,0.,0.));
#33250=DIRECTION('',(1.,0.,0.));
#33251=DIRECTION('',(0.577350269189627,-0.577350269189627,0.577350269189624));
#33252=DIRECTION('center_axis',(0.707106781186548,0.707106781186548,0.));
#33253=DIRECTION('ref_axis',(0.,0.,-1.));
#33254=DIRECTION('',(0.577350269189626,-0.577350269189626,-0.577350269189625));
#33255=DIRECTION('',(0.,0.,-1.));
#33256=DIRECTION('center_axis',(0.,0.707106781186547,-0.707106781186548));
#33257=DIRECTION('ref_axis',(-1.,0.,0.));
#33258=DIRECTION('',(-1.,0.,0.));
#33259=DIRECTION('center_axis',(-0.353553390593273,0.707106781186549,-0.612372435695794));
#33260=DIRECTION('ref_axis',(-0.866025403784439,0.,0.5));
#33261=DIRECTION('',(-0.866025403784439,0.,0.5));
#33262=DIRECTION('',(0.211324865405184,-0.577350269189626,-0.788675134594813));
#33263=DIRECTION('center_axis',(0.5,0.,0.866025403784439));
#33264=DIRECTION('ref_axis',(-0.866025403784439,0.,0.5));
#33265=DIRECTION('',(-0.866025403784439,0.,0.5));
#33266=DIRECTION('',(0.,-1.,0.));
#33267=DIRECTION('center_axis',(0.612372435695796,0.707106781186546,-0.353553390593274));
#33268=DIRECTION('ref_axis',(-0.5,0.,-0.866025403784439));
#33269=DIRECTION('',(-0.5,0.,-0.866025403784439));
#33270=DIRECTION('center_axis',(0.525482745498762,0.707106781186544,-0.473146789255817));
#33271=DIRECTION('ref_axis',(-0.669130606358858,0.,-0.743144825477394));
#33272=DIRECTION('',(-0.669130606358858,0.,-0.743144825477394));
#33273=DIRECTION('',(0.0427321293319396,-0.57735026918963,-0.815377600740553));
#33274=DIRECTION('center_axis',(-0.473146789255815,0.707106781186547,-0.525482745498759));
#33275=DIRECTION('ref_axis',(-0.743144825477394,0.,0.669130606358858));
#33276=DIRECTION('',(-0.743144825477394,0.,0.669130606358858));
#33277=DIRECTION('',(-0.815377600740555,-0.577350269189626,-0.0427321293319522));
#33278=DIRECTION('center_axis',(-0.525482745498759,0.707106781186547,0.473146789255815));
#33279=DIRECTION('ref_axis',(0.669130606358858,0.,0.743144825477394));
#33280=DIRECTION('',(0.669130606358858,0.,0.743144825477394));
#33281=DIRECTION('center_axis',(-0.743144825477394,0.,0.669130606358858));
#33282=DIRECTION('ref_axis',(-0.669130606358858,0.,-0.743144825477394));
#33283=DIRECTION('',(0.,-1.,0.));
#33284=DIRECTION('',(-0.669130606358858,0.,-0.743144825477394));
#33285=DIRECTION('center_axis',(0.669130606358858,0.,0.743144825477394));
#33286=DIRECTION('ref_axis',(-0.743144825477394,0.,0.669130606358858));
#33287=DIRECTION('',(0.,-1.,0.));
#33288=DIRECTION('',(-0.743144825477394,0.,0.669130606358858));
#33289=DIRECTION('center_axis',(0.743144825477394,0.,-0.669130606358858));
#33290=DIRECTION('ref_axis',(0.669130606358858,0.,0.743144825477394));
#33291=DIRECTION('',(0.669130606358858,0.,0.743144825477394));
#33292=DIRECTION('center_axis',(0.415626937777453,0.707106781186548,-0.572061402817684));
#33293=DIRECTION('ref_axis',(-0.809016994374947,0.,-0.587785252292473));
#33294=DIRECTION('',(-0.809016994374947,0.,-0.587785252292473));
#33295=DIRECTION('',(-0.127728205844611,-0.577350269189624,-0.80644415311811));
#33296=DIRECTION('center_axis',(-0.572061402817685,0.707106781186546,-0.415626937777454));
#33297=DIRECTION('ref_axis',(-0.587785252292473,0.,0.809016994374947));
#33298=DIRECTION('',(-0.587785252292473,0.,0.809016994374947));
#33299=DIRECTION('',(-0.80644415311811,-0.577350269189624,0.127728205844611));
#33300=DIRECTION('center_axis',(-0.415626937777449,0.707106781186555,0.572061402817678));
#33301=DIRECTION('ref_axis',(0.809016994374947,0.,0.587785252292473));
#33302=DIRECTION('',(0.809016994374947,0.,0.587785252292473));
#33303=DIRECTION('center_axis',(-0.587785252292473,0.,0.809016994374947));
#33304=DIRECTION('ref_axis',(-0.809016994374947,0.,-0.587785252292473));
#33305=DIRECTION('',(0.,-1.,0.));
#33306=DIRECTION('',(-0.809016994374947,0.,-0.587785252292473));
#33307=DIRECTION('center_axis',(0.809016994374947,0.,0.587785252292473));
#33308=DIRECTION('ref_axis',(-0.587785252292473,0.,0.809016994374947));
#33309=DIRECTION('',(0.,-1.,0.));
#33310=DIRECTION('',(-0.587785252292473,0.,0.809016994374947));
#33311=DIRECTION('center_axis',(0.587785252292473,0.,-0.809016994374947));
#33312=DIRECTION('ref_axis',(0.809016994374947,0.,0.587785252292473));
#33313=DIRECTION('',(0.809016994374947,0.,0.587785252292473));
#33314=DIRECTION('center_axis',(0.287606238475951,0.707106781186546,-0.645974188021252));
#33315=DIRECTION('ref_axis',(-0.913545457642601,0.,-0.4067366430758));
#33316=DIRECTION('',(-0.913545457642601,0.,-0.4067366430758));
#33317=DIRECTION('',(-0.292606205517816,-0.57735026918963,-0.762265226256011));
#33318=DIRECTION('center_axis',(-0.645974188021253,0.707106781186545,-0.287606238475952));
#33319=DIRECTION('ref_axis',(-0.4067366430758,0.,0.913545457642601));
#33320=DIRECTION('',(-0.4067366430758,0.,0.913545457642601));
#33321=DIRECTION('',(-0.762265226256014,-0.577350269189629,0.292606205517809));
#33322=DIRECTION('center_axis',(-0.287606238475952,0.707106781186545,0.645974188021253));
#33323=DIRECTION('ref_axis',(0.913545457642601,0.,0.4067366430758));
#33324=DIRECTION('',(0.913545457642601,0.,0.4067366430758));
#33325=DIRECTION('center_axis',(-0.4067366430758,0.,0.913545457642601));
#33326=DIRECTION('ref_axis',(-0.913545457642601,0.,-0.4067366430758));
#33327=DIRECTION('',(0.,-1.,0.));
#33328=DIRECTION('',(-0.913545457642601,0.,-0.4067366430758));
#33329=DIRECTION('center_axis',(0.913545457642601,0.,0.4067366430758));
#33330=DIRECTION('ref_axis',(-0.4067366430758,0.,0.913545457642601));
#33331=DIRECTION('',(0.,-1.,0.));
#33332=DIRECTION('',(-0.4067366430758,0.,0.913545457642601));
#33333=DIRECTION('center_axis',(0.4067366430758,0.,-0.913545457642601));
#33334=DIRECTION('ref_axis',(0.913545457642601,0.,0.4067366430758));
#33335=DIRECTION('',(0.913545457642601,0.,0.4067366430758));
#33336=DIRECTION('center_axis',(0.147015766465199,0.707106781186547,-0.691654801480226));
#33337=DIRECTION('ref_axis',(-0.978147600733805,0.,-0.20791169081776));
#33338=DIRECTION('',(-0.978147600733805,0.,-0.20791169081776));
#33339=DIRECTION('',(-0.444695909929548,-0.577350269189626,-0.684771651252151));
#33340=DIRECTION('center_axis',(-0.691654801480235,0.707106781186538,-0.147015766465201));
#33341=DIRECTION('ref_axis',(-0.20791169081776,0.,0.978147600733805));
#33342=DIRECTION('',(-0.20791169081776,0.,0.978147600733805));
#33343=DIRECTION('',(-0.684771651252149,-0.577350269189628,0.444695909929549));
#33344=DIRECTION('center_axis',(-0.147015766465199,0.707106781186549,0.691654801480225));
#33345=DIRECTION('ref_axis',(0.978147600733805,0.,0.20791169081776));
#33346=DIRECTION('',(0.978147600733805,0.,0.20791169081776));
#33347=DIRECTION('center_axis',(-0.20791169081776,0.,0.978147600733806));
#33348=DIRECTION('ref_axis',(-0.978147600733805,0.,-0.20791169081776));
#33349=DIRECTION('',(0.,-1.,0.));
#33350=DIRECTION('',(-0.978147600733805,0.,-0.20791169081776));
#33351=DIRECTION('center_axis',(0.978147600733806,0.,0.20791169081776));
#33352=DIRECTION('ref_axis',(-0.20791169081776,0.,0.978147600733805));
#33353=DIRECTION('',(0.,-1.,0.));
#33354=DIRECTION('',(-0.20791169081776,0.,0.978147600733805));
#33355=DIRECTION('center_axis',(0.20791169081776,0.,-0.978147600733806));
#33356=DIRECTION('ref_axis',(0.978147600733805,0.,0.20791169081776));
#33357=DIRECTION('',(0.978147600733805,0.,0.20791169081776));
#33358=DIRECTION('center_axis',(8.65956056235494E-17,0.707106781186547,
-0.707106781186548));
#33359=DIRECTION('ref_axis',(-1.,0.,-1.22464679914735E-16));
#33360=DIRECTION('',(-1.,0.,-1.22464679914735E-16));
#33361=DIRECTION('',(-0.577350269189626,-0.577350269189626,-0.577350269189625));
#33362=DIRECTION('center_axis',(-0.707106781186548,0.707106781186548,-8.65956056235493E-17));
#33363=DIRECTION('ref_axis',(-1.22464679914735E-16,0.,1.));
#33364=DIRECTION('',(-1.22464679914735E-16,0.,1.));
#33365=DIRECTION('',(-0.577350269189626,-0.577350269189626,0.577350269189625));
#33366=DIRECTION('center_axis',(-8.65956056235494E-17,0.707106781186547,
0.707106781186548));
#33367=DIRECTION('ref_axis',(1.,0.,1.22464679914735E-16));
#33368=DIRECTION('',(1.,0.,1.22464679914735E-16));
#33369=DIRECTION('center_axis',(-1.22464679914735E-16,0.,1.));
#33370=DIRECTION('ref_axis',(-1.,0.,-1.22464679914735E-16));
#33371=DIRECTION('',(0.,-1.,0.));
#33372=DIRECTION('',(-1.,0.,-1.22464679914735E-16));
#33373=DIRECTION('center_axis',(1.,0.,1.22464679914735E-16));
#33374=DIRECTION('ref_axis',(-1.22464679914735E-16,0.,1.));
#33375=DIRECTION('',(0.,-1.,0.));
#33376=DIRECTION('',(-1.22464679914735E-16,0.,1.));
#33377=DIRECTION('center_axis',(1.22464679914735E-16,0.,-1.));
#33378=DIRECTION('ref_axis',(1.,0.,1.22464679914735E-16));
#33379=DIRECTION('',(1.,0.,1.22464679914735E-16));
#33380=DIRECTION('center_axis',(-0.147015766465198,0.707106781186547,-0.691654801480227));
#33381=DIRECTION('ref_axis',(-0.978147600733806,0.,0.207911690817759));
#33382=DIRECTION('',(-0.978147600733806,0.,0.207911690817759));
#33383=DIRECTION('',(-0.684771651252158,-0.577350269189624,-0.44469590992954));
#33384=DIRECTION('center_axis',(-0.691654801480227,0.707106781186546,0.147015766465199));
#33385=DIRECTION('ref_axis',(0.207911690817759,0.,0.978147600733806));
#33386=DIRECTION('',(0.207911690817759,0.,0.978147600733806));
#33387=DIRECTION('',(-0.444695909929548,-0.577350269189626,0.684771651252151));
#33388=DIRECTION('center_axis',(0.147015766465198,0.707106781186547,0.691654801480226));
#33389=DIRECTION('ref_axis',(0.978147600733806,0.,-0.207911690817759));
#33390=DIRECTION('',(0.978147600733806,0.,-0.207911690817759));
#33391=DIRECTION('center_axis',(0.207911690817759,0.,0.978147600733806));
#33392=DIRECTION('ref_axis',(-0.978147600733806,0.,0.207911690817759));
#33393=DIRECTION('',(0.,-1.,0.));
#33394=DIRECTION('',(-0.978147600733806,0.,0.207911690817759));
#33395=DIRECTION('center_axis',(0.978147600733806,0.,-0.207911690817759));
#33396=DIRECTION('ref_axis',(0.207911690817759,0.,0.978147600733806));
#33397=DIRECTION('',(0.,-1.,0.));
#33398=DIRECTION('',(0.207911690817759,0.,0.978147600733806));
#33399=DIRECTION('center_axis',(-0.207911690817759,0.,-0.978147600733806));
#33400=DIRECTION('ref_axis',(0.978147600733806,0.,-0.207911690817759));
#33401=DIRECTION('',(0.978147600733806,0.,-0.207911690817759));
#33402=DIRECTION('center_axis',(0.287606238475948,0.707106781186554,0.645974188021245));
#33403=DIRECTION('ref_axis',(0.913545457642601,0.,-0.4067366430758));
#33404=DIRECTION('',(0.913545457642601,0.,-0.4067366430758));
#33405=DIRECTION('',(-0.292606205517798,-0.577350269189628,0.762265226256019));
#33406=DIRECTION('center_axis',(-0.4067366430758,0.,-0.913545457642601));
#33407=DIRECTION('ref_axis',(0.913545457642601,0.,-0.4067366430758));
#33408=DIRECTION('',(0.913545457642601,0.,-0.4067366430758));
#33409=DIRECTION('',(0.,-1.,0.));
#33410=DIRECTION('center_axis',(-0.28760623847595,0.707106781186549,-0.64597418802125));
#33411=DIRECTION('ref_axis',(-0.913545457642601,0.,0.4067366430758));
#33412=DIRECTION('',(-0.913545457642601,0.,0.4067366430758));
#33413=DIRECTION('',(-0.762265226256003,-0.577350269189631,-0.292606205517836));
#33414=DIRECTION('center_axis',(-0.645974188021261,0.707106781186537,0.287606238475955));
#33415=DIRECTION('ref_axis',(0.4067366430758,0.,0.913545457642601));
#33416=DIRECTION('',(0.4067366430758,0.,0.913545457642601));
#33417=DIRECTION('center_axis',(0.4067366430758,0.,0.913545457642601));
#33418=DIRECTION('ref_axis',(-0.913545457642601,0.,0.4067366430758));
#33419=DIRECTION('',(0.,-1.,0.));
#33420=DIRECTION('',(-0.913545457642601,0.,0.4067366430758));
#33421=DIRECTION('center_axis',(0.913545457642601,0.,-0.4067366430758));
#33422=DIRECTION('ref_axis',(0.4067366430758,0.,0.913545457642601));
#33423=DIRECTION('',(0.4067366430758,0.,0.913545457642601));
#33424=DIRECTION('center_axis',(-0.415626937777449,0.707106781186555,-0.572061402817678));
#33425=DIRECTION('ref_axis',(-0.809016994374947,0.,0.587785252292473));
#33426=DIRECTION('',(-0.809016994374947,0.,0.587785252292473));
#33427=DIRECTION('',(-0.806444153118099,-0.577350269189634,-0.127728205844633));
#33428=DIRECTION('center_axis',(-0.572061402817694,0.707106781186535,0.415626937777461));
#33429=DIRECTION('ref_axis',(0.587785252292473,0.,0.809016994374947));
#33430=DIRECTION('',(0.587785252292473,0.,0.809016994374947));
#33431=DIRECTION('',(-0.127728205844587,-0.577350269189629,0.80644415311811));
#33432=DIRECTION('center_axis',(0.415626937777453,0.707106781186548,0.572061402817684));
#33433=DIRECTION('ref_axis',(0.809016994374947,0.,-0.587785252292473));
#33434=DIRECTION('',(0.809016994374947,0.,-0.587785252292473));
#33435=DIRECTION('center_axis',(0.587785252292473,0.,0.809016994374948));
#33436=DIRECTION('ref_axis',(-0.809016994374947,0.,0.587785252292473));
#33437=DIRECTION('',(0.,-1.,0.));
#33438=DIRECTION('',(-0.809016994374947,0.,0.587785252292473));
#33439=DIRECTION('center_axis',(0.809016994374948,0.,-0.587785252292473));
#33440=DIRECTION('ref_axis',(0.587785252292473,0.,0.809016994374947));
#33441=DIRECTION('',(0.,-1.,0.));
#33442=DIRECTION('',(0.587785252292473,0.,0.809016994374947));
#33443=DIRECTION('center_axis',(-0.587785252292473,0.,-0.809016994374948));
#33444=DIRECTION('ref_axis',(0.809016994374947,0.,-0.587785252292473));
#33445=DIRECTION('',(0.809016994374947,0.,-0.587785252292473));
#33446=DIRECTION('center_axis',(-0.525482745498762,0.707106781186543,-0.473146789255818));
#33447=DIRECTION('ref_axis',(-0.669130606358858,0.,0.743144825477394));
#33448=DIRECTION('',(-0.669130606358858,0.,0.743144825477394));
#33449=DIRECTION('',(-0.815377600740551,-0.577350269189633,0.0427321293319399));
#33450=DIRECTION('center_axis',(-0.473146789255817,0.707106781186545,0.525482745498761));
#33451=DIRECTION('ref_axis',(0.743144825477394,0.,0.669130606358858));
#33452=DIRECTION('',(0.743144825477394,0.,0.669130606358858));
#33453=DIRECTION('',(0.0427321293319399,-0.577350269189633,0.815377600740551));
#33454=DIRECTION('center_axis',(0.525482745498759,0.707106781186547,0.473146789255815));
#33455=DIRECTION('ref_axis',(0.669130606358858,0.,-0.743144825477394));
#33456=DIRECTION('',(0.669130606358858,0.,-0.743144825477394));
#33457=DIRECTION('center_axis',(0.743144825477394,0.,0.669130606358858));
#33458=DIRECTION('ref_axis',(-0.669130606358858,0.,0.743144825477394));
#33459=DIRECTION('',(0.,-1.,0.));
#33460=DIRECTION('',(-0.669130606358858,0.,0.743144825477394));
#33461=DIRECTION('center_axis',(0.669130606358858,0.,-0.743144825477394));
#33462=DIRECTION('ref_axis',(0.743144825477394,0.,0.669130606358858));
#33463=DIRECTION('',(0.,-1.,0.));
#33464=DIRECTION('',(0.743144825477394,0.,0.669130606358858));
#33465=DIRECTION('center_axis',(-0.743144825477394,0.,-0.669130606358858));
#33466=DIRECTION('ref_axis',(0.669130606358858,0.,-0.743144825477394));
#33467=DIRECTION('',(0.669130606358858,0.,-0.743144825477394));
#33468=DIRECTION('center_axis',(-0.612372435695796,0.707106781186545,-0.353553390593275));
#33469=DIRECTION('ref_axis',(-0.5,0.,0.866025403784438));
#33470=DIRECTION('',(-0.5,0.,0.866025403784438));
#33471=DIRECTION('',(-0.788675134594813,-0.577350269189619,0.211324865405206));
#33472=DIRECTION('center_axis',(-0.353553390593269,0.707106781186557,0.612372435695786));
#33473=DIRECTION('ref_axis',(0.866025403784438,0.,0.5));
#33474=DIRECTION('',(0.866025403784438,0.,0.5));
#33475=DIRECTION('',(0.211324865405179,-0.577350269189617,0.788675134594822));
#33476=DIRECTION('center_axis',(0.612372435695793,0.707106781186549,0.353553390593274));
#33477=DIRECTION('ref_axis',(0.5,0.,-0.866025403784438));
#33478=DIRECTION('',(0.5,0.,-0.866025403784438));
#33479=DIRECTION('center_axis',(0.866025403784438,0.,0.5));
#33480=DIRECTION('ref_axis',(-0.5,0.,0.866025403784438));
#33481=DIRECTION('',(0.,-1.,0.));
#33482=DIRECTION('',(-0.5,0.,0.866025403784438));
#33483=DIRECTION('center_axis',(0.5,0.,-0.866025403784438));
#33484=DIRECTION('ref_axis',(0.866025403784438,0.,0.5));
#33485=DIRECTION('',(0.,-1.,0.));
#33486=DIRECTION('',(0.866025403784438,0.,0.5));
#33487=DIRECTION('center_axis',(-0.866025403784438,0.,-0.5));
#33488=DIRECTION('ref_axis',(0.5,0.,-0.866025403784438));
#33489=DIRECTION('',(0.5,0.,-0.866025403784438));
#33490=DIRECTION('center_axis',(-0.672498511963957,0.707106781186548,-0.218508012224411));
#33491=DIRECTION('ref_axis',(-0.309016994374948,0.,0.951056516295153));
#33492=DIRECTION('',(-0.309016994374948,0.,0.951056516295153));
#33493=DIRECTION('',(-0.7275037805841,-0.577350269189624,0.370681690811012));
#33494=DIRECTION('center_axis',(-0.218508012224412,0.707106781186544,0.67249851196396));
#33495=DIRECTION('ref_axis',(0.951056516295153,0.,0.309016994374948));
#33496=DIRECTION('',(0.951056516295153,0.,0.309016994374948));
#33497=DIRECTION('',(0.370681690811018,-0.577350269189624,0.727503780584097));
#33498=DIRECTION('center_axis',(0.672498511963954,0.707106781186551,0.21850801222441));
#33499=DIRECTION('ref_axis',(0.309016994374948,0.,-0.951056516295153));
#33500=DIRECTION('',(0.309016994374948,0.,-0.951056516295153));
#33501=DIRECTION('center_axis',(0.951056516295154,0.,0.309016994374948));
#33502=DIRECTION('ref_axis',(-0.309016994374948,0.,0.951056516295153));
#33503=DIRECTION('',(0.,-1.,0.));
#33504=DIRECTION('',(-0.309016994374948,0.,0.951056516295153));
#33505=DIRECTION('center_axis',(0.309016994374948,0.,-0.951056516295154));
#33506=DIRECTION('ref_axis',(0.951056516295153,0.,0.309016994374948));
#33507=DIRECTION('',(0.,-1.,0.));
#33508=DIRECTION('',(0.951056516295153,0.,0.309016994374948));
#33509=DIRECTION('center_axis',(-0.951056516295154,0.,-0.309016994374948));
#33510=DIRECTION('ref_axis',(0.309016994374948,0.,-0.951056516295153));
#33511=DIRECTION('',(0.309016994374948,0.,-0.951056516295153));
#33512=DIRECTION('center_axis',(-0.703233176253405,0.707106781186547,-0.0739127852035674));
#33513=DIRECTION('ref_axis',(-0.104528463267654,0.,0.994521895368273));
#33514=DIRECTION('',(-0.104528463267654,0.,0.994521895368273));
#33515=DIRECTION('',(-0.634537020411399,-0.577350269189621,0.513837947600307));
#33516=DIRECTION('center_axis',(-0.0739127852035669,0.707106781186551,0.703233176253401));
#33517=DIRECTION('ref_axis',(0.994521895368273,0.,0.104528463267654));
#33518=DIRECTION('',(0.994521895368273,0.,0.104528463267654));
#33519=DIRECTION('',(0.513837947600289,-0.577350269189625,0.63453702041141));
#33520=DIRECTION('center_axis',(0.703233176253406,0.707106781186546,0.0739127852035675));
#33521=DIRECTION('ref_axis',(0.104528463267654,0.,-0.994521895368273));
#33522=DIRECTION('',(0.104528463267654,0.,-0.994521895368273));
#33523=DIRECTION('center_axis',(0.994521895368273,0.,0.104528463267654));
#33524=DIRECTION('ref_axis',(-0.104528463267654,0.,0.994521895368273));
#33525=DIRECTION('',(0.,-1.,0.));
#33526=DIRECTION('',(-0.104528463267654,0.,0.994521895368273));
#33527=DIRECTION('center_axis',(0.104528463267654,0.,-0.994521895368273));
#33528=DIRECTION('ref_axis',(0.994521895368273,0.,0.104528463267654));
#33529=DIRECTION('',(0.,-1.,0.));
#33530=DIRECTION('',(0.994521895368273,0.,0.104528463267654));
#33531=DIRECTION('center_axis',(-0.994521895368273,0.,-0.104528463267654));
#33532=DIRECTION('ref_axis',(0.104528463267654,0.,-0.994521895368273));
#33533=DIRECTION('',(0.104528463267654,0.,-0.994521895368273));
#33534=DIRECTION('center_axis',(-0.703233176253405,0.707106781186547,0.0739127852035665));
#33535=DIRECTION('ref_axis',(0.104528463267653,0.,0.994521895368274));
#33536=DIRECTION('',(0.104528463267653,0.,0.994521895368273));
#33537=DIRECTION('',(-0.513837947600287,-0.57735026918962,0.634537020411416));
#33538=DIRECTION('center_axis',(0.0739127852035652,0.707106781186559,0.703233176253393));
#33539=DIRECTION('ref_axis',(0.994521895368273,0.,-0.104528463267653));
#33540=DIRECTION('',(0.994521895368273,0.,-0.104528463267653));
#33541=DIRECTION('',(0.634537020411404,-0.577350269189624,0.513837947600297));
#33542=DIRECTION('center_axis',(0.703233176253404,0.707106781186547,-0.0739127852035664));
#33543=DIRECTION('ref_axis',(-0.104528463267653,0.,-0.994521895368274));
#33544=DIRECTION('',(-0.104528463267653,0.,-0.994521895368273));
#33545=DIRECTION('center_axis',(0.994521895368273,0.,-0.104528463267653));
#33546=DIRECTION('ref_axis',(0.104528463267653,0.,0.994521895368273));
#33547=DIRECTION('',(0.,-1.,0.));
#33548=DIRECTION('',(0.104528463267653,0.,0.994521895368273));
#33549=DIRECTION('center_axis',(-0.104528463267653,0.,-0.994521895368273));
#33550=DIRECTION('ref_axis',(0.994521895368273,0.,-0.104528463267653));
#33551=DIRECTION('',(0.,-1.,0.));
#33552=DIRECTION('',(0.994521895368273,0.,-0.104528463267653));
#33553=DIRECTION('center_axis',(-0.994521895368273,0.,0.104528463267653));
#33554=DIRECTION('ref_axis',(-0.104528463267653,0.,-0.994521895368273));
#33555=DIRECTION('',(-0.104528463267653,0.,-0.994521895368273));
#33556=DIRECTION('center_axis',(-0.672498511963955,0.70710678118655,0.21850801222441));
#33557=DIRECTION('ref_axis',(0.309016994374947,0.,0.951056516295154));
#33558=DIRECTION('',(0.309016994374947,0.,0.951056516295154));
#33559=DIRECTION('',(-0.370681690810995,-0.577350269189617,0.727503780584114));
#33560=DIRECTION('center_axis',(0.218508012224409,0.707106781186553,0.672498511963952));
#33561=DIRECTION('ref_axis',(0.951056516295154,0.,-0.309016994374947));
#33562=DIRECTION('',(0.951056516295154,0.,-0.309016994374947));
#33563=DIRECTION('',(0.727503780584098,-0.57735026918962,0.370681690811022));
#33564=DIRECTION('center_axis',(0.672498511963957,0.707106781186548,-0.21850801222441));
#33565=DIRECTION('ref_axis',(-0.309016994374947,0.,-0.951056516295154));
#33566=DIRECTION('',(-0.309016994374947,0.,-0.951056516295154));
#33567=DIRECTION('center_axis',(0.951056516295154,0.,-0.309016994374947));
#33568=DIRECTION('ref_axis',(0.309016994374947,0.,0.951056516295154));
#33569=DIRECTION('',(0.,-1.,0.));
#33570=DIRECTION('',(0.309016994374947,0.,0.951056516295154));
#33571=DIRECTION('center_axis',(-0.309016994374947,0.,-0.951056516295154));
#33572=DIRECTION('ref_axis',(0.951056516295154,0.,-0.309016994374947));
#33573=DIRECTION('',(0.,-1.,0.));
#33574=DIRECTION('',(0.951056516295154,0.,-0.309016994374947));
#33575=DIRECTION('center_axis',(-0.951056516295154,0.,0.309016994374947));
#33576=DIRECTION('ref_axis',(-0.309016994374947,0.,-0.951056516295154));
#33577=DIRECTION('',(-0.309016994374947,0.,-0.951056516295154));
#33578=DIRECTION('center_axis',(-0.612372435695797,0.707106781186545,0.353553390593274));
#33579=DIRECTION('ref_axis',(0.499999999999999,0.,0.866025403784439));
#33580=DIRECTION('',(0.499999999999999,0.,0.866025403784439));
#33581=DIRECTION('',(-0.211324865405175,-0.577350269189623,0.788675134594818));
#33582=DIRECTION('center_axis',(0.353553390593268,0.707106781186557,0.612372435695786));
#33583=DIRECTION('ref_axis',(0.866025403784439,0.,-0.499999999999999));
#33584=DIRECTION('',(0.866025403784439,0.,-0.499999999999999));
#33585=DIRECTION('',(0.788675134594813,-0.577350269189619,0.211324865405206));
#33586=DIRECTION('center_axis',(0.612372435695795,0.707106781186547,-0.353553390593274));
#33587=DIRECTION('ref_axis',(-0.499999999999999,0.,-0.866025403784439));
#33588=DIRECTION('',(-0.499999999999999,0.,-0.866025403784439));
#33589=DIRECTION('center_axis',(0.866025403784439,0.,-0.499999999999999));
#33590=DIRECTION('ref_axis',(0.499999999999999,0.,0.866025403784439));
#33591=DIRECTION('',(0.,-1.,0.));
#33592=DIRECTION('',(0.499999999999999,0.,0.866025403784439));
#33593=DIRECTION('center_axis',(-0.499999999999999,0.,-0.866025403784439));
#33594=DIRECTION('ref_axis',(0.866025403784439,0.,-0.499999999999999));
#33595=DIRECTION('',(0.,-1.,0.));
#33596=DIRECTION('',(0.866025403784439,0.,-0.499999999999999));
#33597=DIRECTION('center_axis',(-0.866025403784439,0.,0.499999999999999));
#33598=DIRECTION('ref_axis',(-0.499999999999999,0.,-0.866025403784439));
#33599=DIRECTION('',(-0.499999999999999,0.,-0.866025403784439));
#33600=DIRECTION('center_axis',(-0.525482745498764,0.707106781186541,0.473146789255819));
#33601=DIRECTION('ref_axis',(0.669130606358858,0.,0.743144825477395));
#33602=DIRECTION('',(0.669130606358858,0.,0.743144825477395));
#33603=DIRECTION('',(-0.0427321293319654,-0.577350269189632,0.81537760074055));
#33604=DIRECTION('center_axis',(0.473146789255822,0.707106781186536,0.525482745498768));
#33605=DIRECTION('ref_axis',(0.743144825477395,0.,-0.669130606358858));
#33606=DIRECTION('',(0.743144825477395,0.,-0.669130606358858));
#33607=DIRECTION('',(0.815377600740551,-0.577350269189633,0.0427321293319271));
#33608=DIRECTION('center_axis',(0.52548274549876,0.707106781186547,-0.473146789255815));
#33609=DIRECTION('ref_axis',(-0.669130606358858,0.,-0.743144825477395));
#33610=DIRECTION('',(-0.669130606358858,0.,-0.743144825477395));
#33611=DIRECTION('center_axis',(0.743144825477395,0.,-0.669130606358858));
#33612=DIRECTION('ref_axis',(0.669130606358858,0.,0.743144825477395));
#33613=DIRECTION('',(0.,-1.,0.));
#33614=DIRECTION('',(0.669130606358858,0.,0.743144825477395));
#33615=DIRECTION('center_axis',(-0.669130606358858,0.,-0.743144825477395));
#33616=DIRECTION('ref_axis',(0.743144825477395,0.,-0.669130606358858));
#33617=DIRECTION('',(0.,-1.,0.));
#33618=DIRECTION('',(0.743144825477395,0.,-0.669130606358858));
#33619=DIRECTION('center_axis',(-0.743144825477395,0.,0.669130606358858));
#33620=DIRECTION('ref_axis',(-0.669130606358858,0.,-0.743144825477395));
#33621=DIRECTION('',(-0.669130606358858,0.,-0.743144825477395));
#33622=DIRECTION('center_axis',(-0.415626937777453,0.707106781186548,0.572061402817684));
#33623=DIRECTION('ref_axis',(0.809016994374947,0.,0.587785252292473));
#33624=DIRECTION('',(0.809016994374947,0.,0.587785252292473));
#33625=DIRECTION('',(0.127728205844587,-0.577350269189632,0.806444153118108));
#33626=DIRECTION('center_axis',(0.572061402817692,0.707106781186538,0.415626937777459));
#33627=DIRECTION('ref_axis',(0.587785252292473,0.,-0.809016994374947));
#33628=DIRECTION('',(0.587785252292473,0.,-0.809016994374947));
#33629=DIRECTION('',(0.806444153118105,-0.577350269189629,-0.127728205844619));
#33630=DIRECTION('center_axis',(0.415626937777454,0.707106781186546,-0.572061402817685));
#33631=DIRECTION('ref_axis',(-0.809016994374947,0.,-0.587785252292473));
#33632=DIRECTION('',(-0.809016994374947,0.,-0.587785252292473));
#33633=DIRECTION('center_axis',(0.587785252292473,0.,-0.809016994374947));
#33634=DIRECTION('ref_axis',(0.809016994374947,0.,0.587785252292473));
#33635=DIRECTION('',(0.,-1.,0.));
#33636=DIRECTION('',(0.809016994374947,0.,0.587785252292473));
#33637=DIRECTION('center_axis',(-0.809016994374947,0.,-0.587785252292473));
#33638=DIRECTION('ref_axis',(0.587785252292473,0.,-0.809016994374947));
#33639=DIRECTION('',(0.,-1.,0.));
#33640=DIRECTION('',(0.587785252292473,0.,-0.809016994374947));
#33641=DIRECTION('center_axis',(-0.587785252292473,0.,0.809016994374947));
#33642=DIRECTION('ref_axis',(-0.809016994374947,0.,-0.587785252292473));
#33643=DIRECTION('',(-0.809016994374947,0.,-0.587785252292473));
#33644=DIRECTION('center_axis',(-0.287606238475952,0.707106781186546,0.645974188021252));
#33645=DIRECTION('ref_axis',(0.913545457642601,0.,0.406736643075801));
#33646=DIRECTION('',(0.913545457642601,0.,0.406736643075801));
#33647=DIRECTION('',(0.292606205517837,-0.577350269189621,0.76226522625601));
#33648=DIRECTION('center_axis',(0.645974188021245,0.707106781186554,0.287606238475949));
#33649=DIRECTION('ref_axis',(0.406736643075801,0.,-0.913545457642601));
#33650=DIRECTION('',(0.406736643075801,0.,-0.913545457642601));
#33651=DIRECTION('',(0.762265226256017,-0.577350269189622,-0.292606205517818));
#33652=DIRECTION('center_axis',(0.287606238475951,0.707106781186549,-0.64597418802125));
#33653=DIRECTION('ref_axis',(-0.913545457642601,0.,-0.406736643075801));
#33654=DIRECTION('',(-0.913545457642601,0.,-0.406736643075801));
#33655=DIRECTION('center_axis',(0.406736643075801,0.,-0.913545457642601));
#33656=DIRECTION('ref_axis',(0.913545457642601,0.,0.406736643075801));
#33657=DIRECTION('',(0.,-1.,0.));
#33658=DIRECTION('',(0.913545457642601,0.,0.406736643075801));
#33659=DIRECTION('center_axis',(-0.913545457642601,0.,-0.406736643075801));
#33660=DIRECTION('ref_axis',(0.406736643075801,0.,-0.913545457642601));
#33661=DIRECTION('',(0.,-1.,0.));
#33662=DIRECTION('',(0.406736643075801,0.,-0.913545457642601));
#33663=DIRECTION('center_axis',(-0.406736643075801,0.,0.913545457642601));
#33664=DIRECTION('ref_axis',(-0.913545457642601,0.,-0.406736643075801));
#33665=DIRECTION('',(-0.913545457642601,0.,-0.406736643075801));
#33666=DIRECTION('center_axis',(-0.147015766465199,0.707106781186546,0.691654801480227));
#33667=DIRECTION('ref_axis',(0.978147600733805,0.,0.20791169081776));
#33668=DIRECTION('',(0.978147600733805,0.,0.20791169081776));
#33669=DIRECTION('',(0.444695909929548,-0.577350269189626,0.684771651252151));
#33670=DIRECTION('center_axis',(0.691654801480234,0.707106781186539,0.147015766465201));
#33671=DIRECTION('ref_axis',(0.20791169081776,0.,-0.978147600733805));
#33672=DIRECTION('',(0.20791169081776,0.,-0.978147600733805));
#33673=DIRECTION('',(0.68477165125215,-0.577350269189629,-0.444695909929547));
#33674=DIRECTION('center_axis',(0.147015766465199,0.707106781186547,-0.691654801480226));
#33675=DIRECTION('ref_axis',(-0.978147600733805,0.,-0.20791169081776));
#33676=DIRECTION('',(-0.978147600733805,0.,-0.20791169081776));
#33677=DIRECTION('center_axis',(0.20791169081776,0.,-0.978147600733806));
#33678=DIRECTION('ref_axis',(0.978147600733805,0.,0.20791169081776));
#33679=DIRECTION('',(0.,-1.,0.));
#33680=DIRECTION('',(0.978147600733805,0.,0.20791169081776));
#33681=DIRECTION('center_axis',(-0.978147600733806,0.,-0.20791169081776));
#33682=DIRECTION('ref_axis',(0.20791169081776,0.,-0.978147600733805));
#33683=DIRECTION('',(0.,-1.,0.));
#33684=DIRECTION('',(0.20791169081776,0.,-0.978147600733805));
#33685=DIRECTION('center_axis',(-0.20791169081776,0.,0.978147600733806));
#33686=DIRECTION('ref_axis',(-0.978147600733805,0.,-0.20791169081776));
#33687=DIRECTION('',(-0.978147600733805,0.,-0.20791169081776));
#33688=DIRECTION('center_axis',(0.707106781186548,-0.707106781186548,0.));
#33689=DIRECTION('ref_axis',(0.,0.,-1.));
#33690=DIRECTION('',(0.,0.,-1.));
#33691=DIRECTION('',(-0.577350269189625,-0.577350269189625,-0.577350269189627));
#33692=DIRECTION('',(0.,0.,1.));
#33693=DIRECTION('',(-0.577350269189625,-0.577350269189625,0.577350269189627));
#33694=DIRECTION('center_axis',(0.,-0.707106781186549,-0.707106781186546));
#33695=DIRECTION('ref_axis',(-1.,0.,0.));
#33696=DIRECTION('',(1.,0.,0.));
#33697=DIRECTION('',(-1.,0.,0.));
#33698=DIRECTION('center_axis',(0.,-1.,0.));
#33699=DIRECTION('ref_axis',(0.,0.,-1.));
#33700=DIRECTION('',(1.,0.,0.));
#33701=DIRECTION('',(0.978147600733805,0.,0.20791169081776));
#33702=DIRECTION('',(0.20791169081776,0.,-0.978147600733805));
#33703=DIRECTION('',(-0.978147600733805,0.,-0.20791169081776));
#33704=DIRECTION('',(0.913545457642601,0.,0.406736643075801));
#33705=DIRECTION('',(0.406736643075801,0.,-0.913545457642601));
#33706=DIRECTION('',(-0.913545457642601,0.,-0.406736643075801));
#33707=DIRECTION('',(0.809016994374947,0.,0.587785252292473));
#33708=DIRECTION('',(0.587785252292473,0.,-0.809016994374947));
#33709=DIRECTION('',(-0.809016994374947,0.,-0.587785252292473));
#33710=DIRECTION('',(0.669130606358858,0.,0.743144825477395));
#33711=DIRECTION('',(0.743144825477395,0.,-0.669130606358858));
#33712=DIRECTION('',(-0.669130606358858,0.,-0.743144825477395));
#33713=DIRECTION('',(0.499999999999999,0.,0.866025403784439));
#33714=DIRECTION('',(0.866025403784439,0.,-0.499999999999999));
#33715=DIRECTION('',(-0.499999999999999,0.,-0.866025403784439));
#33716=DIRECTION('',(0.309016994374947,0.,0.951056516295154));
#33717=DIRECTION('',(0.951056516295154,0.,-0.309016994374947));
#33718=DIRECTION('',(-0.309016994374947,0.,-0.951056516295154));
#33719=DIRECTION('',(0.104528463267653,0.,0.994521895368273));
#33720=DIRECTION('',(0.994521895368273,0.,-0.104528463267653));
#33721=DIRECTION('',(-0.104528463267653,0.,-0.994521895368273));
#33722=DIRECTION('',(-0.104528463267654,0.,0.994521895368273));
#33723=DIRECTION('',(0.994521895368273,0.,0.104528463267654));
#33724=DIRECTION('',(0.104528463267654,0.,-0.994521895368273));
#33725=DIRECTION('',(-0.309016994374948,0.,0.951056516295153));
#33726=DIRECTION('',(0.951056516295153,0.,0.309016994374948));
#33727=DIRECTION('',(0.309016994374948,0.,-0.951056516295153));
#33728=DIRECTION('',(-0.5,0.,0.866025403784438));
#33729=DIRECTION('',(0.866025403784438,0.,0.5));
#33730=DIRECTION('',(0.5,0.,-0.866025403784438));
#33731=DIRECTION('',(-0.669130606358858,0.,0.743144825477394));
#33732=DIRECTION('',(0.743144825477394,0.,0.669130606358858));
#33733=DIRECTION('',(0.669130606358858,0.,-0.743144825477394));
#33734=DIRECTION('',(-0.809016994374947,0.,0.587785252292473));
#33735=DIRECTION('',(0.587785252292473,0.,0.809016994374947));
#33736=DIRECTION('',(0.809016994374947,0.,-0.587785252292473));
#33737=DIRECTION('',(-0.913545457642601,0.,0.4067366430758));
#33738=DIRECTION('',(0.4067366430758,0.,0.913545457642601));
#33739=DIRECTION('',(0.913545457642601,0.,-0.4067366430758));
#33740=DIRECTION('',(-0.978147600733806,0.,0.207911690817759));
#33741=DIRECTION('',(0.207911690817759,0.,0.978147600733806));
#33742=DIRECTION('',(0.978147600733806,0.,-0.207911690817759));
#33743=DIRECTION('',(-1.,0.,-1.22464679914735E-16));
#33744=DIRECTION('',(-1.22464679914735E-16,0.,1.));
#33745=DIRECTION('',(1.,0.,1.22464679914735E-16));
#33746=DIRECTION('',(-0.978147600733805,0.,-0.20791169081776));
#33747=DIRECTION('',(-0.20791169081776,0.,0.978147600733805));
#33748=DIRECTION('',(0.978147600733805,0.,0.20791169081776));
#33749=DIRECTION('',(-0.913545457642601,0.,-0.4067366430758));
#33750=DIRECTION('',(-0.4067366430758,0.,0.913545457642601));
#33751=DIRECTION('',(0.913545457642601,0.,0.4067366430758));
#33752=DIRECTION('',(-0.809016994374947,0.,-0.587785252292473));
#33753=DIRECTION('',(-0.587785252292473,0.,0.809016994374947));
#33754=DIRECTION('',(0.809016994374947,0.,0.587785252292473));
#33755=DIRECTION('',(-0.669130606358858,0.,-0.743144825477394));
#33756=DIRECTION('',(-0.743144825477394,0.,0.669130606358858));
#33757=DIRECTION('',(0.669130606358858,0.,0.743144825477394));
#33758=DIRECTION('',(-0.5,0.,-0.866025403784439));
#33759=DIRECTION('',(-0.866025403784439,0.,0.5));
#33760=DIRECTION('',(0.5,0.,0.866025403784439));
#33761=DIRECTION('',(-0.309016994374947,0.,-0.951056516295154));
#33762=DIRECTION('',(-0.951056516295154,0.,0.309016994374947));
#33763=DIRECTION('',(0.309016994374947,0.,0.951056516295154));
#33764=DIRECTION('',(-0.104528463267653,0.,-0.994521895368273));
#33765=DIRECTION('',(-0.994521895368273,0.,0.104528463267653));
#33766=DIRECTION('',(0.104528463267653,0.,0.994521895368273));
#33767=DIRECTION('',(0.104528463267654,0.,-0.994521895368273));
#33768=DIRECTION('',(-0.994521895368273,0.,-0.104528463267654));
#33769=DIRECTION('',(-0.104528463267654,0.,0.994521895368273));
#33770=DIRECTION('',(0.309016994374948,0.,-0.951056516295154));
#33771=DIRECTION('',(-0.951056516295154,0.,-0.309016994374948));
#33772=DIRECTION('',(-0.309016994374948,0.,0.951056516295154));
#33773=DIRECTION('',(0.5,0.,-0.866025403784439));
#33774=DIRECTION('',(-0.866025403784439,0.,-0.5));
#33775=DIRECTION('',(-0.5,0.,0.866025403784439));
#33776=DIRECTION('',(0.669130606358858,0.,-0.743144825477394));
#33777=DIRECTION('',(-0.743144825477394,0.,-0.669130606358858));
#33778=DIRECTION('',(-0.669130606358858,0.,0.743144825477394));
#33779=DIRECTION('',(0.809016994374947,0.,-0.587785252292473));
#33780=DIRECTION('',(-0.587785252292473,0.,-0.809016994374947));
#33781=DIRECTION('',(-0.809016994374947,0.,0.587785252292473));
#33782=DIRECTION('',(0.913545457642601,0.,-0.4067366430758));
#33783=DIRECTION('',(-0.4067366430758,0.,-0.913545457642601));
#33784=DIRECTION('',(-0.913545457642601,0.,0.4067366430758));
#33785=DIRECTION('',(0.978147600733806,0.,-0.207911690817759));
#33786=DIRECTION('',(-0.207911690817759,0.,-0.978147600733806));
#33787=DIRECTION('',(-0.978147600733806,0.,0.207911690817759));
#33788=DIRECTION('',(1.,0.,0.));
#33789=DIRECTION('',(0.,0.,-1.));
#33790=DIRECTION('',(-1.,0.,0.));
#33791=DIRECTION('center_axis',(0.,1.,0.));
#33792=DIRECTION('ref_axis',(1.,0.,0.));
#33793=DIRECTION('',(-1.,0.,0.));
#33794=DIRECTION('',(0.,0.,1.));
#33795=DIRECTION('',(1.,0.,0.));
#33796=DIRECTION('center_axis',(0.,1.,0.));
#33797=DIRECTION('ref_axis',(1.,0.,0.));
#33798=DIRECTION('center_axis',(0.,-0.707106781186549,0.707106781186546));
#33799=DIRECTION('ref_axis',(1.,0.,0.));
#33800=DIRECTION('',(-1.,0.,0.));
#33801=DIRECTION('center_axis',(0.691654801480234,-0.707106781186539,-0.1470157664652));
#33802=DIRECTION('ref_axis',(-0.207911690817759,0.,-0.978147600733805));
#33803=DIRECTION('',(0.68477165125215,0.577350269189629,0.444695909929547));
#33804=DIRECTION('',(0.207911690817759,0.,0.978147600733806));
#33805=DIRECTION('',(-0.444695909929537,-0.577350269189628,0.684771651252156));
#33806=DIRECTION('center_axis',(0.147015766465198,-0.707106781186549,0.691654801480225));
#33807=DIRECTION('ref_axis',(0.978147600733806,0.,-0.207911690817759));
#33808=DIRECTION('',(-0.978147600733806,0.,0.207911690817759));
#33809=DIRECTION('center_axis',(-0.147015766465198,-0.70710678118655,-0.691654801480224));
#33810=DIRECTION('ref_axis',(-0.978147600733806,0.,0.207911690817759));
#33811=DIRECTION('',(0.978147600733806,0.,-0.207911690817759));
#33812=DIRECTION('center_axis',(0.64597418802127,-0.707106781186527,-0.287606238475959));
#33813=DIRECTION('ref_axis',(-0.4067366430758,0.,-0.913545457642601));
#33814=DIRECTION('',(0.76226522625599,0.577350269189631,0.292606205517868));
#33815=DIRECTION('',(0.4067366430758,0.,0.913545457642601));
#33816=DIRECTION('',(-0.292606205517786,-0.577350269189647,0.762265226256009));
#33817=DIRECTION('center_axis',(0.287606238475944,-0.707106781186565,0.645974188021235));
#33818=DIRECTION('ref_axis',(0.913545457642601,0.,-0.4067366430758));
#33819=DIRECTION('',(-0.913545457642601,0.,0.4067366430758));
#33820=DIRECTION('center_axis',(-0.287606238475955,-0.707106781186538,-0.64597418802126));
#33821=DIRECTION('ref_axis',(-0.913545457642601,0.,0.4067366430758));
#33822=DIRECTION('',(0.913545457642601,0.,-0.4067366430758));
#33823=DIRECTION('center_axis',(0.4067366430758,0.,0.913545457642601));
#33824=DIRECTION('ref_axis',(0.913545457642601,0.,-0.4067366430758));
#33825=DIRECTION('',(0.,1.,0.));
#33826=DIRECTION('',(0.913545457642601,0.,-0.4067366430758));
#33827=DIRECTION('center_axis',(-0.913545457642601,0.,0.4067366430758));
#33828=DIRECTION('ref_axis',(0.4067366430758,0.,0.913545457642601));
#33829=DIRECTION('',(0.,1.,0.));
#33830=DIRECTION('',(0.4067366430758,0.,0.913545457642601));
#33831=DIRECTION('center_axis',(0.572061402817685,-0.707106781186546,-0.415626937777454));
#33832=DIRECTION('ref_axis',(-0.587785252292473,0.,-0.809016994374947));
#33833=DIRECTION('',(0.806444153118111,0.577350269189624,0.127728205844605));
#33834=DIRECTION('',(0.587785252292473,0.,0.809016994374947));
#33835=DIRECTION('',(-0.127728205844611,-0.577350269189624,0.80644415311811));
#33836=DIRECTION('center_axis',(0.415626937777451,-0.707106781186551,0.572061402817681));
#33837=DIRECTION('ref_axis',(0.809016994374947,0.,-0.587785252292473));
#33838=DIRECTION('',(-0.809016994374947,0.,0.587785252292473));
#33839=DIRECTION('center_axis',(-0.415626937777456,-0.707106781186543,-0.572061402817688));
#33840=DIRECTION('ref_axis',(-0.809016994374947,0.,0.587785252292473));
#33841=DIRECTION('',(0.809016994374947,0.,-0.587785252292473));
#33842=DIRECTION('center_axis',(0.473146789255825,-0.707106781186533,-0.525482745498769));
#33843=DIRECTION('ref_axis',(-0.743144825477394,0.,-0.669130606358858));
#33844=DIRECTION('',(0.815377600740556,0.577350269189627,-0.0427321293319138));
#33845=DIRECTION('',(0.743144825477394,0.,0.669130606358858));
#33846=DIRECTION('',(0.0427321293319529,-0.577350269189635,0.815377600740548));
#33847=DIRECTION('center_axis',(0.525482745498748,-0.707106781186563,0.473146789255805));
#33848=DIRECTION('ref_axis',(0.669130606358858,0.,-0.743144825477394));
#33849=DIRECTION('',(-0.669130606358858,0.,0.743144825477394));
#33850=DIRECTION('center_axis',(-0.525482745498762,-0.707106781186544,-0.473146789255818));
#33851=DIRECTION('ref_axis',(-0.669130606358858,0.,0.743144825477394));
#33852=DIRECTION('',(0.669130606358858,0.,-0.743144825477394));
#33853=DIRECTION('center_axis',(0.743144825477394,0.,0.669130606358858));
#33854=DIRECTION('ref_axis',(0.669130606358858,0.,-0.743144825477394));
#33855=DIRECTION('',(0.,1.,0.));
#33856=DIRECTION('',(0.669130606358858,0.,-0.743144825477394));
#33857=DIRECTION('center_axis',(-0.669130606358858,0.,0.743144825477394));
#33858=DIRECTION('ref_axis',(0.743144825477394,0.,0.669130606358858));
#33859=DIRECTION('',(0.,1.,0.));
#33860=DIRECTION('',(0.743144825477394,0.,0.669130606358858));
#33861=DIRECTION('center_axis',(0.353553390593272,-0.707106781186551,-0.612372435695792));
#33862=DIRECTION('ref_axis',(-0.866025403784439,0.,-0.5));
#33863=DIRECTION('',(0.788675134594812,0.577350269189624,-0.211324865405195));
#33864=DIRECTION('',(0.866025403784439,0.,0.5));
#33865=DIRECTION('',(0.211324865405161,-0.577350269189619,0.788675134594825));
#33866=DIRECTION('center_axis',(0.612372435695798,-0.707106781186544,0.353553390593276));
#33867=DIRECTION('ref_axis',(0.5,0.,-0.866025403784439));
#33868=DIRECTION('',(-0.5,0.,0.866025403784439));
#33869=DIRECTION('center_axis',(-0.612372435695801,-0.70710678118654,-0.353553390593278));
#33870=DIRECTION('ref_axis',(-0.5,0.,0.866025403784439));
#33871=DIRECTION('',(0.5,0.,-0.866025403784439));
#33872=DIRECTION('center_axis',(0.218508012224414,-0.707106781186536,-0.672498511963969));
#33873=DIRECTION('ref_axis',(-0.951056516295153,0.,-0.309016994374947));
#33874=DIRECTION('',(0.727503780584104,0.577350269189638,-0.370681690810982));
#33875=DIRECTION('',(0.951056516295154,0.,0.309016994374948));
#33876=DIRECTION('',(0.370681690811009,-0.57735026918962,0.727503780584104));
#33877=DIRECTION('center_axis',(0.672498511963958,-0.707106781186547,0.218508012224411));
#33878=DIRECTION('ref_axis',(0.309016994374947,0.,-0.951056516295154));
#33879=DIRECTION('',(-0.309016994374948,0.,0.951056516295154));
#33880=DIRECTION('center_axis',(-0.672498511963955,-0.707106781186549,-0.21850801222441));
#33881=DIRECTION('ref_axis',(-0.309016994374947,0.,0.951056516295154));
#33882=DIRECTION('',(0.309016994374948,0.,-0.951056516295154));
#33883=DIRECTION('center_axis',(0.951056516295154,0.,0.309016994374948));
#33884=DIRECTION('ref_axis',(0.309016994374948,0.,-0.951056516295154));
#33885=DIRECTION('',(0.,1.,0.));
#33886=DIRECTION('',(0.309016994374948,0.,-0.951056516295154));
#33887=DIRECTION('center_axis',(-0.309016994374948,0.,0.951056516295154));
#33888=DIRECTION('ref_axis',(0.951056516295154,0.,0.309016994374948));
#33889=DIRECTION('',(0.,1.,0.));
#33890=DIRECTION('',(0.951056516295154,0.,0.309016994374948));
#33891=DIRECTION('center_axis',(-0.703233176253405,-0.707106781186547,-0.0739127852035669));
#33892=DIRECTION('ref_axis',(-0.104528463267654,0.,0.994521895368273));
#33893=DIRECTION('',(0.513837947600284,-0.57735026918962,0.634537020411419));
#33894=DIRECTION('',(0.104528463267654,0.,-0.994521895368273));
#33895=DIRECTION('center_axis',(0.0739127852035657,-0.707106781186559,-0.703233176253393));
#33896=DIRECTION('ref_axis',(-0.994521895368273,0.,-0.104528463267654));
#33897=DIRECTION('',(0.994521895368273,0.,0.104528463267654));
#33898=DIRECTION('',(0.634537020411406,0.577350269189623,-0.513837947600297));
#33899=DIRECTION('center_axis',(0.703233176253404,-0.707106781186547,0.0739127852035669));
#33900=DIRECTION('ref_axis',(0.104528463267654,0.,-0.994521895368273));
#33901=DIRECTION('',(-0.104528463267654,0.,0.994521895368273));
#33902=DIRECTION('center_axis',(-0.0739127852035663,-0.707106781186551,
-0.703233176253401));
#33903=DIRECTION('ref_axis',(-0.994521895368273,0.,0.104528463267653));
#33904=DIRECTION('',(0.513837947600291,0.577350269189624,-0.634537020411409));
#33905=DIRECTION('',(0.994521895368273,0.,-0.104528463267653));
#33906=DIRECTION('',(0.63453702041141,-0.577350269189627,0.513837947600287));
#33907=DIRECTION('center_axis',(0.703233176253405,-0.707106781186546,-0.0739127852035667));
#33908=DIRECTION('ref_axis',(-0.104528463267653,0.,-0.994521895368273));
#33909=DIRECTION('',(0.104528463267653,0.,0.994521895368273));
#33910=DIRECTION('center_axis',(-0.703233176253403,-0.707106781186549,0.0739127852035665));
#33911=DIRECTION('ref_axis',(0.104528463267653,0.,0.994521895368273));
#33912=DIRECTION('',(-0.104528463267653,0.,-0.994521895368273));
#33913=DIRECTION('center_axis',(-0.218508012224409,-0.707106781186552,-0.672498511963953));
#33914=DIRECTION('ref_axis',(-0.951056516295154,0.,0.309016994374947));
#33915=DIRECTION('',(0.370681690811016,0.577350269189631,-0.727503780584092));
#33916=DIRECTION('',(0.951056516295154,0.,-0.309016994374947));
#33917=DIRECTION('',(0.727503780584105,-0.577350269189631,0.370681690810991));
#33918=DIRECTION('center_axis',(0.672498511963956,-0.707106781186549,-0.21850801222441));
#33919=DIRECTION('ref_axis',(-0.309016994374947,0.,-0.951056516295154));
#33920=DIRECTION('',(0.309016994374947,0.,0.951056516295154));
#33921=DIRECTION('center_axis',(-0.672498511963956,-0.70710678118655,0.21850801222441));
#33922=DIRECTION('ref_axis',(0.309016994374947,0.,0.951056516295154));
#33923=DIRECTION('',(-0.309016994374947,0.,-0.951056516295154));
#33924=DIRECTION('center_axis',(0.951056516295154,0.,-0.309016994374947));
#33925=DIRECTION('ref_axis',(-0.309016994374947,0.,-0.951056516295154));
#33926=DIRECTION('',(0.,1.,0.));
#33927=DIRECTION('',(-0.309016994374947,0.,-0.951056516295154));
#33928=DIRECTION('center_axis',(0.309016994374947,0.,0.951056516295154));
#33929=DIRECTION('ref_axis',(0.951056516295154,0.,-0.309016994374947));
#33930=DIRECTION('',(0.,1.,0.));
#33931=DIRECTION('',(0.951056516295154,0.,-0.309016994374947));
#33932=DIRECTION('center_axis',(-0.353553390593278,-0.70710678118654,-0.612372435695801));
#33933=DIRECTION('ref_axis',(-0.866025403784439,0.,0.5));
#33934=DIRECTION('',(0.21132486540519,0.577350269189628,-0.788675134594811));
#33935=DIRECTION('',(0.866025403784439,0.,-0.5));
#33936=DIRECTION('',(0.788675134594814,-0.577350269189626,0.211324865405183));
#33937=DIRECTION('center_axis',(0.612372435695794,-0.707106781186548,-0.353553390593274));
#33938=DIRECTION('ref_axis',(-0.5,0.,-0.866025403784439));
#33939=DIRECTION('',(0.5,0.,0.866025403784439));
#33940=DIRECTION('center_axis',(-0.612372435695791,-0.707106781186552,0.353553390593272));
#33941=DIRECTION('ref_axis',(0.5,0.,0.866025403784439));
#33942=DIRECTION('',(-0.5,0.,-0.866025403784439));
#33943=DIRECTION('center_axis',(-0.473146789255817,-0.707106781186544,-0.525482745498761));
#33944=DIRECTION('ref_axis',(-0.743144825477394,0.,0.669130606358858));
#33945=DIRECTION('',(0.0427321293319396,0.57735026918963,-0.815377600740553));
#33946=DIRECTION('',(0.743144825477394,0.,-0.669130606358858));
#33947=DIRECTION('',(0.815377600740554,-0.577350269189626,0.0427321293319778));
#33948=DIRECTION('center_axis',(0.525482745498765,-0.70710678118654,-0.47314678925582));
#33949=DIRECTION('ref_axis',(-0.669130606358858,0.,-0.743144825477394));
#33950=DIRECTION('',(0.669130606358858,0.,0.743144825477394));
#33951=DIRECTION('center_axis',(-0.525482745498768,-0.707106781186536,0.473146789255823));
#33952=DIRECTION('ref_axis',(0.669130606358858,0.,0.743144825477394));
#33953=DIRECTION('',(-0.669130606358858,0.,-0.743144825477394));
#33954=DIRECTION('center_axis',(0.743144825477394,0.,-0.669130606358858));
#33955=DIRECTION('ref_axis',(-0.669130606358858,0.,-0.743144825477394));
#33956=DIRECTION('',(0.,1.,0.));
#33957=DIRECTION('',(-0.669130606358858,0.,-0.743144825477394));
#33958=DIRECTION('center_axis',(0.669130606358858,0.,0.743144825477394));
#33959=DIRECTION('ref_axis',(0.743144825477394,0.,-0.669130606358858));
#33960=DIRECTION('',(0.,1.,0.));
#33961=DIRECTION('',(0.743144825477394,0.,-0.669130606358858));
#33962=DIRECTION('center_axis',(-0.572061402817686,-0.707106781186545,-0.415626937777455));
#33963=DIRECTION('ref_axis',(-0.587785252292473,0.,0.809016994374947));
#33964=DIRECTION('',(-0.127728205844599,0.577350269189625,-0.806444153118111));
#33965=DIRECTION('',(0.587785252292473,0.,-0.809016994374947));
#33966=DIRECTION('',(0.806444153118105,-0.57735026918963,-0.127728205844613));
#33967=DIRECTION('center_axis',(0.415626937777452,-0.707106781186551,-0.572061402817682));
#33968=DIRECTION('ref_axis',(-0.809016994374947,0.,-0.587785252292473));
#33969=DIRECTION('',(0.809016994374947,0.,0.587785252292473));
#33970=DIRECTION('center_axis',(-0.415626937777454,-0.707106781186547,0.572061402817684));
#33971=DIRECTION('ref_axis',(0.809016994374947,0.,0.587785252292473));
#33972=DIRECTION('',(-0.809016994374947,0.,-0.587785252292473));
#33973=DIRECTION('center_axis',(-0.645974188021245,-0.707106781186554,-0.287606238475948));
#33974=DIRECTION('ref_axis',(-0.4067366430758,0.,0.913545457642601));
#33975=DIRECTION('',(-0.292606205517836,0.577350269189618,-0.762265226256012));
#33976=DIRECTION('',(0.4067366430758,0.,-0.913545457642601));
#33977=DIRECTION('',(0.762265226256022,-0.577350269189626,-0.292606205517795));
#33978=DIRECTION('center_axis',(0.287606238475952,-0.707106781186546,-0.645974188021253));
#33979=DIRECTION('ref_axis',(-0.913545457642601,0.,-0.4067366430758));
#33980=DIRECTION('',(0.913545457642601,0.,0.4067366430758));
#33981=DIRECTION('center_axis',(-0.287606238475956,-0.707106781186536,0.645974188021262));
#33982=DIRECTION('ref_axis',(0.913545457642601,0.,0.4067366430758));
#33983=DIRECTION('',(-0.913545457642601,0.,-0.4067366430758));
#33984=DIRECTION('center_axis',(0.4067366430758,0.,-0.913545457642601));
#33985=DIRECTION('ref_axis',(-0.913545457642601,0.,-0.4067366430758));
#33986=DIRECTION('',(0.,1.,0.));
#33987=DIRECTION('',(-0.913545457642601,0.,-0.4067366430758));
#33988=DIRECTION('center_axis',(0.913545457642601,0.,0.4067366430758));
#33989=DIRECTION('ref_axis',(0.4067366430758,0.,-0.913545457642601));
#33990=DIRECTION('',(0.,1.,0.));
#33991=DIRECTION('',(0.4067366430758,0.,-0.913545457642601));
#33992=DIRECTION('center_axis',(-0.691654801480242,-0.70710678118653,-0.147015766465202));
#33993=DIRECTION('ref_axis',(-0.20791169081776,0.,0.978147600733805));
#33994=DIRECTION('',(-0.44469590992953,0.577350269189636,-0.684771651252154));
#33995=DIRECTION('',(0.20791169081776,0.,-0.978147600733805));
#33996=DIRECTION('',(0.684771651252131,-0.577350269189634,-0.44469590992957));
#33997=DIRECTION('center_axis',(0.1470157664652,-0.707106781186543,-0.69165480148023));
#33998=DIRECTION('ref_axis',(-0.978147600733805,0.,-0.20791169081776));
#33999=DIRECTION('',(0.978147600733805,0.,0.20791169081776));
#34000=DIRECTION('center_axis',(-0.147015766465198,-0.707106781186553,0.69165480148022));
#34001=DIRECTION('ref_axis',(0.978147600733805,0.,0.20791169081776));
#34002=DIRECTION('',(-0.978147600733805,0.,-0.20791169081776));
#34003=DIRECTION('center_axis',(-0.707106781186548,-0.707106781186548,-8.65956056235493E-17));
#34004=DIRECTION('ref_axis',(-1.22464679914735E-16,0.,1.));
#34005=DIRECTION('',(-0.577350269189625,0.577350269189625,-0.577350269189627));
#34006=DIRECTION('',(1.22464679914735E-16,0.,-1.));
#34007=DIRECTION('',(0.577350269189633,-0.57735026918962,-0.577350269189624));
#34008=DIRECTION('center_axis',(8.65956056235492E-17,-0.707106781186549,
-0.707106781186546));
#34009=DIRECTION('ref_axis',(-1.,0.,-1.22464679914735E-16));
#34010=DIRECTION('',(1.,0.,1.22464679914735E-16));
#34011=DIRECTION('center_axis',(-8.65956056235491E-17,-0.707106781186549,
0.707106781186546));
#34012=DIRECTION('ref_axis',(1.,0.,1.22464679914735E-16));
#34013=DIRECTION('',(-1.,0.,-1.22464679914735E-16));
#34014=DIRECTION('center_axis',(1.22464679914735E-16,0.,-1.));
#34015=DIRECTION('ref_axis',(-1.,0.,-1.22464679914735E-16));
#34016=DIRECTION('',(0.,1.,0.));
#34017=DIRECTION('',(-1.,0.,-1.22464679914735E-16));
#34018=DIRECTION('center_axis',(1.,0.,1.22464679914735E-16));
#34019=DIRECTION('ref_axis',(1.22464679914735E-16,0.,-1.));
#34020=DIRECTION('',(0.,1.,0.));
#34021=DIRECTION('',(1.22464679914735E-16,0.,-1.));
#34022=DIRECTION('center_axis',(-0.691654801480235,-0.707106781186538,0.1470157664652));
#34023=DIRECTION('ref_axis',(0.207911690817759,0.,0.978147600733806));
#34024=DIRECTION('',(-0.68477165125214,0.577350269189631,-0.444695909929558));
#34025=DIRECTION('',(-0.207911690817759,0.,-0.978147600733806));
#34026=DIRECTION('',(0.444695909929528,-0.577350269189634,-0.684771651252158));
#34027=DIRECTION('center_axis',(-0.147015766465198,-0.707106781186548,-0.691654801480226));
#34028=DIRECTION('ref_axis',(-0.978147600733806,0.,0.207911690817759));
#34029=DIRECTION('',(0.978147600733806,0.,-0.207911690817759));
#34030=DIRECTION('center_axis',(0.147015766465198,-0.707106781186549,0.691654801480225));
#34031=DIRECTION('ref_axis',(0.978147600733806,0.,-0.207911690817759));
#34032=DIRECTION('',(-0.978147600733806,0.,0.207911690817759));
#34033=DIRECTION('center_axis',(-0.645974188021266,-0.707106781186531,0.287606238475957));
#34034=DIRECTION('ref_axis',(0.4067366430758,0.,0.913545457642601));
#34035=DIRECTION('',(-0.762265226255999,0.577350269189637,-0.292606205517833));
#34036=DIRECTION('',(-0.4067366430758,0.,-0.913545457642601));
#34037=DIRECTION('',(0.29260620551779,-0.57735026918963,-0.762265226256021));
#34038=DIRECTION('center_axis',(-0.28760623847595,-0.707106781186549,-0.64597418802125));
#34039=DIRECTION('ref_axis',(-0.913545457642601,0.,0.4067366430758));
#34040=DIRECTION('',(0.913545457642601,0.,-0.4067366430758));
#34041=DIRECTION('center_axis',(0.287606238475948,-0.707106781186554,0.645974188021245));
#34042=DIRECTION('ref_axis',(0.913545457642601,0.,-0.4067366430758));
#34043=DIRECTION('',(-0.913545457642601,0.,0.4067366430758));
#34044=DIRECTION('center_axis',(-0.4067366430758,0.,-0.913545457642601));
#34045=DIRECTION('ref_axis',(-0.913545457642601,0.,0.4067366430758));
#34046=DIRECTION('',(0.,1.,0.));
#34047=DIRECTION('',(-0.913545457642601,0.,0.4067366430758));
#34048=DIRECTION('center_axis',(0.913545457642601,0.,-0.4067366430758));
#34049=DIRECTION('ref_axis',(-0.4067366430758,0.,-0.913545457642601));
#34050=DIRECTION('',(0.,1.,0.));
#34051=DIRECTION('',(-0.4067366430758,0.,-0.913545457642601));
#34052=DIRECTION('center_axis',(-0.572061402817692,-0.707106781186538,0.415626937777459));
#34053=DIRECTION('ref_axis',(0.587785252292473,0.,0.809016994374947));
#34054=DIRECTION('',(-0.806444153118102,0.577350269189636,-0.127728205844608));
#34055=DIRECTION('',(-0.587785252292473,0.,-0.809016994374947));
#34056=DIRECTION('',(0.127728205844599,-0.577350269189625,-0.806444153118111));
#34057=DIRECTION('center_axis',(-0.415626937777457,-0.707106781186541,-0.57206140281769));
#34058=DIRECTION('ref_axis',(-0.809016994374947,0.,0.587785252292473));
#34059=DIRECTION('',(0.809016994374947,0.,-0.587785252292473));
#34060=DIRECTION('center_axis',(0.415626937777451,-0.707106781186552,0.572061402817681));
#34061=DIRECTION('ref_axis',(0.809016994374947,0.,-0.587785252292473));
#34062=DIRECTION('',(-0.809016994374947,0.,0.587785252292473));
#34063=DIRECTION('center_axis',(-0.473146789255816,-0.707106781186547,0.525482745498759));
#34064=DIRECTION('ref_axis',(0.743144825477394,0.,0.669130606358858));
#34065=DIRECTION('',(-0.815377600740555,0.577350269189626,0.0427321293319522));
#34066=DIRECTION('',(-0.743144825477394,0.,-0.669130606358858));
#34067=DIRECTION('',(-0.0427321293319396,-0.57735026918963,-0.815377600740553));
#34068=DIRECTION('center_axis',(-0.525482745498763,-0.707106781186542,-0.473146789255819));
#34069=DIRECTION('ref_axis',(-0.669130606358858,0.,0.743144825477394));
#34070=DIRECTION('',(0.669130606358858,0.,-0.743144825477394));
#34071=DIRECTION('center_axis',(0.525482745498763,-0.707106781186542,0.473146789255819));
#34072=DIRECTION('ref_axis',(0.669130606358858,0.,-0.743144825477394));
#34073=DIRECTION('',(-0.669130606358858,0.,0.743144825477394));
#34074=DIRECTION('center_axis',(-0.743144825477394,0.,-0.669130606358858));
#34075=DIRECTION('ref_axis',(-0.669130606358858,0.,0.743144825477394));
#34076=DIRECTION('',(0.,1.,0.));
#34077=DIRECTION('',(-0.669130606358858,0.,0.743144825477394));
#34078=DIRECTION('center_axis',(0.669130606358858,0.,-0.743144825477394));
#34079=DIRECTION('ref_axis',(-0.743144825477394,0.,-0.669130606358858));
#34080=DIRECTION('',(0.,1.,0.));
#34081=DIRECTION('',(-0.743144825477394,0.,-0.669130606358858));
#34082=DIRECTION('center_axis',(-0.353553390593269,-0.707106781186558,0.612372435695785));
#34083=DIRECTION('ref_axis',(0.866025403784438,0.,0.5));
#34084=DIRECTION('',(0.788675134594818,-0.577350269189616,-0.211324865405193));
#34085=DIRECTION('',(-0.866025403784438,0.,-0.5));
#34086=DIRECTION('',(-0.211324865405179,-0.577350269189617,-0.788675134594822));
#34087=DIRECTION('center_axis',(0.612372435695789,-0.707106781186554,0.353553390593271));
#34088=DIRECTION('ref_axis',(0.5,0.,-0.866025403784438));
#34089=DIRECTION('',(-0.5,0.,0.866025403784438));
#34090=DIRECTION('center_axis',(-0.612372435695789,-0.707106781186554,-0.353553390593271));
#34091=DIRECTION('ref_axis',(-0.5,0.,0.866025403784438));
#34092=DIRECTION('',(0.5,0.,-0.866025403784438));
#34093=DIRECTION('center_axis',(-0.218508012224412,-0.707106781186544,0.67249851196396));
#34094=DIRECTION('ref_axis',(0.951056516295153,0.,0.309016994374948));
#34095=DIRECTION('',(-0.727503780584099,0.577350269189631,0.370681690811003));
#34096=DIRECTION('',(-0.951056516295153,0.,-0.309016994374948));
#34097=DIRECTION('',(-0.370681690811016,-0.577350269189631,-0.727503780584092));
#34098=DIRECTION('center_axis',(-0.672498511963956,-0.707106781186549,-0.21850801222441));
#34099=DIRECTION('ref_axis',(-0.309016994374948,0.,0.951056516295154));
#34100=DIRECTION('',(0.309016994374948,0.,-0.951056516295153));
#34101=DIRECTION('center_axis',(0.672498511963956,-0.707106781186549,0.21850801222441));
#34102=DIRECTION('ref_axis',(0.309016994374948,0.,-0.951056516295154));
#34103=DIRECTION('',(-0.309016994374948,0.,0.951056516295153));
#34104=DIRECTION('center_axis',(-0.0739127852035669,-0.707106781186551,
0.703233176253401));
#34105=DIRECTION('ref_axis',(0.994521895368273,0.,0.104528463267654));
#34106=DIRECTION('',(-0.634537020411406,0.577350269189623,0.513837947600297));
#34107=DIRECTION('',(-0.994521895368273,0.,-0.104528463267654));
#34108=DIRECTION('',(-0.513837947600291,-0.577350269189624,-0.634537020411409));
#34109=DIRECTION('center_axis',(-0.703233176253405,-0.707106781186547,-0.0739127852035674));
#34110=DIRECTION('ref_axis',(-0.104528463267654,0.,0.994521895368273));
#34111=DIRECTION('',(0.104528463267654,0.,-0.994521895368273));
#34112=DIRECTION('center_axis',(0.703233176253405,-0.707106781186547,0.0739127852035674));
#34113=DIRECTION('ref_axis',(0.104528463267654,0.,-0.994521895368273));
#34114=DIRECTION('',(-0.104528463267654,0.,0.994521895368273));
#34115=DIRECTION('center_axis',(-0.994521895368273,0.,-0.104528463267654));
#34116=DIRECTION('ref_axis',(-0.104528463267654,0.,0.994521895368273));
#34117=DIRECTION('',(0.,1.,0.));
#34118=DIRECTION('',(-0.104528463267654,0.,0.994521895368273));
#34119=DIRECTION('center_axis',(0.104528463267654,0.,-0.994521895368273));
#34120=DIRECTION('ref_axis',(-0.994521895368273,0.,-0.104528463267654));
#34121=DIRECTION('',(0.,1.,0.));
#34122=DIRECTION('',(-0.994521895368273,0.,-0.104528463267654));
#34123=DIRECTION('center_axis',(0.0739127852035652,-0.707106781186559,0.703233176253393));
#34124=DIRECTION('ref_axis',(0.994521895368273,0.,-0.104528463267653));
#34125=DIRECTION('',(-0.513837947600285,0.577350269189621,0.634537020411417));
#34126=DIRECTION('',(-0.994521895368273,0.,0.104528463267653));
#34127=DIRECTION('',(-0.6345370204114,-0.57735026918962,-0.513837947600307));
#34128=DIRECTION('center_axis',(-0.703233176253405,-0.707106781186547,0.0739127852035665));
#34129=DIRECTION('ref_axis',(0.104528463267653,0.,0.994521895368274));
#34130=DIRECTION('',(-0.104528463267653,0.,-0.994521895368273));
#34131=DIRECTION('center_axis',(0.703233176253406,-0.707106781186546,-0.0739127852035666));
#34132=DIRECTION('ref_axis',(-0.104528463267653,0.,-0.994521895368273));
#34133=DIRECTION('',(0.104528463267653,0.,0.994521895368273));
#34134=DIRECTION('center_axis',(0.218508012224411,-0.707106781186545,0.67249851196396));
#34135=DIRECTION('ref_axis',(0.951056516295154,0.,-0.309016994374947));
#34136=DIRECTION('',(-0.370681690811007,0.577350269189627,0.7275037805841));
#34137=DIRECTION('',(-0.951056516295154,0.,0.309016994374947));
#34138=DIRECTION('',(-0.7275037805841,-0.577350269189629,-0.370681690811002));
#34139=DIRECTION('center_axis',(-0.672498511963959,-0.707106781186545,0.218508012224411));
#34140=DIRECTION('ref_axis',(0.309016994374947,0.,0.951056516295154));
#34141=DIRECTION('',(-0.309016994374947,0.,-0.951056516295154));
#34142=DIRECTION('center_axis',(0.672498511963956,-0.707106781186549,-0.21850801222441));
#34143=DIRECTION('ref_axis',(-0.309016994374947,0.,-0.951056516295154));
#34144=DIRECTION('',(0.309016994374947,0.,0.951056516295154));
#34145=DIRECTION('center_axis',(-0.951056516295154,0.,0.309016994374947));
#34146=DIRECTION('ref_axis',(0.309016994374947,0.,0.951056516295154));
#34147=DIRECTION('',(0.,1.,0.));
#34148=DIRECTION('',(0.309016994374947,0.,0.951056516295154));
#34149=DIRECTION('center_axis',(-0.309016994374947,0.,-0.951056516295154));
#34150=DIRECTION('ref_axis',(-0.951056516295154,0.,0.309016994374947));
#34151=DIRECTION('',(0.,1.,0.));
#34152=DIRECTION('',(-0.951056516295154,0.,0.309016994374947));
#34153=DIRECTION('center_axis',(0.353553390593277,-0.70710678118654,0.612372435695802));
#34154=DIRECTION('ref_axis',(0.866025403784439,0.,-0.499999999999999));
#34155=DIRECTION('',(-0.211324865405186,0.577350269189634,0.788675134594807));
#34156=DIRECTION('',(-0.866025403784439,0.,0.499999999999999));
#34157=DIRECTION('',(-0.788675134594814,-0.577350269189626,-0.211324865405183));
#34158=DIRECTION('center_axis',(-0.612372435695802,-0.70710678118654,0.353553390593277));
#34159=DIRECTION('ref_axis',(0.499999999999999,0.,0.866025403784439));
#34160=DIRECTION('',(-0.499999999999999,0.,-0.866025403784439));
#34161=DIRECTION('center_axis',(0.612372435695792,-0.707106781186551,-0.353553390593272));
#34162=DIRECTION('ref_axis',(-0.499999999999999,0.,-0.866025403784439));
#34163=DIRECTION('',(0.499999999999999,0.,0.866025403784439));
#34164=DIRECTION('center_axis',(0.473146789255817,-0.707106781186544,0.525482745498762));
#34165=DIRECTION('ref_axis',(0.743144825477395,0.,-0.669130606358858));
#34166=DIRECTION('',(-0.0427321293319524,0.577350269189629,0.815377600740553));
#34167=DIRECTION('',(-0.743144825477395,0.,0.669130606358858));
#34168=DIRECTION('',(-0.81537760074055,-0.577350269189632,-0.0427321293319527));
#34169=DIRECTION('center_axis',(-0.525482745498762,-0.707106781186544,0.473146789255817));
#34170=DIRECTION('ref_axis',(0.669130606358858,0.,0.743144825477395));
#34171=DIRECTION('',(-0.669130606358858,0.,-0.743144825477395));
#34172=DIRECTION('center_axis',(0.525482745498764,-0.707106781186541,-0.473146789255819));
#34173=DIRECTION('ref_axis',(-0.669130606358858,0.,-0.743144825477395));
#34174=DIRECTION('',(0.669130606358858,0.,0.743144825477395));
#34175=DIRECTION('center_axis',(-0.743144825477395,0.,0.669130606358858));
#34176=DIRECTION('ref_axis',(0.669130606358858,0.,0.743144825477395));
#34177=DIRECTION('',(0.,1.,0.));
#34178=DIRECTION('',(0.669130606358858,0.,0.743144825477395));
#34179=DIRECTION('center_axis',(-0.669130606358858,0.,-0.743144825477395));
#34180=DIRECTION('ref_axis',(-0.743144825477395,0.,0.669130606358858));
#34181=DIRECTION('',(0.,1.,0.));
#34182=DIRECTION('',(-0.743144825477395,0.,0.669130606358858));
#34183=DIRECTION('center_axis',(0.415626937777451,-0.707106781186552,-0.572061402817681));
#34184=DIRECTION('ref_axis',(-0.809016994374947,0.,-0.587785252292473));
#34185=DIRECTION('',(-0.806444153118105,-0.577350269189629,0.127728205844622));
#34186=DIRECTION('',(0.809016994374947,0.,0.587785252292473));
#34187=DIRECTION('center_axis',(0.572061402817692,-0.707106781186538,0.415626937777459));
#34188=DIRECTION('ref_axis',(0.587785252292473,0.,-0.809016994374947));
#34189=DIRECTION('',(-0.587785252292473,0.,0.809016994374947));
#34190=DIRECTION('',(0.1277282058446,0.577350269189631,0.806444153118107));
#34191=DIRECTION('center_axis',(-0.415626937777453,-0.707106781186549,0.572061402817683));
#34192=DIRECTION('ref_axis',(0.809016994374947,0.,0.587785252292473));
#34193=DIRECTION('',(-0.809016994374947,0.,-0.587785252292473));
#34194=DIRECTION('center_axis',(0.64597418802125,-0.707106781186549,0.287606238475951));
#34195=DIRECTION('ref_axis',(0.406736643075801,0.,-0.913545457642601));
#34196=DIRECTION('',(0.292606205517828,0.577350269189629,0.762265226256007));
#34197=DIRECTION('',(-0.406736643075801,0.,0.913545457642601));
#34198=DIRECTION('',(-0.762265226256014,-0.577350269189619,0.29260620551783));
#34199=DIRECTION('center_axis',(-0.287606238475954,-0.70710678118654,0.645974188021258));
#34200=DIRECTION('ref_axis',(0.913545457642601,0.,0.406736643075801));
#34201=DIRECTION('',(-0.913545457642601,0.,-0.406736643075801));
#34202=DIRECTION('center_axis',(0.287606238475947,-0.707106781186558,-0.645974188021242));
#34203=DIRECTION('ref_axis',(-0.913545457642601,0.,-0.406736643075801));
#34204=DIRECTION('',(0.913545457642601,0.,0.406736643075801));
#34205=DIRECTION('center_axis',(0.691654801480227,-0.707106781186546,0.147015766465199));
#34206=DIRECTION('ref_axis',(0.20791169081776,0.,-0.978147600733805));
#34207=DIRECTION('',(0.444695909929549,0.577350269189628,0.684771651252149));
#34208=DIRECTION('',(-0.20791169081776,0.,0.978147600733805));
#34209=DIRECTION('',(-0.68477165125215,-0.577350269189629,0.444695909929547));
#34210=DIRECTION('center_axis',(-0.1470157664652,-0.707106781186542,0.69165480148023));
#34211=DIRECTION('ref_axis',(0.978147600733805,0.,0.20791169081776));
#34212=DIRECTION('',(-0.978147600733805,0.,-0.20791169081776));
#34213=DIRECTION('center_axis',(0.147015766465199,-0.707106781186549,-0.691654801480225));
#34214=DIRECTION('ref_axis',(-0.978147600733805,0.,-0.20791169081776));
#34215=DIRECTION('',(0.978147600733805,0.,0.20791169081776));
#34216=DIRECTION('center_axis',(-0.20791169081776,0.,0.978147600733806));
#34217=DIRECTION('ref_axis',(0.978147600733805,0.,0.20791169081776));
#34218=DIRECTION('',(0.,1.,0.));
#34219=DIRECTION('',(0.978147600733805,0.,0.20791169081776));
#34220=DIRECTION('center_axis',(-0.978147600733806,0.,-0.20791169081776));
#34221=DIRECTION('ref_axis',(-0.20791169081776,0.,0.978147600733805));
#34222=DIRECTION('',(0.,1.,0.));
#34223=DIRECTION('',(-0.20791169081776,0.,0.978147600733805));
#34224=DIRECTION('center_axis',(0.707106781186548,0.707106781186548,0.));
#34225=DIRECTION('ref_axis',(0.,0.,-1.));
#34226=DIRECTION('',(0.577350269189626,-0.577350269189626,-0.577350269189625));
#34227=DIRECTION('',(0.,0.,-1.));
#34228=DIRECTION('',(-0.577350269189624,0.577350269189627,-0.577350269189626));
#34229=DIRECTION('center_axis',(0.,0.707106781186547,-0.707106781186548));
#34230=DIRECTION('ref_axis',(-1.,0.,0.));
#34231=DIRECTION('center_axis',(0.,-0.707106781186547,0.707106781186548));
#34232=DIRECTION('ref_axis',(0.,0.707106781186548,0.707106781186546));
#34233=DIRECTION('',(-1.,0.,0.));
#34234=DIRECTION('center_axis',(0.,0.707106781186547,0.707106781186548));
#34235=DIRECTION('ref_axis',(1.,0.,0.));
#34236=DIRECTION('',(1.,0.,0.));
#34237=DIRECTION('center_axis',(0.,-0.707106781186547,-0.707106781186548));
#34238=DIRECTION('ref_axis',(0.,-0.707106781186548,0.707106781186546));
#34239=DIRECTION('center_axis',(0.,0.,-1.));
#34240=DIRECTION('ref_axis',(-1.,0.,0.));
#34241=DIRECTION('',(0.,1.,0.));
#34242=DIRECTION('',(-1.,0.,0.));
#34243=DIRECTION('',(0.,-1.,0.));
#34244=DIRECTION('center_axis',(-1.,0.,0.));
#34245=DIRECTION('ref_axis',(0.,0.,1.));
#34246=DIRECTION('',(0.,1.,0.));
#34247=DIRECTION('',(0.,0.,1.));
#34248=DIRECTION('center_axis',(0.,0.,1.));
#34249=DIRECTION('ref_axis',(1.,0.,0.));
#34250=DIRECTION('',(0.,1.,0.));
#34251=DIRECTION('',(1.,0.,0.));
#34252=DIRECTION('center_axis',(0.,1.,0.));
#34253=DIRECTION('ref_axis',(0.,0.,1.));
#34254=DIRECTION('center_axis',(0.,-0.707106781186547,0.707106781186548));
#34255=DIRECTION('ref_axis',(0.,0.707106781186548,0.707106781186546));
#34256=DIRECTION('',(0.,-1.,0.));
#34257=DIRECTION('center_axis',(0.,0.707106781186547,0.707106781186548));
#34258=DIRECTION('ref_axis',(0.,-0.707106781186548,0.707106781186546));
#34259=DIRECTION('center_axis',(0.,0.707106781186547,0.707106781186548));
#34260=DIRECTION('ref_axis',(0.,-0.707106781186548,0.707106781186546));
#34261=DIRECTION('center_axis',(0.707106781186548,-0.707106781186548,0.));
#34262=DIRECTION('ref_axis',(0.,0.,-1.));
#34263=DIRECTION('',(-0.577350269189626,-0.577350269189626,0.577350269189625));
#34264=DIRECTION('',(0.577350269189624,0.577350269189627,0.577350269189626));
#34265=DIRECTION('center_axis',(0.,-0.707106781186547,-0.707106781186548));
#34266=DIRECTION('ref_axis',(-1.,0.,0.));
#34267=DIRECTION('center_axis',(0.,-0.707106781186547,0.707106781186548));
#34268=DIRECTION('ref_axis',(1.,0.,0.));
#34269=DIRECTION('center_axis',(0.,0.707106781186547,-0.707106781186548));
#34270=DIRECTION('ref_axis',(0.,0.707106781186548,0.707106781186546));
#34271=DIRECTION('center_axis',(0.,-0.707106781186547,0.707106781186548));
#34272=DIRECTION('ref_axis',(1.,0.,0.));
#34273=DIRECTION('',(-1.,0.,0.));
#34274=DIRECTION('center_axis',(0.,0.707106781186547,-0.707106781186548));
#34275=DIRECTION('ref_axis',(0.,0.707106781186548,0.707106781186546));
#34276=DIRECTION('',(-0.577350269189626,0.577350269189626,0.577350269189625));
#34277=DIRECTION('center_axis',(-0.707106781186548,-0.707106781186548,0.));
#34278=DIRECTION('ref_axis',(0.,0.,1.));
#34279=DIRECTION('',(-0.577350269189624,0.577350269189627,-0.577350269189626));
#34280=DIRECTION('',(0.,0.,-1.));
#34281=DIRECTION('center_axis',(0.,-0.707106781186547,-0.707106781186548));
#34282=DIRECTION('ref_axis',(-1.,0.,0.));
#34283=DIRECTION('',(1.,0.,0.));
#34284=DIRECTION('center_axis',(0.,0.,-1.));
#34285=DIRECTION('ref_axis',(-1.,0.,0.));
#34286=DIRECTION('',(0.,1.,0.));
#34287=DIRECTION('',(1.,0.,0.));
#34288=DIRECTION('',(0.,1.,0.));
#34289=DIRECTION('center_axis',(1.,0.,0.));
#34290=DIRECTION('ref_axis',(0.,0.,-1.));
#34291=DIRECTION('',(0.,1.,0.));
#34292=DIRECTION('',(0.,0.,1.));
#34293=DIRECTION('center_axis',(0.,0.,1.));
#34294=DIRECTION('ref_axis',(1.,0.,0.));
#34295=DIRECTION('',(-1.,0.,0.));
#34296=DIRECTION('center_axis',(0.,0.707106781186547,0.707106781186548));
#34297=DIRECTION('ref_axis',(1.,0.,0.));
#34298=DIRECTION('center_axis',(0.,-0.707106781186547,-0.707106781186548));
#34299=DIRECTION('ref_axis',(0.,-0.707106781186548,0.707106781186546));
#34300=DIRECTION('',(0.577350269189626,0.577350269189626,-0.577350269189625));
#34301=DIRECTION('center_axis',(-0.707106781186548,0.707106781186548,0.));
#34302=DIRECTION('ref_axis',(0.,0.,1.));
#34303=DIRECTION('',(0.577350269189624,0.577350269189627,0.577350269189626));
#34304=DIRECTION('center_axis',(0.,0.707106781186547,-0.707106781186548));
#34305=DIRECTION('ref_axis',(-1.,0.,0.));
#34306=DIRECTION('center_axis',(0.,-1.,0.));
#34307=DIRECTION('ref_axis',(0.20791169081776,0.,-0.978147600733805));
#34308=DIRECTION('center_axis',(0.20791169081776,0.,-0.978147600733806));
#34309=DIRECTION('ref_axis',(-0.978147600733805,0.,-0.20791169081776));
#34310=DIRECTION('',(-0.978147600733805,0.,-0.20791169081776));
#34311=DIRECTION('center_axis',(0.,1.,0.));
#34312=DIRECTION('ref_axis',(-0.20791169081776,0.,0.978147600733805));
#34313=DIRECTION('center_axis',(0.,-1.,0.));
#34314=DIRECTION('ref_axis',(0.406736643075801,0.,-0.913545457642601));
#34315=DIRECTION('center_axis',(-0.913545457642601,0.,-0.406736643075801));
#34316=DIRECTION('ref_axis',(-0.406736643075801,0.,0.913545457642601));
#34317=DIRECTION('',(0.,1.,0.));
#34318=DIRECTION('',(-0.406736643075801,0.,0.913545457642601));
#34319=DIRECTION('',(0.,1.,0.));
#34320=DIRECTION('center_axis',(0.406736643075801,0.,-0.913545457642601));
#34321=DIRECTION('ref_axis',(-0.913545457642601,0.,-0.406736643075801));
#34322=DIRECTION('',(-0.913545457642601,0.,-0.406736643075801));
#34323=DIRECTION('center_axis',(-0.406736643075801,0.,0.913545457642601));
#34324=DIRECTION('ref_axis',(0.913545457642601,0.,0.406736643075801));
#34325=DIRECTION('',(0.913545457642601,0.,0.406736643075801));
#34326=DIRECTION('center_axis',(0.,1.,0.));
#34327=DIRECTION('ref_axis',(-0.406736643075801,0.,0.913545457642601));
#34328=DIRECTION('center_axis',(0.,-1.,0.));
#34329=DIRECTION('ref_axis',(0.587785252292473,0.,-0.809016994374947));
#34330=DIRECTION('center_axis',(-0.809016994374947,0.,-0.587785252292473));
#34331=DIRECTION('ref_axis',(-0.587785252292473,0.,0.809016994374947));
#34332=DIRECTION('',(0.,1.,0.));
#34333=DIRECTION('',(-0.587785252292473,0.,0.809016994374947));
#34334=DIRECTION('',(0.,1.,0.));
#34335=DIRECTION('center_axis',(0.587785252292473,0.,-0.809016994374947));
#34336=DIRECTION('ref_axis',(-0.809016994374947,0.,-0.587785252292473));
#34337=DIRECTION('',(-0.809016994374947,0.,-0.587785252292473));
#34338=DIRECTION('center_axis',(-0.587785252292473,0.,0.809016994374947));
#34339=DIRECTION('ref_axis',(0.809016994374947,0.,0.587785252292473));
#34340=DIRECTION('',(0.809016994374947,0.,0.587785252292473));
#34341=DIRECTION('center_axis',(0.,1.,0.));
#34342=DIRECTION('ref_axis',(-0.587785252292473,0.,0.809016994374947));
#34343=DIRECTION('center_axis',(0.,-1.,0.));
#34344=DIRECTION('ref_axis',(0.743144825477395,0.,-0.669130606358858));
#34345=DIRECTION('center_axis',(0.743144825477395,0.,-0.669130606358858));
#34346=DIRECTION('ref_axis',(-0.669130606358858,0.,-0.743144825477395));
#34347=DIRECTION('',(-0.669130606358858,0.,-0.743144825477395));
#34348=DIRECTION('center_axis',(0.,1.,0.));
#34349=DIRECTION('ref_axis',(-0.743144825477395,0.,0.669130606358858));
#34350=DIRECTION('center_axis',(0.,-1.,0.));
#34351=DIRECTION('ref_axis',(0.866025403784439,0.,-0.499999999999999));
#34352=DIRECTION('center_axis',(-0.499999999999999,0.,-0.866025403784439));
#34353=DIRECTION('ref_axis',(-0.866025403784439,0.,0.499999999999999));
#34354=DIRECTION('',(0.,1.,0.));
#34355=DIRECTION('',(-0.866025403784439,0.,0.499999999999999));
#34356=DIRECTION('',(0.,1.,0.));
#34357=DIRECTION('center_axis',(0.866025403784439,0.,-0.499999999999999));
#34358=DIRECTION('ref_axis',(-0.499999999999999,0.,-0.866025403784439));
#34359=DIRECTION('',(-0.499999999999999,0.,-0.866025403784439));
#34360=DIRECTION('center_axis',(-0.866025403784439,0.,0.499999999999999));
#34361=DIRECTION('ref_axis',(0.499999999999999,0.,0.866025403784439));
#34362=DIRECTION('',(0.499999999999999,0.,0.866025403784439));
#34363=DIRECTION('center_axis',(0.,1.,0.));
#34364=DIRECTION('ref_axis',(-0.866025403784439,0.,0.499999999999999));
#34365=DIRECTION('center_axis',(0.,-1.,0.));
#34366=DIRECTION('ref_axis',(0.951056516295154,0.,-0.309016994374947));
#34367=DIRECTION('center_axis',(0.951056516295154,0.,-0.309016994374947));
#34368=DIRECTION('ref_axis',(-0.309016994374947,0.,-0.951056516295154));
#34369=DIRECTION('',(-0.309016994374947,0.,-0.951056516295154));
#34370=DIRECTION('center_axis',(0.,1.,0.));
#34371=DIRECTION('ref_axis',(-0.951056516295154,0.,0.309016994374947));
#34372=DIRECTION('center_axis',(0.,-1.,0.));
#34373=DIRECTION('ref_axis',(0.994521895368273,0.,-0.104528463267653));
#34374=DIRECTION('center_axis',(-0.104528463267653,0.,-0.994521895368273));
#34375=DIRECTION('ref_axis',(-0.994521895368273,0.,0.104528463267653));
#34376=DIRECTION('',(0.,1.,0.));
#34377=DIRECTION('',(-0.994521895368273,0.,0.104528463267653));
#34378=DIRECTION('',(0.,1.,0.));
#34379=DIRECTION('center_axis',(0.994521895368273,0.,-0.104528463267653));
#34380=DIRECTION('ref_axis',(-0.104528463267653,0.,-0.994521895368273));
#34381=DIRECTION('',(-0.104528463267653,0.,-0.994521895368273));
#34382=DIRECTION('center_axis',(-0.994521895368273,0.,0.104528463267653));
#34383=DIRECTION('ref_axis',(0.104528463267653,0.,0.994521895368273));
#34384=DIRECTION('',(0.104528463267653,0.,0.994521895368273));
#34385=DIRECTION('center_axis',(0.,1.,0.));
#34386=DIRECTION('ref_axis',(-0.994521895368273,0.,0.104528463267653));
#34387=DIRECTION('center_axis',(0.,-1.,0.));
#34388=DIRECTION('ref_axis',(0.994521895368273,0.,0.104528463267654));
#34389=DIRECTION('center_axis',(0.994521895368273,0.,0.104528463267654));
#34390=DIRECTION('ref_axis',(0.104528463267654,0.,-0.994521895368273));
#34391=DIRECTION('',(0.104528463267654,0.,-0.994521895368273));
#34392=DIRECTION('center_axis',(0.,1.,0.));
#34393=DIRECTION('ref_axis',(-0.994521895368273,0.,-0.104528463267654));
#34394=DIRECTION('center_axis',(0.,-1.,0.));
#34395=DIRECTION('ref_axis',(0.951056516295153,0.,0.309016994374948));
#34396=DIRECTION('center_axis',(0.309016994374948,0.,-0.951056516295154));
#34397=DIRECTION('ref_axis',(-0.951056516295153,0.,-0.309016994374948));
#34398=DIRECTION('',(0.,1.,0.));
#34399=DIRECTION('',(-0.951056516295153,0.,-0.309016994374948));
#34400=DIRECTION('',(0.,1.,0.));
#34401=DIRECTION('center_axis',(0.951056516295154,0.,0.309016994374948));
#34402=DIRECTION('ref_axis',(0.309016994374948,0.,-0.951056516295153));
#34403=DIRECTION('',(0.309016994374948,0.,-0.951056516295153));
#34404=DIRECTION('center_axis',(-0.951056516295154,0.,-0.309016994374948));
#34405=DIRECTION('ref_axis',(-0.309016994374948,0.,0.951056516295153));
#34406=DIRECTION('',(-0.309016994374948,0.,0.951056516295153));
#34407=DIRECTION('center_axis',(0.,1.,0.));
#34408=DIRECTION('ref_axis',(-0.951056516295153,0.,-0.309016994374948));
#34409=DIRECTION('center_axis',(0.,-1.,0.));
#34410=DIRECTION('ref_axis',(0.866025403784438,0.,0.5));
#34411=DIRECTION('center_axis',(0.5,0.,-0.866025403784438));
#34412=DIRECTION('ref_axis',(-0.866025403784438,0.,-0.5));
#34413=DIRECTION('',(0.,1.,0.));
#34414=DIRECTION('',(-0.866025403784438,0.,-0.5));
#34415=DIRECTION('',(0.,1.,0.));
#34416=DIRECTION('center_axis',(0.866025403784438,0.,0.5));
#34417=DIRECTION('ref_axis',(0.5,0.,-0.866025403784438));
#34418=DIRECTION('',(0.5,0.,-0.866025403784438));
#34419=DIRECTION('center_axis',(-0.866025403784438,0.,-0.5));
#34420=DIRECTION('ref_axis',(-0.5,0.,0.866025403784438));
#34421=DIRECTION('',(-0.5,0.,0.866025403784438));
#34422=DIRECTION('center_axis',(0.,1.,0.));
#34423=DIRECTION('ref_axis',(-0.866025403784438,0.,-0.5));
#34424=DIRECTION('center_axis',(0.,-1.,0.));
#34425=DIRECTION('ref_axis',(0.743144825477394,0.,0.669130606358858));
#34426=DIRECTION('center_axis',(0.743144825477394,0.,0.669130606358858));
#34427=DIRECTION('ref_axis',(0.669130606358858,0.,-0.743144825477394));
#34428=DIRECTION('',(0.669130606358858,0.,-0.743144825477394));
#34429=DIRECTION('center_axis',(0.,1.,0.));
#34430=DIRECTION('ref_axis',(-0.743144825477394,0.,-0.669130606358858));
#34431=DIRECTION('center_axis',(0.,-1.,0.));
#34432=DIRECTION('ref_axis',(0.587785252292473,0.,0.809016994374947));
#34433=DIRECTION('center_axis',(0.809016994374948,0.,-0.587785252292473));
#34434=DIRECTION('ref_axis',(-0.587785252292473,0.,-0.809016994374947));
#34435=DIRECTION('',(0.,1.,0.));
#34436=DIRECTION('',(-0.587785252292473,0.,-0.809016994374947));
#34437=DIRECTION('',(0.,1.,0.));
#34438=DIRECTION('center_axis',(0.587785252292473,0.,0.809016994374948));
#34439=DIRECTION('ref_axis',(0.809016994374947,0.,-0.587785252292473));
#34440=DIRECTION('',(0.809016994374947,0.,-0.587785252292473));
#34441=DIRECTION('center_axis',(-0.587785252292473,0.,-0.809016994374948));
#34442=DIRECTION('ref_axis',(-0.809016994374947,0.,0.587785252292473));
#34443=DIRECTION('',(-0.809016994374947,0.,0.587785252292473));
#34444=DIRECTION('center_axis',(0.,1.,0.));
#34445=DIRECTION('ref_axis',(-0.587785252292473,0.,-0.809016994374947));
#34446=DIRECTION('center_axis',(0.,-1.,0.));
#34447=DIRECTION('ref_axis',(0.4067366430758,0.,0.913545457642601));
#34448=DIRECTION('center_axis',(0.4067366430758,0.,0.913545457642601));
#34449=DIRECTION('ref_axis',(0.913545457642601,0.,-0.4067366430758));
#34450=DIRECTION('',(0.913545457642601,0.,-0.4067366430758));
#34451=DIRECTION('center_axis',(0.,1.,0.));
#34452=DIRECTION('ref_axis',(-0.4067366430758,0.,-0.913545457642601));
#34453=DIRECTION('center_axis',(0.,-1.,0.));
#34454=DIRECTION('ref_axis',(0.207911690817759,0.,0.978147600733806));
#34455=DIRECTION('center_axis',(0.978147600733806,0.,-0.207911690817759));
#34456=DIRECTION('ref_axis',(-0.207911690817759,0.,-0.978147600733806));
#34457=DIRECTION('',(0.,1.,0.));
#34458=DIRECTION('',(-0.207911690817759,0.,-0.978147600733806));
#34459=DIRECTION('',(0.,1.,0.));
#34460=DIRECTION('center_axis',(0.207911690817759,0.,0.978147600733806));
#34461=DIRECTION('ref_axis',(0.978147600733806,0.,-0.207911690817759));
#34462=DIRECTION('',(0.978147600733806,0.,-0.207911690817759));
#34463=DIRECTION('center_axis',(-0.207911690817759,0.,-0.978147600733806));
#34464=DIRECTION('ref_axis',(-0.978147600733806,0.,0.207911690817759));
#34465=DIRECTION('',(-0.978147600733806,0.,0.207911690817759));
#34466=DIRECTION('center_axis',(0.,1.,0.));
#34467=DIRECTION('ref_axis',(-0.207911690817759,0.,-0.978147600733806));
#34468=DIRECTION('center_axis',(0.,-1.,0.));
#34469=DIRECTION('ref_axis',(-1.22464679914735E-16,0.,1.));
#34470=DIRECTION('center_axis',(-1.22464679914735E-16,0.,1.));
#34471=DIRECTION('ref_axis',(1.,0.,1.22464679914735E-16));
#34472=DIRECTION('',(1.,0.,1.22464679914735E-16));
#34473=DIRECTION('center_axis',(0.,1.,0.));
#34474=DIRECTION('ref_axis',(1.22464679914735E-16,0.,-1.));
#34475=DIRECTION('center_axis',(0.,-1.,0.));
#34476=DIRECTION('ref_axis',(-0.20791169081776,0.,0.978147600733805));
#34477=DIRECTION('center_axis',(0.978147600733806,0.,0.20791169081776));
#34478=DIRECTION('ref_axis',(0.20791169081776,0.,-0.978147600733805));
#34479=DIRECTION('',(0.,1.,0.));
#34480=DIRECTION('',(0.20791169081776,0.,-0.978147600733805));
#34481=DIRECTION('',(0.,1.,0.));
#34482=DIRECTION('center_axis',(-0.20791169081776,0.,0.978147600733806));
#34483=DIRECTION('ref_axis',(0.978147600733805,0.,0.20791169081776));
#34484=DIRECTION('',(0.978147600733805,0.,0.20791169081776));
#34485=DIRECTION('center_axis',(0.20791169081776,0.,-0.978147600733806));
#34486=DIRECTION('ref_axis',(-0.978147600733805,0.,-0.20791169081776));
#34487=DIRECTION('',(-0.978147600733805,0.,-0.20791169081776));
#34488=DIRECTION('center_axis',(0.,1.,0.));
#34489=DIRECTION('ref_axis',(0.20791169081776,0.,-0.978147600733805));
#34490=DIRECTION('center_axis',(0.,-1.,0.));
#34491=DIRECTION('ref_axis',(-0.4067366430758,0.,0.913545457642601));
#34492=DIRECTION('center_axis',(-0.4067366430758,0.,0.913545457642601));
#34493=DIRECTION('ref_axis',(0.913545457642601,0.,0.4067366430758));
#34494=DIRECTION('',(0.913545457642601,0.,0.4067366430758));
#34495=DIRECTION('center_axis',(0.,1.,0.));
#34496=DIRECTION('ref_axis',(0.4067366430758,0.,-0.913545457642601));
#34497=DIRECTION('center_axis',(0.,-1.,0.));
#34498=DIRECTION('ref_axis',(-0.587785252292473,0.,0.809016994374947));
#34499=DIRECTION('center_axis',(0.809016994374947,0.,0.587785252292473));
#34500=DIRECTION('ref_axis',(0.587785252292473,0.,-0.809016994374947));
#34501=DIRECTION('',(0.,1.,0.));
#34502=DIRECTION('',(0.587785252292473,0.,-0.809016994374947));
#34503=DIRECTION('',(0.,1.,0.));
#34504=DIRECTION('center_axis',(-0.587785252292473,0.,0.809016994374947));
#34505=DIRECTION('ref_axis',(0.809016994374947,0.,0.587785252292473));
#34506=DIRECTION('',(0.809016994374947,0.,0.587785252292473));
#34507=DIRECTION('center_axis',(0.587785252292473,0.,-0.809016994374947));
#34508=DIRECTION('ref_axis',(-0.809016994374947,0.,-0.587785252292473));
#34509=DIRECTION('',(-0.809016994374947,0.,-0.587785252292473));
#34510=DIRECTION('center_axis',(0.,1.,0.));
#34511=DIRECTION('ref_axis',(0.587785252292473,0.,-0.809016994374947));
#34512=DIRECTION('center_axis',(0.,-1.,0.));
#34513=DIRECTION('ref_axis',(-0.743144825477394,0.,0.669130606358858));
#34514=DIRECTION('center_axis',(-0.743144825477394,0.,0.669130606358858));
#34515=DIRECTION('ref_axis',(0.669130606358858,0.,0.743144825477394));
#34516=DIRECTION('',(0.669130606358858,0.,0.743144825477394));
#34517=DIRECTION('center_axis',(0.,1.,0.));
#34518=DIRECTION('ref_axis',(0.743144825477394,0.,-0.669130606358858));
#34519=DIRECTION('center_axis',(-0.866025403784439,0.,0.5));
#34520=DIRECTION('ref_axis',(-0.5,0.,-0.866025403784439));
#34521=DIRECTION('',(-0.5,0.,-0.866025403784439));
#34522=DIRECTION('center_axis',(0.,-1.,0.));
#34523=DIRECTION('ref_axis',(-0.866025403784439,0.,0.5));
#34524=DIRECTION('center_axis',(0.5,0.,0.866025403784439));
#34525=DIRECTION('ref_axis',(0.866025403784439,0.,-0.5));
#34526=DIRECTION('',(0.,1.,0.));
#34527=DIRECTION('',(0.866025403784439,0.,-0.5));
#34528=DIRECTION('',(0.,1.,0.));
#34529=DIRECTION('center_axis',(-0.866025403784439,0.,0.5));
#34530=DIRECTION('ref_axis',(0.5,0.,0.866025403784439));
#34531=DIRECTION('',(0.5,0.,0.866025403784439));
#34532=DIRECTION('center_axis',(0.866025403784439,0.,-0.5));
#34533=DIRECTION('ref_axis',(-0.5,0.,-0.866025403784439));
#34534=DIRECTION('',(-0.5,0.,-0.866025403784439));
#34535=DIRECTION('center_axis',(0.,1.,0.));
#34536=DIRECTION('ref_axis',(0.866025403784439,0.,-0.5));
#34537=DIRECTION('center_axis',(0.,-1.,0.));
#34538=DIRECTION('ref_axis',(-0.951056516295154,0.,0.309016994374947));
#34539=DIRECTION('center_axis',(-0.951056516295154,0.,0.309016994374947));
#34540=DIRECTION('ref_axis',(0.309016994374947,0.,0.951056516295154));
#34541=DIRECTION('',(0.309016994374947,0.,0.951056516295154));
#34542=DIRECTION('center_axis',(0.,1.,0.));
#34543=DIRECTION('ref_axis',(0.951056516295154,0.,-0.309016994374947));
#34544=DIRECTION('center_axis',(0.,-1.,0.));
#34545=DIRECTION('ref_axis',(-0.994521895368273,0.,0.104528463267653));
#34546=DIRECTION('center_axis',(0.104528463267653,0.,0.994521895368273));
#34547=DIRECTION('ref_axis',(0.994521895368273,0.,-0.104528463267653));
#34548=DIRECTION('',(0.,1.,0.));
#34549=DIRECTION('',(0.994521895368273,0.,-0.104528463267653));
#34550=DIRECTION('',(0.,1.,0.));
#34551=DIRECTION('center_axis',(-0.994521895368273,0.,0.104528463267653));
#34552=DIRECTION('ref_axis',(0.104528463267653,0.,0.994521895368273));
#34553=DIRECTION('',(0.104528463267653,0.,0.994521895368273));
#34554=DIRECTION('center_axis',(0.994521895368273,0.,-0.104528463267653));
#34555=DIRECTION('ref_axis',(-0.104528463267653,0.,-0.994521895368273));
#34556=DIRECTION('',(-0.104528463267653,0.,-0.994521895368273));
#34557=DIRECTION('center_axis',(0.,1.,0.));
#34558=DIRECTION('ref_axis',(0.994521895368273,0.,-0.104528463267653));
#34559=DIRECTION('center_axis',(0.,-1.,0.));
#34560=DIRECTION('ref_axis',(-0.994521895368273,0.,-0.104528463267654));
#34561=DIRECTION('center_axis',(-0.104528463267654,0.,0.994521895368273));
#34562=DIRECTION('ref_axis',(0.994521895368273,0.,0.104528463267654));
#34563=DIRECTION('',(0.,1.,0.));
#34564=DIRECTION('',(0.994521895368273,0.,0.104528463267654));
#34565=DIRECTION('',(0.,1.,0.));
#34566=DIRECTION('center_axis',(-0.994521895368273,0.,-0.104528463267654));
#34567=DIRECTION('ref_axis',(-0.104528463267654,0.,0.994521895368273));
#34568=DIRECTION('',(-0.104528463267654,0.,0.994521895368273));
#34569=DIRECTION('center_axis',(0.994521895368273,0.,0.104528463267654));
#34570=DIRECTION('ref_axis',(0.104528463267654,0.,-0.994521895368273));
#34571=DIRECTION('',(0.104528463267654,0.,-0.994521895368273));
#34572=DIRECTION('center_axis',(0.,1.,0.));
#34573=DIRECTION('ref_axis',(0.994521895368273,0.,0.104528463267654));
#34574=DIRECTION('center_axis',(0.,-1.,0.));
#34575=DIRECTION('ref_axis',(-0.951056516295154,0.,-0.309016994374948));
#34576=DIRECTION('',(-0.309016994374948,0.,0.951056516295154));
#34577=DIRECTION('center_axis',(0.951056516295154,0.,0.309016994374948));
#34578=DIRECTION('ref_axis',(-0.309016994374948,0.,0.951056516295154));
#34579=DIRECTION('center_axis',(-0.951056516295154,0.,-0.309016994374948));
#34580=DIRECTION('ref_axis',(-0.309016994374948,0.,0.951056516295154));
#34581=DIRECTION('',(-0.309016994374948,0.,0.951056516295154));
#34582=DIRECTION('center_axis',(0.,1.,0.));
#34583=DIRECTION('ref_axis',(0.951056516295154,0.,0.309016994374948));
#34584=DIRECTION('center_axis',(-0.866025403784439,0.,-0.5));
#34585=DIRECTION('ref_axis',(0.5,0.,-0.866025403784439));
#34586=DIRECTION('',(0.,-1.,0.));
#34587=DIRECTION('',(0.5,0.,-0.866025403784439));
#34588=DIRECTION('center_axis',(0.,-1.,0.));
#34589=DIRECTION('ref_axis',(-0.866025403784439,0.,-0.5));
#34590=DIRECTION('',(-0.866025403784439,0.,-0.5));
#34591=DIRECTION('',(-0.5,0.,0.866025403784439));
#34592=DIRECTION('center_axis',(-0.5,0.,0.866025403784439));
#34593=DIRECTION('ref_axis',(-0.866025403784439,0.,-0.5));
#34594=DIRECTION('',(0.,-1.,0.));
#34595=DIRECTION('center_axis',(0.866025403784439,0.,0.5));
#34596=DIRECTION('ref_axis',(-0.5,0.,0.866025403784439));
#34597=DIRECTION('center_axis',(-0.5,0.,0.866025403784439));
#34598=DIRECTION('ref_axis',(0.866025403784439,0.,0.5));
#34599=DIRECTION('',(0.,1.,0.));
#34600=DIRECTION('',(0.866025403784439,0.,0.5));
#34601=DIRECTION('',(0.,1.,0.));
#34602=DIRECTION('center_axis',(-0.866025403784439,0.,-0.5));
#34603=DIRECTION('ref_axis',(-0.5,0.,0.866025403784439));
#34604=DIRECTION('',(-0.5,0.,0.866025403784439));
#34605=DIRECTION('center_axis',(0.866025403784439,0.,0.5));
#34606=DIRECTION('ref_axis',(0.5,0.,-0.866025403784439));
#34607=DIRECTION('',(0.5,0.,-0.866025403784439));
#34608=DIRECTION('center_axis',(0.,1.,0.));
#34609=DIRECTION('ref_axis',(0.866025403784439,0.,0.5));
#34610=DIRECTION('center_axis',(-0.743144825477394,0.,-0.669130606358858));
#34611=DIRECTION('ref_axis',(0.669130606358858,0.,-0.743144825477394));
#34612=DIRECTION('',(0.,-1.,0.));
#34613=DIRECTION('',(0.669130606358858,0.,-0.743144825477394));
#34614=DIRECTION('center_axis',(0.,-1.,0.));
#34615=DIRECTION('ref_axis',(-0.743144825477394,0.,-0.669130606358858));
#34616=DIRECTION('',(-0.743144825477394,0.,-0.669130606358858));
#34617=DIRECTION('',(-0.669130606358858,0.,0.743144825477394));
#34618=DIRECTION('center_axis',(-0.669130606358858,0.,0.743144825477394));
#34619=DIRECTION('ref_axis',(-0.743144825477394,0.,-0.669130606358858));
#34620=DIRECTION('',(0.,-1.,0.));
#34621=DIRECTION('center_axis',(0.743144825477394,0.,0.669130606358858));
#34622=DIRECTION('ref_axis',(-0.669130606358858,0.,0.743144825477394));
#34623=DIRECTION('center_axis',(-0.743144825477394,0.,-0.669130606358858));
#34624=DIRECTION('ref_axis',(-0.669130606358858,0.,0.743144825477394));
#34625=DIRECTION('',(-0.669130606358858,0.,0.743144825477394));
#34626=DIRECTION('center_axis',(0.,1.,0.));
#34627=DIRECTION('ref_axis',(0.743144825477394,0.,0.669130606358858));
#34628=DIRECTION('center_axis',(-0.587785252292473,0.,-0.809016994374947));
#34629=DIRECTION('ref_axis',(0.809016994374947,0.,-0.587785252292473));
#34630=DIRECTION('',(0.,-1.,0.));
#34631=DIRECTION('',(0.809016994374947,0.,-0.587785252292473));
#34632=DIRECTION('center_axis',(0.,-1.,0.));
#34633=DIRECTION('ref_axis',(-0.587785252292473,0.,-0.809016994374947));
#34634=DIRECTION('',(-0.587785252292473,0.,-0.809016994374947));
#34635=DIRECTION('',(-0.809016994374947,0.,0.587785252292473));
#34636=DIRECTION('center_axis',(-0.809016994374947,0.,0.587785252292473));
#34637=DIRECTION('ref_axis',(-0.587785252292473,0.,-0.809016994374947));
#34638=DIRECTION('',(0.,-1.,0.));
#34639=DIRECTION('center_axis',(0.587785252292473,0.,0.809016994374947));
#34640=DIRECTION('ref_axis',(-0.809016994374947,0.,0.587785252292473));
#34641=DIRECTION('center_axis',(-0.809016994374947,0.,0.587785252292473));
#34642=DIRECTION('ref_axis',(0.587785252292473,0.,0.809016994374947));
#34643=DIRECTION('',(0.,1.,0.));
#34644=DIRECTION('',(0.587785252292473,0.,0.809016994374947));
#34645=DIRECTION('',(0.,1.,0.));
#34646=DIRECTION('center_axis',(-0.587785252292473,0.,-0.809016994374947));
#34647=DIRECTION('ref_axis',(-0.809016994374947,0.,0.587785252292473));
#34648=DIRECTION('',(-0.809016994374947,0.,0.587785252292473));
#34649=DIRECTION('center_axis',(0.587785252292473,0.,0.809016994374947));
#34650=DIRECTION('ref_axis',(0.809016994374947,0.,-0.587785252292473));
#34651=DIRECTION('',(0.809016994374947,0.,-0.587785252292473));
#34652=DIRECTION('center_axis',(0.,1.,0.));
#34653=DIRECTION('ref_axis',(0.587785252292473,0.,0.809016994374947));
#34654=DIRECTION('center_axis',(-0.4067366430758,0.,-0.913545457642601));
#34655=DIRECTION('ref_axis',(0.913545457642601,0.,-0.4067366430758));
#34656=DIRECTION('',(0.,-1.,0.));
#34657=DIRECTION('',(0.913545457642601,0.,-0.4067366430758));
#34658=DIRECTION('center_axis',(0.,-1.,0.));
#34659=DIRECTION('ref_axis',(-0.4067366430758,0.,-0.913545457642601));
#34660=DIRECTION('',(-0.4067366430758,0.,-0.913545457642601));
#34661=DIRECTION('',(-0.913545457642601,0.,0.4067366430758));
#34662=DIRECTION('center_axis',(-0.913545457642601,0.,0.4067366430758));
#34663=DIRECTION('ref_axis',(-0.4067366430758,0.,-0.913545457642601));
#34664=DIRECTION('',(0.,-1.,0.));
#34665=DIRECTION('center_axis',(0.4067366430758,0.,0.913545457642601));
#34666=DIRECTION('ref_axis',(-0.913545457642601,0.,0.4067366430758));
#34667=DIRECTION('center_axis',(-0.4067366430758,0.,-0.913545457642601));
#34668=DIRECTION('ref_axis',(-0.913545457642601,0.,0.4067366430758));
#34669=DIRECTION('',(-0.913545457642601,0.,0.4067366430758));
#34670=DIRECTION('center_axis',(0.,1.,0.));
#34671=DIRECTION('ref_axis',(0.4067366430758,0.,0.913545457642601));
#34672=DIRECTION('center_axis',(-0.207911690817759,0.,-0.978147600733806));
#34673=DIRECTION('ref_axis',(0.978147600733806,0.,-0.207911690817759));
#34674=DIRECTION('',(0.,-1.,0.));
#34675=DIRECTION('',(0.978147600733806,0.,-0.207911690817759));
#34676=DIRECTION('center_axis',(0.,-1.,0.));
#34677=DIRECTION('ref_axis',(-0.207911690817759,0.,-0.978147600733806));
#34678=DIRECTION('',(-0.207911690817759,0.,-0.978147600733806));
#34679=DIRECTION('',(-0.978147600733806,0.,0.207911690817759));
#34680=DIRECTION('center_axis',(-0.978147600733806,0.,0.207911690817759));
#34681=DIRECTION('ref_axis',(-0.207911690817759,0.,-0.978147600733806));
#34682=DIRECTION('',(0.,-1.,0.));
#34683=DIRECTION('center_axis',(0.207911690817759,0.,0.978147600733806));
#34684=DIRECTION('ref_axis',(-0.978147600733806,0.,0.207911690817759));
#34685=DIRECTION('center_axis',(-0.978147600733806,0.,0.207911690817759));
#34686=DIRECTION('ref_axis',(0.207911690817759,0.,0.978147600733806));
#34687=DIRECTION('',(0.,1.,0.));
#34688=DIRECTION('',(0.207911690817759,0.,0.978147600733806));
#34689=DIRECTION('',(0.,1.,0.));
#34690=DIRECTION('center_axis',(-0.207911690817759,0.,-0.978147600733806));
#34691=DIRECTION('ref_axis',(-0.978147600733806,0.,0.207911690817759));
#34692=DIRECTION('',(-0.978147600733806,0.,0.207911690817759));
#34693=DIRECTION('center_axis',(0.207911690817759,0.,0.978147600733806));
#34694=DIRECTION('ref_axis',(0.978147600733806,0.,-0.207911690817759));
#34695=DIRECTION('',(0.978147600733806,0.,-0.207911690817759));
#34696=DIRECTION('center_axis',(0.,1.,0.));
#34697=DIRECTION('ref_axis',(0.207911690817759,0.,0.978147600733806));
#34698=DIRECTION('center_axis',(0.,0.,-1.));
#34699=DIRECTION('ref_axis',(1.,0.,0.));
#34700=DIRECTION('',(0.,-1.,0.));
#34701=DIRECTION('',(1.,0.,0.));
#34702=DIRECTION('center_axis',(0.,-1.,0.));
#34703=DIRECTION('ref_axis',(0.,0.,-1.));
#34704=DIRECTION('',(0.,0.,-1.));
#34705=DIRECTION('',(-1.,0.,0.));
#34706=DIRECTION('center_axis',(-1.,0.,0.));
#34707=DIRECTION('ref_axis',(0.,0.,-1.));
#34708=DIRECTION('',(0.,-1.,0.));
#34709=DIRECTION('center_axis',(0.,0.,1.));
#34710=DIRECTION('ref_axis',(-1.,0.,0.));
#34711=DIRECTION('center_axis',(0.,1.,0.));
#34712=DIRECTION('ref_axis',(0.,0.,1.));
#34713=DIRECTION('',(1.,0.,0.));
#34714=DIRECTION('',(0.,0.,1.));
#34715=DIRECTION('',(-1.,0.,0.));
#34716=DIRECTION('center_axis',(0.,0.,-1.));
#34717=DIRECTION('ref_axis',(-1.,0.,0.));
#34718=DIRECTION('',(0.,1.,0.));
#34719=DIRECTION('center_axis',(-1.,0.,0.));
#34720=DIRECTION('ref_axis',(0.,0.,1.));
#34721=DIRECTION('',(0.,1.,0.));
#34722=DIRECTION('center_axis',(0.,0.,1.));
#34723=DIRECTION('ref_axis',(1.,0.,0.));
#34724=DIRECTION('center_axis',(0.,1.,0.));
#34725=DIRECTION('ref_axis',(-1.22464679914735E-16,0.,-1.));
#34726=DIRECTION('axis',(0.,0.,1.));
#34727=DIRECTION('refdir',(1.,0.,0.));
#34728=DIRECTION('center_axis',(-1.,0.,0.));
#34729=DIRECTION('ref_axis',(0.,1.,0.));
#34730=DIRECTION('center_axis',(-1.,0.,0.));
#34731=DIRECTION('ref_axis',(0.,1.,0.));
#34732=DIRECTION('',(0.,0.,-1.));
#34733=DIRECTION('',(0.,1.,0.));
#34734=DIRECTION('',(0.,0.,-1.));
#34735=DIRECTION('center_axis',(0.,1.,0.));
#34736=DIRECTION('ref_axis',(1.,0.,0.));
#34737=DIRECTION('',(1.,0.,0.));
#34738=DIRECTION('',(1.,0.,0.));
#34739=DIRECTION('',(0.,0.,-1.));
#34740=DIRECTION('center_axis',(0.,-1.,0.));
#34741=DIRECTION('ref_axis',(-1.,0.,0.));
#34742=DIRECTION('',(-1.,0.,0.));
#34743=DIRECTION('',(0.,0.,-1.));
#34744=DIRECTION('',(-1.,0.,0.));
#34745=DIRECTION('center_axis',(1.,0.,0.));
#34746=DIRECTION('ref_axis',(0.,-1.,0.));
#34747=DIRECTION('center_axis',(1.,0.,0.));
#34748=DIRECTION('ref_axis',(0.,1.,0.));
#34749=DIRECTION('',(0.,-1.,0.));
#34750=DIRECTION('center_axis',(0.,0.,-1.));
#34751=DIRECTION('ref_axis',(-1.,0.,0.));
#34752=DIRECTION('center_axis',(0.,1.,0.));
#34753=DIRECTION('ref_axis',(1.,0.,0.));
#34754=DIRECTION('',(0.,1.,0.));
#34755=DIRECTION('center_axis',(-1.,0.,0.));
#34756=DIRECTION('ref_axis',(0.,0.,1.));
#34757=DIRECTION('center_axis',(1.,0.,0.));
#34758=DIRECTION('ref_axis',(0.,0.,-1.));
#34759=DIRECTION('center_axis',(1.,0.,0.));
#34760=DIRECTION('ref_axis',(0.,1.,0.));
#34761=DIRECTION('center_axis',(1.,0.,0.));
#34762=DIRECTION('ref_axis',(0.,0.,-1.));
#34763=DIRECTION('',(-0.707106781186548,0.707106781186548,8.65956056235494E-17));
#34764=DIRECTION('center_axis',(1.,0.,0.));
#34765=DIRECTION('ref_axis',(0.,1.,0.));
#34766=DIRECTION('center_axis',(1.,0.,0.));
#34767=DIRECTION('ref_axis',(0.,0.,-1.));
#34768=DIRECTION('',(-1.,0.,0.));
#34769=DIRECTION('',(-1.,0.,0.));
#34770=DIRECTION('center_axis',(1.,0.,0.));
#34771=DIRECTION('ref_axis',(0.,1.,0.));
#34772=DIRECTION('center_axis',(1.,0.,0.));
#34773=DIRECTION('ref_axis',(0.,0.,-1.));
#34774=DIRECTION('',(-0.196116135138183,0.98058067569092,1.20086498579063E-16));
#34775=DIRECTION('center_axis',(1.,0.,0.));
#34776=DIRECTION('ref_axis',(0.,1.,0.));
#34777=DIRECTION('center_axis',(1.,0.,0.));
#34778=DIRECTION('ref_axis',(0.,0.,-1.));
#34779=DIRECTION('',(-1.,0.,0.));
#34780=DIRECTION('center_axis',(-1.,0.,0.));
#34781=DIRECTION('ref_axis',(0.,0.,1.));
#34782=DIRECTION('center_axis',(1.,0.,0.));
#34783=DIRECTION('ref_axis',(0.,0.,-1.));
#34784=DIRECTION('center_axis',(1.,0.,0.));
#34785=DIRECTION('ref_axis',(0.,1.,0.));
#34786=DIRECTION('center_axis',(1.,0.,0.));
#34787=DIRECTION('ref_axis',(0.,0.,-1.));
#34788=DIRECTION('',(-1.,0.,0.));
#34789=DIRECTION('center_axis',(1.,0.,0.));
#34790=DIRECTION('ref_axis',(0.,0.,-1.));
#34791=DIRECTION('center_axis',(1.,0.,0.));
#34792=DIRECTION('ref_axis',(0.,0.,-1.));
#34793=DIRECTION('center_axis',(1.,0.,0.));
#34794=DIRECTION('ref_axis',(0.,1.,0.));
#34795=DIRECTION('center_axis',(1.,0.,0.));
#34796=DIRECTION('ref_axis',(0.,0.,-1.));
#34797=DIRECTION('',(-1.,0.,0.));
#34798=DIRECTION('center_axis',(1.,0.,0.));
#34799=DIRECTION('ref_axis',(0.,0.,-1.));
#34800=DIRECTION('center_axis',(1.,0.,0.));
#34801=DIRECTION('ref_axis',(0.,0.,-1.));
#34802=DIRECTION('center_axis',(1.,0.,0.));
#34803=DIRECTION('ref_axis',(0.,1.,0.));
#34804=DIRECTION('center_axis',(1.,0.,0.));
#34805=DIRECTION('ref_axis',(0.,0.,-1.));
#34806=DIRECTION('',(-1.,0.,0.));
#34807=DIRECTION('center_axis',(-1.,0.,0.));
#34808=DIRECTION('ref_axis',(0.,0.,1.));
#34809=DIRECTION('center_axis',(1.,0.,0.));
#34810=DIRECTION('ref_axis',(0.,0.,-1.));
#34811=DIRECTION('center_axis',(1.,0.,0.));
#34812=DIRECTION('ref_axis',(0.,1.,0.));
#34813=DIRECTION('center_axis',(1.,0.,0.));
#34814=DIRECTION('ref_axis',(0.,0.,-1.));
#34815=DIRECTION('',(-1.,0.,0.));
#34816=DIRECTION('center_axis',(1.,0.,0.));
#34817=DIRECTION('ref_axis',(0.,0.,-1.));
#34818=DIRECTION('center_axis',(1.,0.,0.));
#34819=DIRECTION('ref_axis',(0.,0.,-1.));
#34820=DIRECTION('center_axis',(1.,0.,0.));
#34821=DIRECTION('ref_axis',(0.,1.,0.));
#34822=DIRECTION('center_axis',(1.,0.,0.));
#34823=DIRECTION('ref_axis',(0.,0.,-1.));
#34824=DIRECTION('',(-1.,0.,0.));
#34825=DIRECTION('center_axis',(-1.,0.,0.));
#34826=DIRECTION('ref_axis',(0.,1.,0.));
#34827=DIRECTION('center_axis',(1.,0.,0.));
#34828=DIRECTION('ref_axis',(0.,0.,-1.));
#34829=DIRECTION('',(-0.707106781186552,-0.707106781186543,-8.65956056235487E-17));
#34830=DIRECTION('center_axis',(1.,0.,0.));
#34831=DIRECTION('ref_axis',(0.,0.,-1.));
#34832=DIRECTION('axis',(0.,0.,1.));
#34833=DIRECTION('refdir',(1.,0.,0.));
#34834=DIRECTION('center_axis',(1.,0.,0.));
#34835=DIRECTION('ref_axis',(0.,1.,0.));
#34836=DIRECTION('center_axis',(1.,0.,0.));
#34837=DIRECTION('ref_axis',(0.,0.,-1.));
#34838=DIRECTION('',(-0.961523947640823,0.274721127897378,3.36436349937675E-17));
#34839=DIRECTION('center_axis',(1.,0.,0.));
#34840=DIRECTION('ref_axis',(0.,0.,-1.));
#34841=DIRECTION('center_axis',(-1.,0.,0.));
#34842=DIRECTION('ref_axis',(0.,0.,1.));
#34843=DIRECTION('center_axis',(1.,0.,0.));
#34844=DIRECTION('ref_axis',(0.,0.,-1.));
#34845=DIRECTION('center_axis',(-1.,0.,0.));
#34846=DIRECTION('ref_axis',(0.,1.,0.));
#34847=DIRECTION('',(-0.961523947640823,-0.274721127897378,-3.36436349937675E-17));
#34848=DIRECTION('center_axis',(1.,0.,0.));
#34849=DIRECTION('ref_axis',(0.,0.,-1.));
#34850=DIRECTION('center_axis',(-1.,0.,0.));
#34851=DIRECTION('ref_axis',(0.,0.,1.));
#34852=DIRECTION('center_axis',(1.,0.,0.));
#34853=DIRECTION('ref_axis',(0.,0.,-1.));
#34854=DIRECTION('center_axis',(1.,0.,0.));
#34855=DIRECTION('ref_axis',(0.,1.,0.));
#34856=DIRECTION('center_axis',(1.,0.,0.));
#34857=DIRECTION('ref_axis',(0.,0.,-1.));
#34858=DIRECTION('',(-0.707106781186548,0.707106781186547,8.65956056235493E-17));
#34859=DIRECTION('center_axis',(1.,0.,0.));
#34860=DIRECTION('ref_axis',(0.,1.,0.));
#34861=DIRECTION('center_axis',(1.,0.,0.));
#34862=DIRECTION('ref_axis',(0.,0.,-1.));
#34863=DIRECTION('',(-1.,0.,0.));
#34864=DIRECTION('center_axis',(-1.,0.,0.));
#34865=DIRECTION('ref_axis',(0.,1.,0.));
#34866=DIRECTION('center_axis',(1.,0.,0.));
#34867=DIRECTION('ref_axis',(0.,0.,-1.));
#34868=DIRECTION('',(-0.707106781186547,-0.707106781186547,-8.65956056235493E-17));
#34869=DIRECTION('center_axis',(1.,0.,0.));
#34870=DIRECTION('ref_axis',(0.,0.,-1.));
#34871=DIRECTION('center_axis',(1.,0.,0.));
#34872=DIRECTION('ref_axis',(0.,0.,-1.));
#34873=DIRECTION('center_axis',(1.,0.,0.));
#34874=DIRECTION('ref_axis',(0.,1.,0.));
#34875=DIRECTION('',(-0.961523947640823,0.274721127897379,3.36436349937676E-17));
#34876=DIRECTION('center_axis',(1.,0.,0.));
#34877=DIRECTION('ref_axis',(0.,0.,-1.));
#34878=DIRECTION('center_axis',(1.,0.,0.));
#34879=DIRECTION('ref_axis',(0.,0.,-1.));
#34880=DIRECTION('center_axis',(1.,0.,0.));
#34881=DIRECTION('ref_axis',(0.,0.,-1.));
#34882=DIRECTION('center_axis',(-1.,0.,0.));
#34883=DIRECTION('ref_axis',(0.,1.,0.));
#34884=DIRECTION('center_axis',(1.,0.,0.));
#34885=DIRECTION('ref_axis',(0.,0.,-1.));
#34886=DIRECTION('',(-0.961523947640823,-0.274721127897379,-3.36436349937676E-17));
#34887=DIRECTION('center_axis',(1.,0.,0.));
#34888=DIRECTION('ref_axis',(0.,0.,-1.));
#34889=DIRECTION('center_axis',(1.,0.,0.));
#34890=DIRECTION('ref_axis',(0.,0.,-1.));
#34891=DIRECTION('center_axis',(1.,0.,0.));
#34892=DIRECTION('ref_axis',(0.,1.,0.));
#34893=DIRECTION('',(-0.707106781186547,0.707106781186547,8.65956056235493E-17));
#34894=DIRECTION('center_axis',(1.,0.,0.));
#34895=DIRECTION('ref_axis',(0.,0.,-1.));
#34896=DIRECTION('center_axis',(1.,0.,0.));
#34897=DIRECTION('ref_axis',(0.,1.,0.));
#34898=DIRECTION('',(-1.,0.,0.));
#34899=DIRECTION('center_axis',(1.,0.,0.));
#34900=DIRECTION('ref_axis',(0.,0.,-1.));
#34901=DIRECTION('center_axis',(-1.,0.,0.));
#34902=DIRECTION('ref_axis',(0.,1.,0.));
#34903=DIRECTION('',(-0.707106781186548,-0.707106781186547,-8.65956056235493E-17));
#34904=DIRECTION('center_axis',(1.,0.,0.));
#34905=DIRECTION('ref_axis',(0.,0.,-1.));
#34906=DIRECTION('center_axis',(-1.,0.,0.));
#34907=DIRECTION('ref_axis',(0.,0.,1.));
#34908=DIRECTION('axis',(0.,0.,1.));
#34909=DIRECTION('refdir',(1.,0.,0.));
#34910=DIRECTION('center_axis',(-1.,0.,0.));
#34911=DIRECTION('ref_axis',(0.,-1.,0.));
#34912=DIRECTION('center_axis',(-1.,0.,0.));
#34913=DIRECTION('ref_axis',(0.,-1.,0.));
#34914=DIRECTION('',(-0.707106781186547,0.707106781186547,8.65956056235493E-17));
#34915=DIRECTION('center_axis',(1.,0.,0.));
#34916=DIRECTION('ref_axis',(0.,-1.,0.));
#34917=DIRECTION('center_axis',(1.,0.,0.));
#34918=DIRECTION('ref_axis',(0.,-1.,0.));
#34919=DIRECTION('center_axis',(1.,0.,0.));
#34920=DIRECTION('ref_axis',(0.,1.,0.));
#34921=DIRECTION('',(-1.,0.,0.));
#34922=DIRECTION('center_axis',(1.,0.,0.));
#34923=DIRECTION('ref_axis',(0.,0.,-1.));
#34924=DIRECTION('center_axis',(1.,0.,0.));
#34925=DIRECTION('ref_axis',(0.,0.,-1.));
#34926=DIRECTION('center_axis',(1.,0.,0.));
#34927=DIRECTION('ref_axis',(0.,0.,-1.));
#34928=DIRECTION('center_axis',(1.,0.,0.));
#34929=DIRECTION('ref_axis',(0.,1.,0.));
#34930=DIRECTION('center_axis',(1.,0.,0.));
#34931=DIRECTION('ref_axis',(0.,0.,-1.));
#34932=DIRECTION('',(-1.,0.,0.));
#34933=DIRECTION('center_axis',(1.,0.,0.));
#34934=DIRECTION('ref_axis',(0.,0.,-1.));
#34935=DIRECTION('center_axis',(-1.,0.,0.));
#34936=DIRECTION('ref_axis',(0.,0.,1.));
#34937=DIRECTION('center_axis',(1.,0.,0.));
#34938=DIRECTION('ref_axis',(0.,0.,-1.));
#34939=DIRECTION('center_axis',(1.,0.,0.));
#34940=DIRECTION('ref_axis',(0.,1.,0.));
#34941=DIRECTION('',(-0.707106781186547,0.707106781186548,8.65956056235494E-17));
#34942=DIRECTION('center_axis',(1.,0.,0.));
#34943=DIRECTION('ref_axis',(0.,1.,0.));
#34944=DIRECTION('center_axis',(1.,0.,0.));
#34945=DIRECTION('ref_axis',(0.,0.,-1.));
#34946=DIRECTION('',(-1.,0.,0.));
#34947=DIRECTION('center_axis',(1.,0.,0.));
#34948=DIRECTION('ref_axis',(0.,0.,-1.));
#34949=DIRECTION('center_axis',(1.,0.,0.));
#34950=DIRECTION('ref_axis',(0.,0.,-1.));
#34951=DIRECTION('center_axis',(1.,0.,0.));
#34952=DIRECTION('ref_axis',(0.,1.,0.));
#34953=DIRECTION('',(-1.,0.,0.));
#34954=DIRECTION('center_axis',(1.,0.,0.));
#34955=DIRECTION('ref_axis',(0.,0.,-1.));
#34956=DIRECTION('center_axis',(1.,0.,0.));
#34957=DIRECTION('ref_axis',(0.,0.,-1.));
#34958=DIRECTION('axis',(0.,0.,1.));
#34959=DIRECTION('refdir',(1.,0.,0.));
#34960=DIRECTION('center_axis',(1.,0.,0.));
#34961=DIRECTION('ref_axis',(0.,1.,0.));
#34962=DIRECTION('center_axis',(1.,0.,0.));
#34963=DIRECTION('ref_axis',(0.,0.,-1.));
#34964=DIRECTION('',(-1.,0.,0.));
#34965=DIRECTION('center_axis',(1.,0.,0.));
#34966=DIRECTION('ref_axis',(0.,0.,-1.));
#34967=DIRECTION('center_axis',(-1.,0.,0.));
#34968=DIRECTION('ref_axis',(0.,0.,1.));
#34969=DIRECTION('center_axis',(1.,0.,0.));
#34970=DIRECTION('ref_axis',(0.,0.,-1.));
#34971=DIRECTION('center_axis',(1.,0.,0.));
#34972=DIRECTION('ref_axis',(0.,1.,0.));
#34973=DIRECTION('center_axis',(1.,0.,0.));
#34974=DIRECTION('ref_axis',(0.,0.,-1.));
#34975=DIRECTION('',(-0.707106781186546,0.707106781186549,8.65956056235495E-17));
#34976=DIRECTION('center_axis',(1.,0.,0.));
#34977=DIRECTION('ref_axis',(0.,1.,0.));
#34978=DIRECTION('center_axis',(1.,0.,0.));
#34979=DIRECTION('ref_axis',(0.,0.,-1.));
#34980=DIRECTION('',(-1.,0.,0.));
#34981=DIRECTION('center_axis',(1.,0.,0.));
#34982=DIRECTION('ref_axis',(0.,0.,-1.));
#34983=DIRECTION('axis',(0.,0.,1.));
#34984=DIRECTION('refdir',(1.,0.,0.));
#34985=DIRECTION('center_axis',(-1.,0.,0.));
#34986=DIRECTION('ref_axis',(0.,0.,1.));
#34987=DIRECTION('center_axis',(1.,0.,0.));
#34988=DIRECTION('ref_axis',(0.,0.,-1.));
#34989=DIRECTION('center_axis',(1.,0.,0.));
#34990=DIRECTION('ref_axis',(0.,1.,0.));
#34991=DIRECTION('center_axis',(1.,0.,0.));
#34992=DIRECTION('ref_axis',(0.,0.,-1.));
#34993=DIRECTION('',(-0.707106781186548,0.707106781186547,8.65956056235493E-17));
#34994=DIRECTION('center_axis',(1.,0.,0.));
#34995=DIRECTION('ref_axis',(0.,1.,0.));
#34996=DIRECTION('center_axis',(1.,0.,0.));
#34997=DIRECTION('ref_axis',(0.,0.,-1.));
#34998=DIRECTION('',(-1.,0.,0.));
#34999=DIRECTION('center_axis',(-1.,0.,0.));
#35000=DIRECTION('ref_axis',(0.,1.,0.));
#35001=DIRECTION('center_axis',(1.,0.,0.));
#35002=DIRECTION('ref_axis',(0.,0.,-1.));
#35003=DIRECTION('',(-0.707106781186548,-0.707106781186547,-8.65956056235493E-17));
#35004=DIRECTION('center_axis',(1.,0.,0.));
#35005=DIRECTION('ref_axis',(0.,0.,-1.));
#35006=DIRECTION('axis',(0.,0.,1.));
#35007=DIRECTION('refdir',(1.,0.,0.));
#35008=DIRECTION('center_axis',(1.,0.,0.));
#35009=DIRECTION('ref_axis',(0.,1.,0.));
#35010=DIRECTION('center_axis',(1.,0.,0.));
#35011=DIRECTION('ref_axis',(0.,0.,-1.));
#35012=DIRECTION('',(-1.,0.,0.));
#35013=DIRECTION('center_axis',(1.,0.,0.));
#35014=DIRECTION('ref_axis',(0.,0.,-1.));
#35015=DIRECTION('center_axis',(-1.,0.,0.));
#35016=DIRECTION('ref_axis',(0.,0.,1.));
#35017=DIRECTION('center_axis',(1.,0.,0.));
#35018=DIRECTION('ref_axis',(0.,0.,-1.));
#35019=DIRECTION('center_axis',(1.,0.,0.));
#35020=DIRECTION('ref_axis',(0.,1.,0.));
#35021=DIRECTION('center_axis',(1.,0.,0.));
#35022=DIRECTION('ref_axis',(0.,0.,-1.));
#35023=DIRECTION('',(-1.,0.,0.));
#35024=DIRECTION('center_axis',(1.,0.,0.));
#35025=DIRECTION('ref_axis',(0.,0.,-1.));
#35026=DIRECTION('axis',(0.,0.,1.));
#35027=DIRECTION('refdir',(1.,0.,0.));
#35028=DIRECTION('center_axis',(1.,0.,0.));
#35029=DIRECTION('ref_axis',(0.,0.,-1.));
#35030=DIRECTION('center_axis',(0.,-1.,-1.22464679914735E-16));
#35031=DIRECTION('ref_axis',(0.,-1.22464679914735E-16,1.));
#35032=DIRECTION('center_axis',(-1.,0.,0.));
#35033=DIRECTION('ref_axis',(0.,0.,-1.));
#35034=DIRECTION('axis',(0.,0.,1.));
#35035=DIRECTION('refdir',(1.,0.,0.));
#35036=DIRECTION('center_axis',(0.707106781186548,-0.707106781186547,0.));
#35037=DIRECTION('ref_axis',(0.,0.,-1.));
#35038=DIRECTION('',(0.,0.,-1.));
#35039=DIRECTION('center_axis',(-0.707106781186548,0.707106781186547,0.));
#35040=DIRECTION('ref_axis',(-0.707106781186547,-0.707106781186548,6.56942451332124E-17));
#35041=DIRECTION('',(0.,0.,1.));
#35042=DIRECTION('center_axis',(-1.,0.,0.));
#35043=DIRECTION('ref_axis',(0.,0.1875,-0.982264602843857));
#35044=DIRECTION('center_axis',(-1.,0.,0.));
#35045=DIRECTION('ref_axis',(0.,0.1875,-0.982264602843857));
#35046=DIRECTION('center_axis',(1.,0.,0.));
#35047=DIRECTION('ref_axis',(0.,0.1875,-0.982264602843857));
#35048=DIRECTION('center_axis',(0.707106781186548,0.707106781186547,0.));
#35049=DIRECTION('ref_axis',(0.,0.,-1.));
#35050=DIRECTION('',(0.,0.,-1.));
#35051=DIRECTION('center_axis',(-0.707106781186548,-0.707106781186547,0.));
#35052=DIRECTION('ref_axis',(0.707106781186547,-0.707106781186548,6.56942451332124E-17));
#35053=DIRECTION('',(0.,0.,1.));
#35054=DIRECTION('center_axis',(1.,0.,0.));
#35055=DIRECTION('ref_axis',(0.,0.,-1.));
#35056=DIRECTION('center_axis',(-1.,0.,0.));
#35057=DIRECTION('ref_axis',(0.,-0.251046025104602,0.967975151168241));
#35058=DIRECTION('center_axis',(-0.707106781186548,-0.707106781186547,0.));
#35059=DIRECTION('ref_axis',(0.,0.,1.));
#35060=DIRECTION('',(0.,0.,-1.));
#35061=DIRECTION('center_axis',(0.707106781186548,0.707106781186547,0.));
#35062=DIRECTION('ref_axis',(0.707106781186547,-0.707106781186548,6.56942451332124E-17));
#35063=DIRECTION('',(0.,0.,1.));
#35064=DIRECTION('center_axis',(-0.707106781186548,0.707106781186547,0.));
#35065=DIRECTION('ref_axis',(0.,0.,1.));
#35066=DIRECTION('',(0.,0.,-1.));
#35067=DIRECTION('center_axis',(0.707106781186548,-0.707106781186547,0.));
#35068=DIRECTION('ref_axis',(-0.707106781186547,-0.707106781186548,6.56942451332124E-17));
#35069=DIRECTION('',(0.,0.,1.));
#35070=DIRECTION('center_axis',(1.,0.,0.));
#35071=DIRECTION('ref_axis',(0.,0.1875,-0.982264602843857));
#35072=DIRECTION('center_axis',(-1.,0.,0.));
#35073=DIRECTION('ref_axis',(0.,0.1875,-0.982264602843857));
#35074=DIRECTION('center_axis',(1.,0.,0.));
#35075=DIRECTION('ref_axis',(0.,0.1875,-0.982264602843857));
#35076=DIRECTION('center_axis',(1.,0.,0.));
#35077=DIRECTION('ref_axis',(0.,0.,-1.));
#35078=DIRECTION('center_axis',(1.,0.,0.));
#35079=DIRECTION('ref_axis',(0.,-0.251046025104602,0.967975151168241));
#35080=DIRECTION('center_axis',(0.,1.,0.));
#35081=DIRECTION('ref_axis',(0.,0.,1.));
#35082=DIRECTION('',(1.,0.,0.));
#35083=DIRECTION('',(1.,0.,0.));
#35084=DIRECTION('center_axis',(1.,0.,0.));
#35085=DIRECTION('ref_axis',(0.,-2.42861286636753E-16,-1.));
#35086=DIRECTION('',(1.,0.,0.));
#35087=DIRECTION('center_axis',(1.,0.,0.));
#35088=DIRECTION('ref_axis',(0.,9.29056924372516E-17,-1.));
#35089=DIRECTION('',(1.,0.,0.));
#35090=DIRECTION('center_axis',(0.,-1.,0.));
#35091=DIRECTION('ref_axis',(0.,0.,-1.));
#35092=DIRECTION('axis',(0.,0.,1.));
#35093=DIRECTION('refdir',(1.,0.,0.));
#35094=DIRECTION('center_axis',(0.553588677216092,-0.6352112172796,-0.53855945437835));
#35095=DIRECTION('ref_axis',(-0.697310151651834,0.,-0.716769525303145));
#35096=DIRECTION('',(0.703080940100181,0.703080940100181,-0.10655694879121));
#35097=DIRECTION('',(0.,-0.646692806155139,0.762750558483697));
#35098=DIRECTION('center_axis',(-0.553588677216093,-0.635211217279596,-0.538559454378353));
#35099=DIRECTION('ref_axis',(-0.697310151651835,0.,0.716769525303144));
#35100=DIRECTION('',(0.,0.646692806155139,-0.762750558483697));
#35101=DIRECTION('',(0.70308094010018,-0.703080940100181,0.10655694879121));
#35102=DIRECTION('center_axis',(-0.707106781186548,-0.707106781186547,0.));
#35103=DIRECTION('ref_axis',(0.,0.,1.));
#35104=DIRECTION('center_axis',(-0.707106781186548,-0.707106781186547,0.));
#35105=DIRECTION('ref_axis',(0.707106781186547,-0.707106781186548,0.));
#35106=DIRECTION('',(0.,0.,-1.));
#35107=DIRECTION('',(0.,0.,1.));
#35108=DIRECTION('center_axis',(0.553588677216087,0.635211217279597,-0.53855945437836));
#35109=DIRECTION('ref_axis',(-0.697310151651843,0.,-0.716769525303136));
#35110=DIRECTION('',(0.,-0.646692806155144,-0.762750558483693));
#35111=DIRECTION('',(-0.703080940100181,0.703080940100181,0.10655694879121));
#35112=DIRECTION('center_axis',(-0.553588677216087,0.635211217279596,-0.53855945437836));
#35113=DIRECTION('ref_axis',(-0.697310151651843,0.,0.716769525303136));
#35114=DIRECTION('',(0.,0.646692806155144,0.762750558483693));
#35115=DIRECTION('',(-0.70308094010018,-0.703080940100181,-0.10655694879121));
#35116=DIRECTION('center_axis',(-1.,0.,0.));
#35117=DIRECTION('ref_axis',(0.,0.159090909090909,-0.987263937680612));
#35118=DIRECTION('center_axis',(-1.,0.,0.));
#35119=DIRECTION('ref_axis',(0.,0.159090909090909,-0.987263937680612));
#35120=DIRECTION('center_axis',(1.,0.,0.));
#35121=DIRECTION('ref_axis',(0.,0.159090909090909,-0.987263937680612));
#35122=DIRECTION('center_axis',(-0.707106781186548,0.707106781186547,0.));
#35123=DIRECTION('ref_axis',(0.,0.,1.));
#35124=DIRECTION('center_axis',(-0.707106781186548,0.707106781186547,0.));
#35125=DIRECTION('ref_axis',(-0.707106781186547,-0.707106781186548,0.));
#35126=DIRECTION('',(0.,0.,-1.));
#35127=DIRECTION('',(0.,0.,1.));
#35128=DIRECTION('center_axis',(0.,0.762750558483693,-0.646692806155144));
#35129=DIRECTION('ref_axis',(-1.,0.,0.));
#35130=DIRECTION('',(-1.,0.,0.));
#35131=DIRECTION('',(1.,0.,0.));
#35132=DIRECTION('center_axis',(0.707106781186548,0.707106781186548,0.));
#35133=DIRECTION('ref_axis',(0.,0.,-1.));
#35134=DIRECTION('center_axis',(0.707106781186548,0.707106781186548,0.));
#35135=DIRECTION('ref_axis',(0.707106781186547,-0.707106781186547,0.));
#35136=DIRECTION('',(0.,0.,-1.));
#35137=DIRECTION('',(0.,0.,1.));
#35138=DIRECTION('center_axis',(1.,0.,0.));
#35139=DIRECTION('ref_axis',(0.,0.159090909090909,-0.987263937680612));
#35140=DIRECTION('center_axis',(1.,0.,0.));
#35141=DIRECTION('ref_axis',(0.,0.159090909090909,-0.987263937680612));
#35142=DIRECTION('center_axis',(-1.,0.,0.));
#35143=DIRECTION('ref_axis',(0.,0.159090909090909,-0.987263937680612));
#35144=DIRECTION('center_axis',(0.,-0.762750558483697,-0.646692806155139));
#35145=DIRECTION('ref_axis',(-1.,0.,0.));
#35146=DIRECTION('',(-1.,0.,0.));
#35147=DIRECTION('',(1.,0.,0.));
#35148=DIRECTION('center_axis',(0.707106781186548,-0.707106781186548,0.));
#35149=DIRECTION('ref_axis',(0.,0.,-1.));
#35150=DIRECTION('center_axis',(0.707106781186548,-0.707106781186548,0.));
#35151=DIRECTION('ref_axis',(-0.707106781186547,-0.707106781186547,0.));
#35152=DIRECTION('',(0.,0.,-1.));
#35153=DIRECTION('',(0.,0.,1.));
#35154=DIRECTION('center_axis',(1.,0.,0.));
#35155=DIRECTION('ref_axis',(0.,0.,-1.));
#35156=DIRECTION('center_axis',(1.,0.,0.));
#35157=DIRECTION('ref_axis',(0.,-0.127272727272727,0.991867759780789));
#35158=DIRECTION('center_axis',(0.,-1.,0.));
#35159=DIRECTION('ref_axis',(0.,0.,-1.));
#35160=DIRECTION('',(1.,0.,0.));
#35161=DIRECTION('center_axis',(1.,0.,0.));
#35162=DIRECTION('ref_axis',(0.,-4.28949804968811E-16,-1.));
#35163=DIRECTION('center_axis',(1.,0.,0.));
#35164=DIRECTION('ref_axis',(0.,1.4130111222502E-16,-1.));
#35165=DIRECTION('center_axis',(1.,0.,0.));
#35166=DIRECTION('ref_axis',(0.,-0.127272727272727,0.991867759780789));
#35167=DIRECTION('',(1.,0.,0.));
#35168=DIRECTION('center_axis',(0.,1.,0.));
#35169=DIRECTION('ref_axis',(0.,0.,1.));
#35170=DIRECTION('center_axis',(1.,0.,0.));
#35171=DIRECTION('ref_axis',(0.,0.,-1.));
#35172=DIRECTION('axis',(0.,0.,1.));
#35173=DIRECTION('refdir',(1.,0.,0.));
#35174=DIRECTION('center_axis',(-1.,0.,-3.52842604891459E-15));
#35175=DIRECTION('ref_axis',(0.,1.,3.1640767656135E-17));
#35176=DIRECTION('center_axis',(-1.,0.,0.));
#35177=DIRECTION('ref_axis',(0.,1.,0.));
#35178=DIRECTION('',(-0.258825179775134,-0.965924182487616,-1.06209968489537E-15));
#35179=DIRECTION('center_axis',(1.,0.,0.));
#35180=DIRECTION('ref_axis',(0.,1.,6.12323399573677E-17));
#35181=DIRECTION('center_axis',(-1.,0.,0.));
#35182=DIRECTION('ref_axis',(0.,1.,0.));
#35183=DIRECTION('',(0.500011000363013,0.866019052628739,1.06056746080241E-16));
#35184=DIRECTION('center_axis',(1.,0.,0.));
#35185=DIRECTION('ref_axis',(0.,0.,-1.));
#35186=DIRECTION('center_axis',(0.369852508213401,-0.804615959092168,0.464545240576681));
#35187=DIRECTION('ref_axis',(0.782331963393017,0.,-0.622861701386133));
#35188=DIRECTION('',(0.,0.500000000000002,0.866025403784438));
#35189=DIRECTION('center_axis',(0.369852508213402,4.69866669311145E-13,
0.929090481152538));
#35190=DIRECTION('ref_axis',(0.929090481152538,0.,-0.369852508213402));
#35191=DIRECTION('',(0.,1.,2.56395024851141E-15));
#35192=DIRECTION('center_axis',(0.369852508213404,-0.804615959092644,-0.464545240575855));
#35193=DIRECTION('ref_axis',(-0.782331963392475,0.,-0.622861701386813));
#35194=DIRECTION('',(-2.56395024851143E-15,-0.499999999999999,0.866025403784439));
#35195=DIRECTION('center_axis',(0.369852508213404,0.804615959092643,0.464545240575856));
#35196=DIRECTION('ref_axis',(0.782331963392475,0.,-0.622861701386812));
#35197=DIRECTION('',(1.28197512425571E-15,0.499999999999999,-0.866025403784439));
#35198=DIRECTION('center_axis',(0.3698525082134,-4.77010775225235E-13,-0.929090481152539));
#35199=DIRECTION('ref_axis',(-0.929090481152539,0.,-0.3698525082134));
#35200=DIRECTION('',(-1.28197512425571E-15,-1.,2.56395024851142E-15));
#35201=DIRECTION('center_axis',(0.369852508213402,0.80461595909217,-0.464545240576677));
#35202=DIRECTION('ref_axis',(-0.782331963393014,0.,-0.622861701386136));
#35203=DIRECTION('',(-2.56395024851142E-15,-0.499999999999997,-0.86602540378444));
#35204=DIRECTION('center_axis',(0.,0.86602540378444,-0.499999999999997));
#35205=DIRECTION('ref_axis',(0.,0.499999999999997,0.86602540378444));
#35206=DIRECTION('',(0.,0.499999999999997,0.86602540378444));
#35207=DIRECTION('',(1.,0.,0.));
#35208=DIRECTION('',(-1.,0.,0.));
#35209=DIRECTION('center_axis',(0.,-2.56395024851142E-15,-1.));
#35210=DIRECTION('ref_axis',(-1.,0.,0.));
#35211=DIRECTION('',(0.,1.,-2.56395024851142E-15));
#35212=DIRECTION('',(1.,0.,0.));
#35213=DIRECTION('',(-1.,0.,0.));
#35214=DIRECTION('center_axis',(0.,0.866025403784439,0.499999999999999));
#35215=DIRECTION('ref_axis',(0.,-0.499999999999999,0.866025403784439));
#35216=DIRECTION('',(0.,-0.499999999999999,0.866025403784439));
#35217=DIRECTION('',(1.,0.,0.));
#35218=DIRECTION('',(-1.,0.,0.));
#35219=DIRECTION('center_axis',(0.,-0.866025403784439,-0.499999999999999));
#35220=DIRECTION('ref_axis',(0.,0.499999999999999,-0.866025403784439));
#35221=DIRECTION('',(0.,0.499999999999999,-0.866025403784439));
#35222=DIRECTION('',(1.,0.,0.));
#35223=DIRECTION('',(-1.,0.,0.));
#35224=DIRECTION('center_axis',(0.,-2.56395024851141E-15,1.));
#35225=DIRECTION('ref_axis',(1.,0.,0.));
#35226=DIRECTION('',(0.,-1.,-2.56395024851141E-15));
#35227=DIRECTION('',(1.,0.,0.));
#35228=DIRECTION('',(-1.,0.,0.));
#35229=DIRECTION('center_axis',(0.,-0.866025403784438,0.500000000000002));
#35230=DIRECTION('ref_axis',(1.,0.,0.));
#35231=DIRECTION('',(0.,-0.500000000000002,-0.866025403784438));
#35232=DIRECTION('',(1.,0.,0.));
#35233=DIRECTION('',(-1.,0.,0.));
#35234=DIRECTION('center_axis',(1.,0.,0.));
#35235=DIRECTION('ref_axis',(0.,0.,-1.));
#35236=DIRECTION('',(0.,0.866025403784439,-0.5));
#35237=DIRECTION('center_axis',(1.,0.,0.));
#35238=DIRECTION('ref_axis',(0.,0.,-1.));
#35239=DIRECTION('',(0.,0.866025403784439,0.5));
#35240=DIRECTION('center_axis',(0.,-0.5,-0.866025403784439));
#35241=DIRECTION('ref_axis',(0.,0.866025403784439,-0.5));
#35242=DIRECTION('',(0.,0.866025403784439,-0.5));
#35243=DIRECTION('',(0.,-0.866025403784439,0.5));
#35244=DIRECTION('center_axis',(1.,0.,0.));
#35245=DIRECTION('ref_axis',(0.,0.,-1.));
#35246=DIRECTION('',(0.,1.28197512425571E-16,-1.));
#35247=DIRECTION('center_axis',(1.,0.,0.));
#35248=DIRECTION('ref_axis',(0.,0.,-1.));
#35249=DIRECTION('center_axis',(0.,-1.,-1.28197512425571E-16));
#35250=DIRECTION('ref_axis',(0.,1.28197512425571E-16,-1.));
#35251=DIRECTION('',(0.,1.28197512425571E-16,-1.));
#35252=DIRECTION('',(0.,-1.28197512425571E-16,1.));
#35253=DIRECTION('center_axis',(1.,0.,0.));
#35254=DIRECTION('ref_axis',(0.,0.,-1.));
#35255=DIRECTION('',(0.,-0.866025403784439,-0.5));
#35256=DIRECTION('center_axis',(1.,0.,0.));
#35257=DIRECTION('ref_axis',(0.,0.,-1.));
#35258=DIRECTION('center_axis',(0.,-0.5,0.866025403784439));
#35259=DIRECTION('ref_axis',(0.,-0.866025403784439,-0.5));
#35260=DIRECTION('',(0.,-0.866025403784439,-0.5));
#35261=DIRECTION('',(0.,0.866025403784439,0.5));
#35262=DIRECTION('center_axis',(0.,0.5,0.866025403784439));
#35263=DIRECTION('ref_axis',(0.,-0.866025403784439,0.5));
#35264=DIRECTION('',(0.,-0.866025403784439,0.5));
#35265=DIRECTION('',(0.,0.866025403784439,-0.5));
#35266=DIRECTION('',(0.,-0.866025403784439,0.5));
#35267=DIRECTION('center_axis',(0.,1.,-3.84592537276713E-16));
#35268=DIRECTION('ref_axis',(0.,3.84592537276713E-16,1.));
#35269=DIRECTION('',(0.,3.84592537276713E-16,1.));
#35270=DIRECTION('',(0.,-3.84592537276713E-16,-1.));
#35271=DIRECTION('',(0.,3.84592537276713E-16,1.));
#35272=DIRECTION('center_axis',(1.,0.,0.));
#35273=DIRECTION('ref_axis',(0.,0.,-1.));
#35274=DIRECTION('',(0.,0.866025403784439,0.5));
#35275=DIRECTION('center_axis',(1.,0.,0.));
#35276=DIRECTION('ref_axis',(0.,0.,-1.));
#35277=DIRECTION('center_axis',(1.,0.,0.));
#35278=DIRECTION('ref_axis',(0.,0.,-1.));
#35279=DIRECTION('center_axis',(1.,0.,0.));
#35280=DIRECTION('ref_axis',(0.,0.,-1.));
#35281=DIRECTION('center_axis',(1.,0.,0.));
#35282=DIRECTION('ref_axis',(0.,0.,-1.));
#35283=DIRECTION('center_axis',(1.,0.,0.));
#35284=DIRECTION('ref_axis',(0.,0.,-1.));
#35285=DIRECTION('center_axis',(0.,0.5,-0.866025403784439));
#35286=DIRECTION('ref_axis',(0.,0.866025403784439,0.5));
#35287=DIRECTION('',(0.,-0.866025403784439,-0.5));
#35288=DIRECTION('center_axis',(1.,0.,0.));
#35289=DIRECTION('ref_axis',(0.,0.,-1.));
#35290=DIRECTION('center_axis',(1.,0.,0.));
#35291=DIRECTION('ref_axis',(0.,0.,-1.));
#35292=DIRECTION('center_axis',(1.,0.,0.));
#35293=DIRECTION('ref_axis',(0.,0.,-1.));
#35294=DIRECTION('center_axis',(1.,0.,0.));
#35295=DIRECTION('ref_axis',(0.,0.,-1.));
#35296=DIRECTION('center_axis',(1.,0.,0.));
#35297=DIRECTION('ref_axis',(0.,0.,-1.));
#35298=DIRECTION('center_axis',(1.,0.,0.));
#35299=DIRECTION('ref_axis',(0.,0.,-1.));
#35300=DIRECTION('center_axis',(1.,0.,0.));
#35301=DIRECTION('ref_axis',(0.,0.,-1.));
#35302=DIRECTION('center_axis',(1.,0.,0.));
#35303=DIRECTION('ref_axis',(0.,0.,-1.));
#35304=DIRECTION('center_axis',(1.,0.,0.));
#35305=DIRECTION('ref_axis',(0.,0.,-1.));
#35306=DIRECTION('center_axis',(1.,0.,0.));
#35307=DIRECTION('ref_axis',(0.,0.,-1.));
#35308=DIRECTION('center_axis',(1.,0.,0.));
#35309=DIRECTION('ref_axis',(0.,0.,-1.));
#35310=DIRECTION('center_axis',(1.,0.,0.));
#35311=DIRECTION('ref_axis',(0.,0.,-1.));
#35312=DIRECTION('center_axis',(1.,0.,0.));
#35313=DIRECTION('ref_axis',(0.,0.,-1.));
#35314=DIRECTION('center_axis',(-1.,0.,0.));
#35315=DIRECTION('ref_axis',(0.,0.,1.));
#35316=DIRECTION('center_axis',(1.,0.,0.));
#35317=DIRECTION('ref_axis',(0.,0.,-1.));
#35318=DIRECTION('center_axis',(1.,0.,0.));
#35319=DIRECTION('ref_axis',(0.,1.,0.));
#35320=DIRECTION('center_axis',(1.,0.,0.));
#35321=DIRECTION('ref_axis',(0.,0.,-1.));
#35322=DIRECTION('',(-0.707106781186548,0.707106781186548,8.65956056235493E-17));
#35323=DIRECTION('center_axis',(1.,0.,0.));
#35324=DIRECTION('ref_axis',(0.,1.,0.));
#35325=DIRECTION('',(-1.,0.,0.));
#35326=DIRECTION('axis',(0.,0.,1.));
#35327=DIRECTION('refdir',(1.,0.,0.));
#35328=DIRECTION('center_axis',(-0.707106781186548,0.,-0.707106781186548));
#35329=DIRECTION('ref_axis',(-0.707106781186548,0.,0.707106781186548));
#35330=DIRECTION('',(-0.707106781186532,0.,0.707106781186563));
#35331=DIRECTION('',(0.,1.,0.));
#35332=DIRECTION('',(0.707106781186548,0.,-0.707106781186548));
#35333=DIRECTION('',(0.,-1.,0.));
#35334=DIRECTION('center_axis',(1.,0.,0.));
#35335=DIRECTION('ref_axis',(0.,-1.,-1.77635683940024E-15));
#35336=DIRECTION('',(-0.707106781186548,0.707106781186548,0.));
#35337=DIRECTION('center_axis',(1.,0.,0.));
#35338=DIRECTION('ref_axis',(0.,-1.,-1.77635683940024E-15));
#35339=DIRECTION('center_axis',(-1.,0.,0.));
#35340=DIRECTION('ref_axis',(0.,-1.,-1.77635683940024E-15));
#35341=DIRECTION('center_axis',(-0.707106781186548,-0.707106781186548,0.));
#35342=DIRECTION('ref_axis',(0.,0.,1.));
#35343=DIRECTION('',(-0.707106781186548,0.707106781186548,0.));
#35344=DIRECTION('',(0.,0.,-1.));
#35345=DIRECTION('',(0.,0.,1.));
#35346=DIRECTION('center_axis',(1.,0.,0.));
#35347=DIRECTION('ref_axis',(0.,-3.55271367880049E-15,1.));
#35348=DIRECTION('',(-0.707106781186548,0.,-0.707106781186548));
#35349=DIRECTION('center_axis',(1.,0.,0.));
#35350=DIRECTION('ref_axis',(0.,-3.5527136788005E-15,1.));
#35351=DIRECTION('center_axis',(-1.,0.,0.));
#35352=DIRECTION('ref_axis',(0.,-3.55271367880049E-15,1.));
#35353=DIRECTION('center_axis',(-0.707106781186548,0.,0.707106781186548));
#35354=DIRECTION('ref_axis',(0.707106781186548,0.,0.707106781186548));
#35355=DIRECTION('',(-0.7071067811865,0.,-0.707106781186595));
#35356=DIRECTION('',(0.,-1.,0.));
#35357=DIRECTION('',(0.,1.,0.));
#35358=DIRECTION('center_axis',(1.,0.,0.));
#35359=DIRECTION('ref_axis',(0.,1.,1.77635683940024E-15));
#35360=DIRECTION('',(-0.707106781186548,-0.707106781186548,0.));
#35361=DIRECTION('center_axis',(1.,0.,0.));
#35362=DIRECTION('ref_axis',(0.,1.,1.77635683940024E-15));
#35363=DIRECTION('center_axis',(-1.,0.,0.));
#35364=DIRECTION('ref_axis',(0.,1.,1.77635683940024E-15));
#35365=DIRECTION('center_axis',(-0.707106781186548,0.707106781186548,0.));
#35366=DIRECTION('ref_axis',(0.,0.,1.));
#35367=DIRECTION('',(-0.70710678118661,-0.707106781186485,0.));
#35368=DIRECTION('',(0.,0.,1.));
#35369=DIRECTION('',(0.,0.,-1.));
#35370=DIRECTION('center_axis',(1.,0.,0.));
#35371=DIRECTION('ref_axis',(0.,7.10542735760099E-15,-1.));
#35372=DIRECTION('center_axis',(1.,0.,0.));
#35373=DIRECTION('ref_axis',(0.,7.10542735760099E-15,-1.));
#35374=DIRECTION('center_axis',(-1.,0.,0.));
#35375=DIRECTION('ref_axis',(0.,7.10542735760099E-15,-1.));
#35376=DIRECTION('center_axis',(-1.,0.,0.));
#35377=DIRECTION('ref_axis',(0.,-3.55271367880049E-15,1.));
#35378=DIRECTION('',(-1.,0.,0.));
#35379=DIRECTION('center_axis',(1.,0.,0.));
#35380=DIRECTION('ref_axis',(0.,-3.55271367880049E-15,1.));
#35381=DIRECTION('',(-1.,0.,0.));
#35382=DIRECTION('center_axis',(0.,-1.,0.));
#35383=DIRECTION('ref_axis',(0.,0.,1.));
#35384=DIRECTION('',(-1.,0.,0.));
#35385=DIRECTION('',(0.,0.,-1.));
#35386=DIRECTION('center_axis',(-1.,0.,0.));
#35387=DIRECTION('ref_axis',(0.,-1.,-1.77635683940024E-15));
#35388=DIRECTION('',(-1.,0.,0.));
#35389=DIRECTION('center_axis',(1.,0.,0.));
#35390=DIRECTION('ref_axis',(0.,-1.,-1.77635683940024E-15));
#35391=DIRECTION('center_axis',(0.,0.,-1.));
#35392=DIRECTION('ref_axis',(0.,-1.,0.));
#35393=DIRECTION('',(-1.,0.,0.));
#35394=DIRECTION('',(0.,1.,0.));
#35395=DIRECTION('center_axis',(1.,0.,0.));
#35396=DIRECTION('ref_axis',(0.,0.,-1.));
#35397=DIRECTION('center_axis',(1.,0.,0.));
#35398=DIRECTION('ref_axis',(0.,0.,-1.));
#35399=DIRECTION('center_axis',(1.,0.,0.));
#35400=DIRECTION('ref_axis',(0.,0.,-1.));
#35401=DIRECTION('center_axis',(1.,0.,0.));
#35402=DIRECTION('ref_axis',(0.,0.,-1.));
#35403=DIRECTION('center_axis',(1.,0.,0.));
#35404=DIRECTION('ref_axis',(0.,0.,-1.));
#35405=DIRECTION('',(0.,1.,0.));
#35406=DIRECTION('center_axis',(1.,0.,0.));
#35407=DIRECTION('ref_axis',(0.,0.,-1.));
#35408=DIRECTION('',(0.,0.,1.));
#35409=DIRECTION('center_axis',(1.,0.,0.));
#35410=DIRECTION('ref_axis',(0.,1.,-4.44089209850064E-15));
#35411=DIRECTION('',(0.,-1.,0.));
#35412=DIRECTION('center_axis',(1.,0.,0.));
#35413=DIRECTION('ref_axis',(0.,-4.44089209850061E-15,1.));
#35414=DIRECTION('',(0.,0.,-1.));
#35415=DIRECTION('center_axis',(1.,0.,0.));
#35416=DIRECTION('ref_axis',(0.,-1.,-4.4408920985006E-15));
#35417=DIRECTION('center_axis',(0.707106781186548,0.,-0.707106781186548));
#35418=DIRECTION('ref_axis',(-0.707106781186548,0.,-0.707106781186548));
#35419=DIRECTION('',(0.707106781186548,0.,0.707106781186548));
#35420=DIRECTION('',(0.,-1.,0.));
#35421=DIRECTION('',(-0.707106781186532,0.,-0.707106781186563));
#35422=DIRECTION('center_axis',(-1.,0.,0.));
#35423=DIRECTION('ref_axis',(0.,7.10542735760099E-15,-1.));
#35424=DIRECTION('',(0.707106781186548,-0.707106781186548,0.));
#35425=DIRECTION('center_axis',(-1.,0.,0.));
#35426=DIRECTION('ref_axis',(0.,7.10542735760099E-15,-1.));
#35427=DIRECTION('center_axis',(1.,0.,0.));
#35428=DIRECTION('ref_axis',(0.,7.10542735760099E-15,-1.));
#35429=DIRECTION('center_axis',(0.707106781186548,0.707106781186548,0.));
#35430=DIRECTION('ref_axis',(0.,0.,-1.));
#35431=DIRECTION('',(0.707106781186548,-0.707106781186548,0.));
#35432=DIRECTION('',(0.,0.,-1.));
#35433=DIRECTION('',(0.,0.,1.));
#35434=DIRECTION('center_axis',(-1.,0.,0.));
#35435=DIRECTION('ref_axis',(0.,1.,1.77635683940024E-15));
#35436=DIRECTION('',(0.707106781186516,0.,-0.707106781186579));
#35437=DIRECTION('center_axis',(-1.,0.,0.));
#35438=DIRECTION('ref_axis',(0.,1.,1.77635683940024E-15));
#35439=DIRECTION('center_axis',(1.,0.,0.));
#35440=DIRECTION('ref_axis',(0.,1.,1.77635683940024E-15));
#35441=DIRECTION('center_axis',(0.707106781186548,0.,0.707106781186548));
#35442=DIRECTION('ref_axis',(0.707106781186548,0.,-0.707106781186548));
#35443=DIRECTION('',(0.707106781186548,0.,-0.707106781186548));
#35444=DIRECTION('',(0.,1.,0.));
#35445=DIRECTION('',(0.,-1.,0.));
#35446=DIRECTION('center_axis',(-1.,0.,0.));
#35447=DIRECTION('ref_axis',(0.,-3.55271367880049E-15,1.));
#35448=DIRECTION('',(0.707106781186548,0.707106781186548,0.));
#35449=DIRECTION('center_axis',(-1.,0.,0.));
#35450=DIRECTION('ref_axis',(0.,-3.5527136788005E-15,1.));
#35451=DIRECTION('center_axis',(0.707106781186548,-0.707106781186548,0.));
#35452=DIRECTION('ref_axis',(0.,0.,-1.));
#35453=DIRECTION('',(0.707106781186548,0.707106781186548,0.));
#35454=DIRECTION('',(0.,0.,1.));
#35455=DIRECTION('center_axis',(-1.,0.,0.));
#35456=DIRECTION('ref_axis',(0.,-1.,-1.77635683940024E-15));
#35457=DIRECTION('center_axis',(-1.,0.,0.));
#35458=DIRECTION('ref_axis',(0.,-1.,-1.77635683940024E-15));
#35459=DIRECTION('center_axis',(-1.,0.,0.));
#35460=DIRECTION('ref_axis',(0.,1.,1.77635683940024E-15));
#35461=DIRECTION('',(-1.,0.,0.));
#35462=DIRECTION('',(-1.,0.,0.));
#35463=DIRECTION('center_axis',(0.,1.,0.));
#35464=DIRECTION('ref_axis',(0.,0.,-1.));
#35465=DIRECTION('',(-1.,0.,0.));
#35466=DIRECTION('center_axis',(-1.,0.,0.));
#35467=DIRECTION('ref_axis',(0.,7.10542735760099E-15,-1.));
#35468=DIRECTION('center_axis',(1.,0.,0.));
#35469=DIRECTION('ref_axis',(0.,0.,-1.));
#35470=DIRECTION('center_axis',(-1.,0.,0.));
#35471=DIRECTION('ref_axis',(0.,0.,-1.));
#35472=DIRECTION('center_axis',(-1.,0.,0.));
#35473=DIRECTION('ref_axis',(0.,0.,-1.));
#35474=DIRECTION('center_axis',(-1.,0.,0.));
#35475=DIRECTION('ref_axis',(0.,0.,-1.));
#35476=DIRECTION('center_axis',(-1.,0.,0.));
#35477=DIRECTION('ref_axis',(0.,0.,-1.));
#35478=DIRECTION('center_axis',(-0.70710678118654,0.,-0.707106781186555));
#35479=DIRECTION('ref_axis',(-0.707106781186555,0.,0.70710678118654));
#35480=DIRECTION('',(-0.707106781186548,0.,0.707106781186548));
#35481=DIRECTION('',(0.,1.,0.));
#35482=DIRECTION('',(0.707106781186555,0.,-0.70710678118654));
#35483=DIRECTION('',(0.,-1.,0.));
#35484=DIRECTION('center_axis',(1.,0.,0.));
#35485=DIRECTION('ref_axis',(0.,-1.,-4.4408920985006E-15));
#35486=DIRECTION('',(-0.707106781186548,0.707106781186548,0.));
#35487=DIRECTION('center_axis',(1.,0.,0.));
#35488=DIRECTION('ref_axis',(0.,-1.,-4.4408920985006E-15));
#35489=DIRECTION('center_axis',(-1.,0.,0.));
#35490=DIRECTION('ref_axis',(0.,-1.,-4.4408920985006E-15));
#35491=DIRECTION('center_axis',(-0.707106781186532,-0.707106781186563,0.));
#35492=DIRECTION('ref_axis',(0.,0.,1.));
#35493=DIRECTION('',(-0.707106781186563,0.707106781186532,1.57009245868377E-14));
#35494=DIRECTION('',(0.,0.,-1.));
#35495=DIRECTION('',(0.,0.,1.));
#35496=DIRECTION('center_axis',(1.,0.,0.));
#35497=DIRECTION('ref_axis',(0.,-4.44089209850061E-15,1.));
#35498=DIRECTION('',(-0.707106781186548,0.,-0.707106781186548));
#35499=DIRECTION('center_axis',(1.,0.,0.));
#35500=DIRECTION('ref_axis',(0.,-4.44089209850061E-15,1.));
#35501=DIRECTION('center_axis',(-1.,0.,0.));
#35502=DIRECTION('ref_axis',(0.,-4.44089209850061E-15,1.));
#35503=DIRECTION('center_axis',(-0.70710678118654,0.,0.707106781186555));
#35504=DIRECTION('ref_axis',(0.707106781186555,0.,0.70710678118654));
#35505=DIRECTION('',(-0.707106781186548,0.,-0.707106781186548));
#35506=DIRECTION('',(0.,-1.,0.));
#35507=DIRECTION('',(0.,1.,0.));
#35508=DIRECTION('center_axis',(1.,0.,0.));
#35509=DIRECTION('ref_axis',(0.,1.,-4.44089209850064E-15));
#35510=DIRECTION('',(-0.707106781186548,-0.707106781186548,0.));
#35511=DIRECTION('center_axis',(1.,0.,0.));
#35512=DIRECTION('ref_axis',(0.,1.,-4.44089209850064E-15));
#35513=DIRECTION('center_axis',(-1.,0.,0.));
#35514=DIRECTION('ref_axis',(0.,1.,-4.44089209850064E-15));
#35515=DIRECTION('center_axis',(-0.707106781186532,0.707106781186563,0.));
#35516=DIRECTION('ref_axis',(0.,0.,1.));
#35517=DIRECTION('',(-0.707106781186563,-0.707106781186532,-1.57009245868377E-14));
#35518=DIRECTION('',(0.,0.,1.));
#35519=DIRECTION('',(0.,0.,-1.));
#35520=DIRECTION('center_axis',(1.,0.,0.));
#35521=DIRECTION('ref_axis',(0.,0.,-1.));
#35522=DIRECTION('center_axis',(1.,0.,0.));
#35523=DIRECTION('ref_axis',(0.,0.,-1.));
#35524=DIRECTION('center_axis',(-1.,0.,0.));
#35525=DIRECTION('ref_axis',(0.,0.,-1.));
#35526=DIRECTION('center_axis',(-1.,0.,0.));
#35527=DIRECTION('ref_axis',(0.,-4.44089209850061E-15,1.));
#35528=DIRECTION('',(-1.,0.,0.));
#35529=DIRECTION('',(-1.,0.,0.));
#35530=DIRECTION('center_axis',(0.,-1.,0.));
#35531=DIRECTION('ref_axis',(0.,0.,1.));
#35532=DIRECTION('',(-1.,0.,0.));
#35533=DIRECTION('center_axis',(-1.,0.,0.));
#35534=DIRECTION('ref_axis',(0.,-1.,-4.4408920985006E-15));
#35535=DIRECTION('',(-1.,0.,0.));
#35536=DIRECTION('center_axis',(0.,0.,-1.));
#35537=DIRECTION('ref_axis',(0.,-1.,0.));
#35538=DIRECTION('',(-1.,0.,0.));
#35539=DIRECTION('center_axis',(1.,0.,0.));
#35540=DIRECTION('ref_axis',(0.,0.,-1.));
#35541=DIRECTION('center_axis',(-1.,0.,0.));
#35542=DIRECTION('ref_axis',(0.,0.,-1.));
#35543=DIRECTION('',(-1.,0.,0.));
#35544=DIRECTION('center_axis',(0.,1.,0.));
#35545=DIRECTION('ref_axis',(0.,0.,-1.));
#35546=DIRECTION('',(-1.,0.,0.));
#35547=DIRECTION('center_axis',(-1.,0.,0.));
#35548=DIRECTION('ref_axis',(0.,1.,-4.44089209850064E-15));
#35549=DIRECTION('',(-1.,0.,0.));
#35550=DIRECTION('center_axis',(0.,0.,1.));
#35551=DIRECTION('ref_axis',(0.,1.,0.));
#35552=DIRECTION('center_axis',(-1.,0.,0.));
#35553=DIRECTION('ref_axis',(0.,0.,-1.));
#35554=DIRECTION('',(-1.,0.,0.));
#35555=DIRECTION('center_axis',(-1.,0.,0.));
#35556=DIRECTION('ref_axis',(0.,0.,-1.));
#35557=DIRECTION('',(-1.,0.,0.));
#35558=DIRECTION('center_axis',(-1.,0.,0.));
#35559=DIRECTION('ref_axis',(0.,0.,-1.));
#35560=DIRECTION('',(-1.,0.,0.));
#35561=DIRECTION('center_axis',(-1.,0.,0.));
#35562=DIRECTION('ref_axis',(0.,0.,-1.));
#35563=DIRECTION('',(-1.,0.,0.));
#35564=DIRECTION('center_axis',(0.,0.,1.));
#35565=DIRECTION('ref_axis',(0.,1.,0.));
#35566=DIRECTION('axis',(0.,0.,1.));
#35567=DIRECTION('refdir',(1.,0.,0.));
#35568=DIRECTION('center_axis',(-1.,0.,-4.21782140988753E-15));
#35569=DIRECTION('ref_axis',(0.,-1.,-3.1162263922408E-17));
#35570=DIRECTION('center_axis',(1.,0.,0.));
#35571=DIRECTION('ref_axis',(0.,-1.,-6.12323399573677E-17));
#35572=DIRECTION('center_axis',(1.,0.,0.));
#35573=DIRECTION('ref_axis',(0.,-1.,-6.12323399573677E-17));
#35574=DIRECTION('center_axis',(-1.,0.,0.));
#35575=DIRECTION('ref_axis',(0.,-1.,0.));
#35576=DIRECTION('center_axis',(-1.,0.,0.));
#35577=DIRECTION('ref_axis',(0.,1.,0.));
#35578=DIRECTION('',(-0.707106781186552,-0.707106781186543,-8.65956056235487E-17));
#35579=DIRECTION('center_axis',(-1.,0.,0.));
#35580=DIRECTION('ref_axis',(0.,-1.,-6.12323399573676E-17));
#35581=DIRECTION('center_axis',(-1.,0.,0.));
#35582=DIRECTION('ref_axis',(0.,-1.,-6.12323399573676E-17));
#35583=DIRECTION('center_axis',(1.,0.,0.));
#35584=DIRECTION('ref_axis',(0.,0.,-1.));
#35585=DIRECTION('center_axis',(1.,0.,0.));
#35586=DIRECTION('ref_axis',(0.,1.,6.12323399573677E-17));
#35587=DIRECTION('center_axis',(1.,0.,0.));
#35588=DIRECTION('ref_axis',(0.,0.,-1.));
#35589=DIRECTION('center_axis',(1.,0.,0.));
#35590=DIRECTION('ref_axis',(0.,1.,6.12323399573677E-17));
#35591=DIRECTION('center_axis',(1.,0.,0.));
#35592=DIRECTION('ref_axis',(0.,0.,-1.));
#35593=DIRECTION('center_axis',(1.,0.,-4.21782140988753E-15));
#35594=DIRECTION('ref_axis',(0.,-1.,-3.1162263922408E-17));
#35595=DIRECTION('center_axis',(-1.,0.,0.));
#35596=DIRECTION('ref_axis',(0.,-1.,-6.12323399573677E-17));
#35597=DIRECTION('center_axis',(-1.,0.,0.));
#35598=DIRECTION('ref_axis',(0.,-1.,-6.12323399573677E-17));
#35599=DIRECTION('',(-0.382683432365103,-0.923879532511281,1.47215758518538E-15));
#35600=DIRECTION('center_axis',(1.,0.,0.));
#35601=DIRECTION('ref_axis',(0.,-1.,0.));
#35602=DIRECTION('center_axis',(1.,0.,0.));
#35603=DIRECTION('ref_axis',(0.,1.,0.));
#35604=DIRECTION('center_axis',(1.,0.,0.));
#35605=DIRECTION('ref_axis',(0.,-1.,-6.12323399573676E-17));
#35606=DIRECTION('center_axis',(1.,0.,0.));
#35607=DIRECTION('ref_axis',(0.,-1.,-6.12323399573676E-17));
#35608=DIRECTION('',(-0.707106781186552,0.707106781186543,8.65956056235487E-17));
#35609=DIRECTION('center_axis',(-1.,0.,0.));
#35610=DIRECTION('ref_axis',(0.,0.,1.));
#35611=DIRECTION('center_axis',(1.,0.,0.));
#35612=DIRECTION('ref_axis',(0.,0.,-1.));
#35613=DIRECTION('center_axis',(-1.,0.,-4.21782140988753E-15));
#35614=DIRECTION('ref_axis',(0.,1.,3.1162263922408E-17));
#35615=DIRECTION('center_axis',(-1.,0.,0.));
#35616=DIRECTION('ref_axis',(0.,1.,0.));
#35617=DIRECTION('center_axis',(-1.,0.,-4.21782140988753E-15));
#35618=DIRECTION('ref_axis',(0.,1.,3.1162263922408E-17));
#35619=DIRECTION('center_axis',(-1.,0.,0.));
#35620=DIRECTION('ref_axis',(0.,1.,0.));
#35621=DIRECTION('center_axis',(0.553280795424863,-0.635591688956665,-0.538426936866317));
#35622=DIRECTION('ref_axis',(-0.697421280285469,0.,-0.716661396898826));
#35623=DIRECTION('',(0.703011344182424,0.703011344182365,-0.107471391084913));
#35624=DIRECTION('',(0.,-0.646374896130196,0.763019982472725));
#35625=DIRECTION('',(-0.703011344182424,-0.00956522589581351,-0.71111430614521));
#35626=DIRECTION('center_axis',(0.,-0.763019982472725,-0.646374896130196));
#35627=DIRECTION('ref_axis',(-1.,0.,0.));
#35628=DIRECTION('',(0.,-0.646374896130196,0.763019982472725));
#35629=DIRECTION('',(1.,0.,0.));
#35630=DIRECTION('',(-1.,0.,0.));
#35631=DIRECTION('center_axis',(0.61702108254174,0.508662540160709,-0.600455996669427));
#35632=DIRECTION('ref_axis',(-0.697421280285471,0.,-0.716661396898825));
#35633=DIRECTION('',(0.701419241812877,-0.0095435636297033,0.712685040959816));
#35634=DIRECTION('',(0.,-0.763019982472724,-0.646374896130198));
#35635=DIRECTION('',(-0.701419241812879,0.701419241812816,-0.126578412177515));
#35636=DIRECTION('center_axis',(0.553280795424862,-0.635591688956666,0.538426936866317));
#35637=DIRECTION('ref_axis',(0.69742128028547,0.,-0.716661396898825));
#35638=DIRECTION('',(0.703011344182427,0.00956522589581354,-0.711114306145207));
#35639=DIRECTION('',(0.,0.646374896130195,0.763019982472726));
#35640=DIRECTION('',(-0.703011344182424,-0.703011344182364,-0.107471391084915));
#35641=DIRECTION('center_axis',(0.,-0.763019982472726,0.646374896130195));
#35642=DIRECTION('ref_axis',(1.,0.,0.));
#35643=DIRECTION('',(0.,0.646374896130195,0.763019982472726));
#35644=DIRECTION('',(1.,0.,0.));
#35645=DIRECTION('',(-1.,0.,0.));
#35646=DIRECTION('center_axis',(0.707106781186518,-0.707106781186577,0.));
#35647=DIRECTION('ref_axis',(0.,0.,-1.));
#35648=DIRECTION('',(0.,0.,1.));
#35649=DIRECTION('',(0.,0.,-1.));
#35650=DIRECTION('center_axis',(-0.617021082541767,0.508662540160695,-0.60045599666941));
#35651=DIRECTION('ref_axis',(-0.697421280285445,0.,0.71666139689885));
#35652=DIRECTION('',(0.,0.763019982472724,0.646374896130198));
#35653=DIRECTION('',(0.701419241812852,0.00954356362970364,-0.712685040959841));
#35654=DIRECTION('',(-0.701419241812853,-0.701419241812841,0.12657841217752));
#35655=DIRECTION('center_axis',(-0.707106781186542,-0.11624763874382,-0.697485832462921));
#35656=DIRECTION('ref_axis',(-0.702246883176789,0.,0.711933504667737));
#35657=DIRECTION('',(0.,0.986393923832144,-0.164398987305357));
#35658=DIRECTION('',(0.,-0.986393923832144,0.164398987305357));
#35659=DIRECTION('center_axis',(0.617021082541738,0.508662540160709,0.600455996669429));
#35660=DIRECTION('ref_axis',(0.697421280285473,0.,-0.716661396898823));
#35661=DIRECTION('',(0.701419241812879,-0.701419241812817,-0.126578412177511));
#35662=DIRECTION('',(0.,0.763019982472725,-0.646374896130197));
#35663=DIRECTION('',(-0.701419241812879,0.00954356362970333,0.712685040959814));
#35664=DIRECTION('center_axis',(-0.617021082541767,0.508662540160693,0.600455996669412));
#35665=DIRECTION('ref_axis',(0.697421280285446,0.,0.716661396898849));
#35666=DIRECTION('',(0.,-0.763019982472725,0.646374896130197));
#35667=DIRECTION('',(0.701419241812853,0.701419241812841,0.126578412177521));
#35668=DIRECTION('',(-0.701419241812852,-0.00954356362970365,-0.71268504095984));
#35669=DIRECTION('center_axis',(-0.707106781186541,0.707106781186554,0.));
#35670=DIRECTION('ref_axis',(0.,0.,1.));
#35671=DIRECTION('',(0.,0.,-1.));
#35672=DIRECTION('',(0.,0.,1.));
#35673=DIRECTION('center_axis',(-0.707106781186542,-0.11624763874382,0.697485832462921));
#35674=DIRECTION('ref_axis',(0.702246883176789,0.,0.711933504667736));
#35675=DIRECTION('',(0.,0.986393923832144,0.164398987305357));
#35676=DIRECTION('',(0.,-0.986393923832144,-0.164398987305357));
#35677=DIRECTION('center_axis',(0.,0.646374896130197,0.763019982472725));
#35678=DIRECTION('ref_axis',(1.,0.,0.));
#35679=DIRECTION('',(-1.,0.,0.));
#35680=DIRECTION('',(1.,0.,0.));
#35681=DIRECTION('center_axis',(0.707106781186515,-0.116247638743825,0.697485832462947));
#35682=DIRECTION('ref_axis',(0.702246883176816,0.,-0.71193350466771));
#35683=DIRECTION('',(0.,0.986393923832144,0.164398987305357));
#35684=DIRECTION('',(0.,-0.986393923832144,-0.164398987305357));
#35685=DIRECTION('center_axis',(0.707106781186516,0.707106781186579,0.));
#35686=DIRECTION('ref_axis',(0.,0.,-1.));
#35687=DIRECTION('',(0.,0.,-1.));
#35688=DIRECTION('',(0.,0.,1.));
#35689=DIRECTION('center_axis',(0.,0.646374896130198,-0.763019982472724));
#35690=DIRECTION('ref_axis',(-1.,0.,0.));
#35691=DIRECTION('',(-1.,0.,0.));
#35692=DIRECTION('',(1.,0.,0.));
#35693=DIRECTION('center_axis',(0.707106781186517,-0.116247638743824,-0.697485832462946));
#35694=DIRECTION('ref_axis',(-0.702246883176814,0.,-0.711933504667711));
#35695=DIRECTION('',(0.,-0.986393923832144,0.164398987305357));
#35696=DIRECTION('',(0.,0.986393923832144,-0.164398987305357));
#35697=DIRECTION('center_axis',(0.,-0.164398987305357,-0.986393923832144));
#35698=DIRECTION('ref_axis',(0.,0.986393923832144,-0.164398987305357));
#35699=DIRECTION('',(0.,-0.986393923832144,0.164398987305357));
#35700=DIRECTION('center_axis',(0.,-1.,0.));
#35701=DIRECTION('ref_axis',(0.,0.,-1.));
#35702=DIRECTION('',(0.,0.,1.));
#35703=DIRECTION('center_axis',(1.,0.,0.));
#35704=DIRECTION('ref_axis',(0.,0.,-1.));
#35705=DIRECTION('center_axis',(0.,1.,0.));
#35706=DIRECTION('ref_axis',(0.,0.,1.));
#35707=DIRECTION('center_axis',(1.,0.,1.76809044889307E-15));
#35708=DIRECTION('ref_axis',(0.,-1.,-3.03981392545898E-17));
#35709=DIRECTION('center_axis',(-1.,0.,0.));
#35710=DIRECTION('ref_axis',(0.,-1.,0.));
#35711=DIRECTION('center_axis',(-1.,0.,0.));
#35712=DIRECTION('ref_axis',(0.,-1.,0.));
#35713=DIRECTION('',(-0.923879532511294,-0.382683432365072,-1.69200064568173E-15));
#35714=DIRECTION('center_axis',(1.,0.,0.));
#35715=DIRECTION('ref_axis',(0.,1.,0.));
#35716=DIRECTION('center_axis',(1.,0.,0.));
#35717=DIRECTION('ref_axis',(0.,-1.,0.));
#35718=DIRECTION('center_axis',(1.,0.,0.));
#35719=DIRECTION('ref_axis',(0.,-1.,0.));
#35720=DIRECTION('',(-1.,0.,0.));
#35721=DIRECTION('center_axis',(-1.,0.,1.76809044889307E-15));
#35722=DIRECTION('ref_axis',(0.,-1.,-3.03981392545898E-17));
#35723=DIRECTION('',(-0.923879532511294,0.382683432365072,1.69200064568173E-15));
#35724=DIRECTION('center_axis',(0.553280795424864,0.784087249886401,-0.281225080637575));
#35725=DIRECTION('ref_axis',(-0.453113352871865,0.,-0.891452909271834));
#35726=DIRECTION('',(0.703011344182424,-0.258432717231594,0.66256137875303));
#35727=DIRECTION('',(0.,-0.337607240351444,-0.941287071653639));
#35728=DIRECTION('',(-0.703011344182424,0.620625667064205,0.34727342445389));
#35729=DIRECTION('center_axis',(0.,0.941287071653639,-0.337607240351444));
#35730=DIRECTION('ref_axis',(0.,0.337607240351444,0.941287071653639));
#35731=DIRECTION('',(0.,-0.337607240351444,-0.941287071653639));
#35732=DIRECTION('',(1.,0.,0.));
#35733=DIRECTION('',(-1.,0.,0.));
#35734=DIRECTION('center_axis',(0.707106781186518,0.662164269064559,0.248069507949364));
#35735=DIRECTION('ref_axis',(0.331042401509786,0.,-0.943615879689736));
#35736=DIRECTION('',(0.542846344219036,-0.283533375605797,-0.79052303665713));
#35737=DIRECTION('',(0.,0.350823262553197,-0.936441689829928));
#35738=DIRECTION('',(0.,-0.350823262553197,0.936441689829928));
#35739=DIRECTION('',(0.606604029806706,-0.748327100188909,0.268399147064822));
#35740=DIRECTION('center_axis',(0.707106781186517,0.353553390593289,-0.612372435695821));
#35741=DIRECTION('ref_axis',(-0.65465367070801,0.,-0.755928946018426));
#35742=DIRECTION('',(-0.542846344219037,0.82637971982479,-0.149714412233186));
#35743=DIRECTION('',(0.,0.866025403784439,0.5));
#35744=DIRECTION('',(0.,-0.866025403784439,-0.5));
#35745=DIRECTION('',(-0.60660402980671,-0.14172307038225,-0.782269852636344));
#35746=DIRECTION('center_axis',(0.,0.936441689829928,0.350823262553197));
#35747=DIRECTION('ref_axis',(0.,-0.350823262553197,0.936441689829928));
#35748=DIRECTION('',(0.,0.350823262553197,-0.936441689829928));
#35749=DIRECTION('',(0.,-0.350823262553197,0.936441689829928));
#35750=DIRECTION('',(-0.702246883176787,0.249762834828468,-0.6666842141576));
#35751=DIRECTION('',(-1.,0.,0.));
#35752=DIRECTION('center_axis',(0.,0.5,-0.866025403784439));
#35753=DIRECTION('ref_axis',(0.,0.866025403784439,0.5));
#35754=DIRECTION('',(1.,0.,0.));
#35755=DIRECTION('',(0.,-0.866025403784439,-0.5));
#35756=DIRECTION('center_axis',(0.,-0.178267089180912,-0.983982136481636));
#35757=DIRECTION('ref_axis',(-1.,0.,0.));
#35758=DIRECTION('',(-0.542846344219054,-0.82637971982478,0.149714412233182));
#35759=DIRECTION('',(-1.,0.,0.));
#35760=DIRECTION('',(0.,-0.983982136481636,0.178267089180912));
#35761=DIRECTION('center_axis',(0.617021082541744,-0.774341417050779,0.140286683397983));
#35762=DIRECTION('ref_axis',(0.221703181086956,0.,-0.975114198181897));
#35763=DIRECTION('',(0.701419241812875,0.460329741422837,-0.544157676024363));
#35764=DIRECTION('',(0.,0.178267089180919,0.983982136481635));
#35765=DIRECTION('',(-0.701419241812876,-0.621975132183211,-0.348077551933944));
#35766=DIRECTION('center_axis',(-0.617021082541771,-0.774341417050759,0.140286683397977));
#35767=DIRECTION('ref_axis',(0.221703181086938,0.,0.975114198181901));
#35768=DIRECTION('',(0.,-0.178267089180919,-0.983982136481635));
#35769=DIRECTION('',(0.70141924181285,-0.460329741422853,0.544157676024382));
#35770=DIRECTION('',(-0.701419241812853,0.621975132183231,0.348077551933954));
#35771=DIRECTION('center_axis',(-0.707106781186544,-0.353553390593275,0.612372435695797));
#35772=DIRECTION('ref_axis',(0.654653670707981,0.,0.755928946018452));
#35773=DIRECTION('',(0.,-0.866025403784439,-0.5));
#35774=DIRECTION('',(0.,0.866025403784439,0.5));
#35775=DIRECTION('',(-0.606604029806695,0.748327100188916,-0.268399147064825));
#35776=DIRECTION('center_axis',(-0.707106781186542,-0.545916630320717,-0.449416324513565));
#35777=DIRECTION('ref_axis',(-0.536399063209287,0.,0.843964480880682));
#35778=DIRECTION('',(0.,-0.635570661278947,0.772042702524571));
#35779=DIRECTION('',(0.,0.635570661278947,-0.772042702524571));
#35780=DIRECTION('center_axis',(0.,-0.983982136481635,0.178267089180919));
#35781=DIRECTION('ref_axis',(0.,-0.178267089180919,-0.983982136481635));
#35782=DIRECTION('',(-1.,0.,0.));
#35783=DIRECTION('',(1.,0.,0.));
#35784=DIRECTION('center_axis',(0.707106781186517,-0.545916630320736,-0.449416324513581));
#35785=DIRECTION('ref_axis',(-0.536399063209314,0.,-0.843964480880665));
#35786=DIRECTION('',(0.,-0.635570661278947,0.772042702524571));
#35787=DIRECTION('',(0.,0.635570661278947,-0.772042702524571));
#35788=DIRECTION('center_axis',(0.707106781186519,-0.353553390593288,0.612372435695819));
#35789=DIRECTION('ref_axis',(0.654653670708007,0.,-0.755928946018428));
#35790=DIRECTION('',(0.606604029806723,0.748327100188896,-0.268399147064818));
#35791=DIRECTION('',(0.,-0.866025403784439,-0.5));
#35792=DIRECTION('',(0.,0.866025403784439,0.5));
#35793=DIRECTION('center_axis',(0.,0.33760724035145,0.941287071653637));
#35794=DIRECTION('ref_axis',(1.,0.,0.));
#35795=DIRECTION('',(1.,0.,0.));
#35796=DIRECTION('center_axis',(0.,-0.772042702524571,-0.635570661278947));
#35797=DIRECTION('ref_axis',(0.,0.635570661278947,-0.772042702524571));
#35798=DIRECTION('',(0.,-0.635570661278947,0.772042702524571));
#35799=DIRECTION('center_axis',(1.,0.,0.));
#35800=DIRECTION('ref_axis',(0.,0.,-1.));
#35801=DIRECTION('center_axis',(0.,-0.5,0.866025403784439));
#35802=DIRECTION('ref_axis',(0.,-0.866025403784439,-0.5));
#35803=DIRECTION('center_axis',(0.55328079542486,-0.148495560929736,0.81965201750389));
#35804=DIRECTION('ref_axis',(0.828841319689926,0.,-0.559483750232893));
#35805=DIRECTION('',(0.703011344182424,-0.44457862695077,-0.555089987668116));
#35806=DIRECTION('',(0.,0.983982136481636,0.178267089180912));
#35807=DIRECTION('',(-0.703011344182425,-0.611060441168389,0.363840881691315));
#35808=DIRECTION('center_axis',(0.,-0.178267089180912,0.983982136481636));
#35809=DIRECTION('ref_axis',(1.,0.,0.));
#35810=DIRECTION('',(0.,0.983982136481636,0.178267089180912));
#35811=DIRECTION('',(1.,0.,0.));
#35812=DIRECTION('',(-1.,0.,0.));
#35813=DIRECTION('center_axis',(0.617021082541743,-0.77434141705078,-0.140286683397981));
#35814=DIRECTION('ref_axis',(-0.221703181086953,0.,-0.975114198181898));
#35815=DIRECTION('',(0.701419241812879,0.621975132183207,-0.348077551933945));
#35816=DIRECTION('',(0.,-0.178267089180915,0.983982136481635));
#35817=DIRECTION('',(-0.701419241812875,-0.460329741422837,-0.544157676024363));
#35818=DIRECTION('center_axis',(0.553280795424862,0.784087249886404,0.281225080637571));
#35819=DIRECTION('ref_axis',(0.453113352871861,0.,-0.891452909271836));
#35820=DIRECTION('',(0.703011344182424,-0.620625667064201,0.347273424453897));
#35821=DIRECTION('',(0.,0.337607240351439,-0.941287071653641));
#35822=DIRECTION('',(-0.703011344182424,0.258432717231595,0.66256137875303));
#35823=DIRECTION('center_axis',(0.,0.941287071653641,0.337607240351439));
#35824=DIRECTION('ref_axis',(0.,-0.337607240351439,0.941287071653641));
#35825=DIRECTION('',(0.,0.337607240351439,-0.941287071653641));
#35826=DIRECTION('',(1.,0.,0.));
#35827=DIRECTION('',(-1.,0.,0.));
#35828=DIRECTION('center_axis',(0.707106781186517,0.353553390593289,0.61237243569582));
#35829=DIRECTION('ref_axis',(0.654653670708009,0.,-0.755928946018427));
#35830=DIRECTION('',(0.,0.866025403784438,-0.500000000000001));
#35831=DIRECTION('',(0.,-0.866025403784438,0.500000000000001));
#35832=DIRECTION('center_axis',(-0.617021082541769,-0.77434141705076,-0.140286683397974));
#35833=DIRECTION('ref_axis',(-0.221703181086934,0.,0.975114198181902));
#35834=DIRECTION('',(0.,0.178267089180915,-0.983982136481635));
#35835=DIRECTION('',(0.701419241812854,-0.621975132183229,0.348077551933958));
#35836=DIRECTION('',(-0.70141924181285,0.460329741422853,0.544157676024382));
#35837=DIRECTION('center_axis',(-0.707106781186542,-0.545916630320716,0.449416324513565));
#35838=DIRECTION('ref_axis',(0.536399063209287,0.,0.843964480880682));
#35839=DIRECTION('',(0.,-0.635570661278947,-0.77204270252457));
#35840=DIRECTION('',(0.,0.635570661278947,0.77204270252457));
#35841=DIRECTION('center_axis',(0.617021082541747,0.265678876890073,-0.740742680067404));
#35842=DIRECTION('ref_axis',(-0.768356185646342,0.,-0.640022477713872));
#35843=DIRECTION('',(0.701419241812876,0.241089500389983,0.67073608820188));
#35844=DIRECTION('',(0.,-0.941287071653641,-0.337607240351439));
#35845=DIRECTION('',(-0.701419241812877,0.612431568553495,-0.364607489025876));
#35846=DIRECTION('center_axis',(-0.617021082541771,0.265678876890066,-0.740742680067387));
#35847=DIRECTION('ref_axis',(-0.768356185646323,0.,0.640022477713895));
#35848=DIRECTION('',(0.,0.941287071653641,0.337607240351439));
#35849=DIRECTION('',(0.70141924181285,-0.241089500389991,-0.670736088201903));
#35850=DIRECTION('',(-0.701419241812852,-0.61243156855352,0.364607489025883));
#35851=DIRECTION('center_axis',(-0.707106781186544,-0.353553390593276,-0.612372435695797));
#35852=DIRECTION('ref_axis',(-0.65465367070798,0.,0.755928946018452));
#35853=DIRECTION('',(0.,-0.866025403784438,0.5));
#35854=DIRECTION('',(0.,0.866025403784438,-0.5));
#35855=DIRECTION('center_axis',(-0.707106781186543,0.662164269064536,-0.248069507949356));
#35856=DIRECTION('ref_axis',(-0.331042401509766,0.,0.943615879689743));
#35857=DIRECTION('',(0.,-0.350823262553198,-0.936441689829927));
#35858=DIRECTION('',(0.,0.350823262553198,0.936441689829927));
#35859=DIRECTION('center_axis',(0.,0.337607240351439,-0.941287071653641));
#35860=DIRECTION('ref_axis',(-1.,0.,0.));
#35861=DIRECTION('',(-1.,0.,0.));
#35862=DIRECTION('',(1.,0.,0.));
#35863=DIRECTION('center_axis',(0.707106781186517,0.66216426906456,-0.248069507949365));
#35864=DIRECTION('ref_axis',(-0.331042401509787,0.,-0.943615879689735));
#35865=DIRECTION('',(0.,-0.350823262553198,-0.936441689829927));
#35866=DIRECTION('',(0.,0.350823262553198,0.936441689829927));
#35867=DIRECTION('center_axis',(0.707106781186519,-0.353553390593288,-0.612372435695819));
#35868=DIRECTION('ref_axis',(-0.654653670708007,0.,-0.755928946018429));
#35869=DIRECTION('',(0.,-0.866025403784438,0.5));
#35870=DIRECTION('',(0.,0.866025403784438,-0.5));
#35871=DIRECTION('center_axis',(0.,-0.983982136481635,-0.178267089180915));
#35872=DIRECTION('ref_axis',(0.,0.178267089180915,-0.983982136481635));
#35873=DIRECTION('',(-1.,0.,0.));
#35874=DIRECTION('',(1.,0.,0.));
#35875=DIRECTION('center_axis',(0.707106781186517,-0.545916630320736,0.449416324513581));
#35876=DIRECTION('ref_axis',(0.536399063209314,0.,-0.843964480880665));
#35877=DIRECTION('',(0.,0.635570661278947,0.77204270252457));
#35878=DIRECTION('',(0.,-0.635570661278947,-0.77204270252457));
#35879=DIRECTION('center_axis',(0.,-0.77204270252457,0.635570661278947));
#35880=DIRECTION('ref_axis',(0.,-0.635570661278947,-0.77204270252457));
#35881=DIRECTION('',(0.,0.635570661278947,0.77204270252457));
#35882=DIRECTION('center_axis',(0.,0.500000000000001,0.866025403784438));
#35883=DIRECTION('ref_axis',(0.,-0.866025403784438,0.500000000000001));
#35884=DIRECTION('',(0.,0.866025403784438,-0.500000000000001));
#35885=DIRECTION('center_axis',(1.,0.,0.));
#35886=DIRECTION('ref_axis',(0.,0.,-1.));
#35887=DIRECTION('center_axis',(0.,-0.5,-0.866025403784438));
#35888=DIRECTION('ref_axis',(0.,0.866025403784438,-0.5));
#35889=DIRECTION('',(0.707106781186529,1.96261557335478E-15,-0.707106781186566));
#35890=DIRECTION('center_axis',(0.,0.,-1.));
#35891=DIRECTION('ref_axis',(1.,0.,0.));
#35892=DIRECTION('',(0.,0.,-1.));
#35893=DIRECTION('center_axis',(0.,0.,-1.));
#35894=DIRECTION('ref_axis',(1.,0.,0.));
#35895=DIRECTION('center_axis',(0.,0.,-1.));
#35896=DIRECTION('ref_axis',(1.,0.,0.));
#35897=DIRECTION('center_axis',(0.,0.,1.));
#35898=DIRECTION('ref_axis',(1.,0.,0.));
#35899=DIRECTION('',(-1.,0.,0.));
#35900=DIRECTION('center_axis',(0.,0.,1.));
#35901=DIRECTION('ref_axis',(1.,0.,0.));
#35902=DIRECTION('',(-1.,0.,0.));
#35903=DIRECTION('center_axis',(0.,0.936441689829928,-0.350823262553198));
#35904=DIRECTION('ref_axis',(0.,0.350823262553198,0.936441689829927));
#35905=DIRECTION('',(0.,-0.350823262553198,-0.936441689829927));
#35906=DIRECTION('center_axis',(1.,0.,0.));
#35907=DIRECTION('ref_axis',(0.,0.,-1.));
#35908=DIRECTION('center_axis',(1.,0.,0.));
#35909=DIRECTION('ref_axis',(0.,0.,-1.));
#35910=DIRECTION('center_axis',(0.,-0.164398987305357,0.986393923832144));
#35911=DIRECTION('ref_axis',(0.,-0.986393923832144,-0.164398987305357));
#35912=DIRECTION('',(0.,0.986393923832144,0.164398987305357));
#35913=DIRECTION('center_axis',(1.,0.,0.));
#35914=DIRECTION('ref_axis',(0.,0.,-1.));
#35915=DIRECTION('center_axis',(1.,0.,0.));
#35916=DIRECTION('ref_axis',(0.,-1.83697019872103E-16,-1.));
#35917=DIRECTION('center_axis',(1.,0.,0.));
#35918=DIRECTION('ref_axis',(0.,0.,-1.));
#35919=DIRECTION('',(-1.,0.,0.));
#35920=DIRECTION('',(-1.,0.,0.));
#35921=DIRECTION('center_axis',(1.,0.,0.));
#35922=DIRECTION('ref_axis',(0.,0.,-1.));
#35923=DIRECTION('axis',(0.,0.,1.));
#35924=DIRECTION('refdir',(1.,0.,0.));
#35925=DIRECTION('center_axis',(1.,0.,0.));
#35926=DIRECTION('ref_axis',(0.,1.,0.));
#35927=DIRECTION('',(-1.,0.,0.));
#35928=DIRECTION('center_axis',(1.,0.,0.));
#35929=DIRECTION('ref_axis',(0.,1.,0.));
#35930=DIRECTION('center_axis',(1.,0.,0.));
#35931=DIRECTION('ref_axis',(0.,1.,0.));
#35932=DIRECTION('',(-1.,0.,0.));
#35933=DIRECTION('center_axis',(1.,0.,0.));
#35934=DIRECTION('ref_axis',(0.,1.,0.));
#35935=DIRECTION('',(-1.,0.,0.));
#35936=DIRECTION('center_axis',(1.,0.,0.));
#35937=DIRECTION('ref_axis',(0.,1.,0.));
#35938=DIRECTION('',(-1.,0.,0.));
#35939=DIRECTION('center_axis',(1.,0.,0.));
#35940=DIRECTION('ref_axis',(0.,1.,0.));
#35941=DIRECTION('',(-1.,0.,0.));
#35942=DIRECTION('center_axis',(1.,0.,0.));
#35943=DIRECTION('ref_axis',(0.,1.,0.));
#35944=DIRECTION('',(-1.,0.,0.));
#35945=DIRECTION('center_axis',(1.,0.,0.));
#35946=DIRECTION('ref_axis',(0.,1.,0.));
#35947=DIRECTION('',(-1.,0.,0.));
#35948=DIRECTION('center_axis',(1.,0.,0.));
#35949=DIRECTION('ref_axis',(0.,1.,0.));
#35950=DIRECTION('',(-1.,0.,0.));
#35951=DIRECTION('center_axis',(1.,0.,0.));
#35952=DIRECTION('ref_axis',(0.,1.,0.));
#35953=DIRECTION('',(-1.,0.,0.));
#35954=DIRECTION('center_axis',(1.,0.,0.));
#35955=DIRECTION('ref_axis',(0.,1.,0.));
#35956=DIRECTION('',(-1.,0.,0.));
#35957=DIRECTION('center_axis',(1.,0.,0.));
#35958=DIRECTION('ref_axis',(0.,1.,0.));
#35959=DIRECTION('',(-1.,0.,0.));
#35960=DIRECTION('center_axis',(1.,0.,0.));
#35961=DIRECTION('ref_axis',(0.,1.,0.));
#35962=DIRECTION('',(-1.,0.,0.));
#35963=DIRECTION('center_axis',(1.,0.,0.));
#35964=DIRECTION('ref_axis',(0.,1.,0.));
#35965=DIRECTION('',(-1.,0.,0.));
#35966=DIRECTION('center_axis',(1.,0.,0.));
#35967=DIRECTION('ref_axis',(0.,1.,0.));
#35968=DIRECTION('',(-1.,0.,0.));
#35969=DIRECTION('center_axis',(1.,0.,0.));
#35970=DIRECTION('ref_axis',(0.,1.,0.));
#35971=DIRECTION('',(-1.,0.,0.));
#35972=DIRECTION('center_axis',(1.,0.,0.));
#35973=DIRECTION('ref_axis',(0.,1.,0.));
#35974=DIRECTION('',(-1.,0.,0.));
#35975=DIRECTION('center_axis',(1.,0.,0.));
#35976=DIRECTION('ref_axis',(0.,1.,0.));
#35977=DIRECTION('',(-1.,0.,0.));
#35978=DIRECTION('center_axis',(1.,0.,0.));
#35979=DIRECTION('ref_axis',(0.,1.,0.));
#35980=DIRECTION('',(-1.,0.,0.));
#35981=DIRECTION('center_axis',(1.,0.,0.));
#35982=DIRECTION('ref_axis',(0.,1.,0.));
#35983=DIRECTION('',(-1.,0.,0.));
#35984=DIRECTION('center_axis',(1.,0.,0.));
#35985=DIRECTION('ref_axis',(0.,1.,0.));
#35986=DIRECTION('',(-1.,0.,0.));
#35987=DIRECTION('center_axis',(1.,0.,0.));
#35988=DIRECTION('ref_axis',(0.,1.,1.18505573263654E-13));
#35989=DIRECTION('',(1.,0.,0.));
#35990=DIRECTION('center_axis',(1.,0.,0.));
#35991=DIRECTION('ref_axis',(0.,1.,1.18505573263654E-13));
#35992=DIRECTION('center_axis',(1.,0.,0.));
#35993=DIRECTION('ref_axis',(0.,1.,1.18505573263654E-13));
#35994=DIRECTION('',(1.,0.,0.));
#35995=DIRECTION('center_axis',(1.,0.,0.));
#35996=DIRECTION('ref_axis',(0.,1.,1.18505573263654E-13));
#35997=DIRECTION('center_axis',(1.,0.,0.));
#35998=DIRECTION('ref_axis',(0.,1.,1.18505573263654E-13));
#35999=DIRECTION('',(1.,0.,0.));
#36000=DIRECTION('center_axis',(1.,0.,0.));
#36001=DIRECTION('ref_axis',(0.,1.,1.18505573263654E-13));
#36002=DIRECTION('',(1.,0.,0.));
#36003=DIRECTION('center_axis',(1.,0.,0.));
#36004=DIRECTION('ref_axis',(0.,1.,1.18505573263654E-13));
#36005=DIRECTION('',(1.,0.,0.));
#36006=DIRECTION('center_axis',(1.,0.,0.));
#36007=DIRECTION('ref_axis',(0.,1.,1.18505573263654E-13));
#36008=DIRECTION('',(1.,0.,0.));
#36009=DIRECTION('center_axis',(1.,0.,0.));
#36010=DIRECTION('ref_axis',(0.,1.,1.18505573263654E-13));
#36011=DIRECTION('',(1.,0.,0.));
#36012=DIRECTION('center_axis',(1.,0.,0.));
#36013=DIRECTION('ref_axis',(0.,1.,1.18505573263654E-13));
#36014=DIRECTION('',(1.,0.,0.));
#36015=DIRECTION('center_axis',(1.,0.,0.));
#36016=DIRECTION('ref_axis',(0.,1.,1.18505573263654E-13));
#36017=DIRECTION('',(1.,0.,0.));
#36018=DIRECTION('center_axis',(1.,0.,0.));
#36019=DIRECTION('ref_axis',(0.,1.,1.18505573263654E-13));
#36020=DIRECTION('',(1.,0.,0.));
#36021=DIRECTION('center_axis',(1.,0.,0.));
#36022=DIRECTION('ref_axis',(0.,1.,1.18505573263654E-13));
#36023=DIRECTION('',(1.,0.,0.));
#36024=DIRECTION('center_axis',(1.,0.,0.));
#36025=DIRECTION('ref_axis',(0.,1.,1.18505573263654E-13));
#36026=DIRECTION('',(1.,0.,0.));
#36027=DIRECTION('center_axis',(1.,0.,0.));
#36028=DIRECTION('ref_axis',(0.,1.,1.18505573263654E-13));
#36029=DIRECTION('',(1.,0.,0.));
#36030=DIRECTION('center_axis',(1.,0.,0.));
#36031=DIRECTION('ref_axis',(0.,1.,1.18505573263654E-13));
#36032=DIRECTION('',(1.,0.,0.));
#36033=DIRECTION('center_axis',(1.,0.,0.));
#36034=DIRECTION('ref_axis',(0.,1.,1.18505573263654E-13));
#36035=DIRECTION('',(1.,0.,0.));
#36036=DIRECTION('center_axis',(1.,0.,0.));
#36037=DIRECTION('ref_axis',(0.,1.,1.18505573263654E-13));
#36038=DIRECTION('',(1.,0.,0.));
#36039=DIRECTION('center_axis',(1.,0.,0.));
#36040=DIRECTION('ref_axis',(0.,1.,1.18505573263654E-13));
#36041=DIRECTION('',(1.,0.,0.));
#36042=DIRECTION('center_axis',(1.,0.,0.));
#36043=DIRECTION('ref_axis',(0.,1.,1.18505573263654E-13));
#36044=DIRECTION('',(1.,0.,0.));
#36045=DIRECTION('center_axis',(1.,0.,0.));
#36046=DIRECTION('ref_axis',(0.,1.,1.18505573263654E-13));
#36047=DIRECTION('',(1.,0.,0.));
#36048=DIRECTION('center_axis',(1.,0.,0.));
#36049=DIRECTION('ref_axis',(0.,1.,1.18505573263654E-13));
#36050=DIRECTION('',(1.,0.,0.));
#36051=DIRECTION('center_axis',(1.,0.,0.));
#36052=DIRECTION('ref_axis',(0.,0.,-1.));
#36053=DIRECTION('center_axis',(1.,0.,0.));
#36054=DIRECTION('ref_axis',(0.,1.,0.));
#36055=DIRECTION('center_axis',(1.,0.,0.));
#36056=DIRECTION('ref_axis',(0.,1.,0.));
#36057=DIRECTION('center_axis',(-1.,0.,0.));
#36058=DIRECTION('ref_axis',(0.,1.,1.18505573263654E-13));
#36059=DIRECTION('center_axis',(1.,0.,0.));
#36060=DIRECTION('ref_axis',(0.,1.,1.18505573263654E-13));
#36061=DIRECTION('center_axis',(-1.,0.,0.));
#36062=DIRECTION('ref_axis',(0.,1.,0.));
#36063=DIRECTION('',(0.500438231481872,0.865772242839476,1.06026520598399E-16));
#36064=DIRECTION('center_axis',(1.,0.,0.));
#36065=DIRECTION('ref_axis',(0.,1.,0.));
#36066=DIRECTION('center_axis',(0.,-0.5,0.866025403784439));
#36067=DIRECTION('ref_axis',(0.,-0.866025403784439,-0.5));
#36068=DIRECTION('',(1.,0.,0.));
#36069=DIRECTION('',(0.,-0.866025403784439,-0.5));
#36070=DIRECTION('',(1.,0.,0.));
#36071=DIRECTION('center_axis',(0.,0.5,0.866025403784439));
#36072=DIRECTION('ref_axis',(0.,-0.866025403784439,0.5));
#36073=DIRECTION('',(1.,0.,0.));
#36074=DIRECTION('',(0.,-0.866025403784439,0.5));
#36075=DIRECTION('center_axis',(0.,1.,-3.60555503696918E-16));
#36076=DIRECTION('ref_axis',(0.,3.60555503696918E-16,1.));
#36077=DIRECTION('',(1.,0.,0.));
#36078=DIRECTION('',(0.,3.60555503696918E-16,1.));
#36079=DIRECTION('center_axis',(1.,0.,0.));
#36080=DIRECTION('ref_axis',(0.,0.,-1.));
#36081=DIRECTION('',(0.,0.866025403784439,0.5));
#36082=DIRECTION('',(0.,0.866025403784439,-0.5));
#36083=DIRECTION('',(0.,1.20185167898973E-16,-1.));
#36084=DIRECTION('center_axis',(-1.,0.,0.));
#36085=DIRECTION('ref_axis',(0.,1.,0.));
#36086=DIRECTION('center_axis',(0.,0.5,-0.866025403784439));
#36087=DIRECTION('ref_axis',(0.,0.866025403784439,0.5));
#36088=DIRECTION('',(1.,0.,0.));
#36089=DIRECTION('center_axis',(0.,-0.5,-0.866025403784439));
#36090=DIRECTION('ref_axis',(0.,0.866025403784439,-0.5));
#36091=DIRECTION('',(1.,0.,0.));
#36092=DIRECTION('center_axis',(0.,-1.,-1.20185167898973E-16));
#36093=DIRECTION('ref_axis',(0.,1.20185167898973E-16,-1.));
#36094=DIRECTION('center_axis',(1.,0.,0.));
#36095=DIRECTION('ref_axis',(0.,0.,-1.));
#36096=DIRECTION('center_axis',(-1.,0.,0.));
#36097=DIRECTION('ref_axis',(0.,0.,1.));
#36098=DIRECTION('center_axis',(1.,0.,0.));
#36099=DIRECTION('ref_axis',(0.,0.,-1.));
#36100=DIRECTION('center_axis',(1.,0.,0.));
#36101=DIRECTION('ref_axis',(0.,1.,0.));
#36102=DIRECTION('',(-0.707106781186546,0.707106781186549,8.65956056235495E-17));
#36103=DIRECTION('center_axis',(1.,0.,0.));
#36104=DIRECTION('ref_axis',(0.,1.,0.));
#36105=DIRECTION('axis',(0.,0.,1.));
#36106=DIRECTION('refdir',(1.,0.,0.));
#36107=DIRECTION('center_axis',(1.,0.,0.));
#36108=DIRECTION('ref_axis',(0.,1.,0.));
#36109=DIRECTION('',(-1.,0.,0.));
#36110=DIRECTION('center_axis',(1.,0.,0.));
#36111=DIRECTION('ref_axis',(0.,1.,0.));
#36112=DIRECTION('center_axis',(1.,0.,0.));
#36113=DIRECTION('ref_axis',(0.,1.,0.));
#36114=DIRECTION('',(-1.,0.,0.));
#36115=DIRECTION('center_axis',(1.,0.,0.));
#36116=DIRECTION('ref_axis',(0.,1.,0.));
#36117=DIRECTION('',(-1.,0.,0.));
#36118=DIRECTION('center_axis',(1.,0.,0.));
#36119=DIRECTION('ref_axis',(0.,1.,0.));
#36120=DIRECTION('',(-1.,0.,0.));
#36121=DIRECTION('center_axis',(1.,0.,0.));
#36122=DIRECTION('ref_axis',(0.,1.,0.));
#36123=DIRECTION('',(-1.,0.,0.));
#36124=DIRECTION('center_axis',(1.,0.,0.));
#36125=DIRECTION('ref_axis',(0.,1.,0.));
#36126=DIRECTION('',(-1.,0.,0.));
#36127=DIRECTION('center_axis',(1.,0.,0.));
#36128=DIRECTION('ref_axis',(0.,1.,0.));
#36129=DIRECTION('',(-1.,0.,0.));
#36130=DIRECTION('center_axis',(1.,0.,0.));
#36131=DIRECTION('ref_axis',(0.,1.,0.));
#36132=DIRECTION('',(-1.,0.,0.));
#36133=DIRECTION('center_axis',(1.,0.,0.));
#36134=DIRECTION('ref_axis',(0.,1.,0.));
#36135=DIRECTION('',(-1.,0.,0.));
#36136=DIRECTION('center_axis',(1.,0.,0.));
#36137=DIRECTION('ref_axis',(0.,1.,0.));
#36138=DIRECTION('',(-1.,0.,0.));
#36139=DIRECTION('center_axis',(1.,0.,0.));
#36140=DIRECTION('ref_axis',(0.,1.,0.));
#36141=DIRECTION('',(-1.,0.,0.));
#36142=DIRECTION('center_axis',(1.,0.,0.));
#36143=DIRECTION('ref_axis',(0.,1.,0.));
#36144=DIRECTION('',(-1.,0.,0.));
#36145=DIRECTION('center_axis',(1.,0.,0.));
#36146=DIRECTION('ref_axis',(0.,1.,0.));
#36147=DIRECTION('',(-1.,0.,0.));
#36148=DIRECTION('center_axis',(1.,0.,0.));
#36149=DIRECTION('ref_axis',(0.,1.,0.));
#36150=DIRECTION('',(-1.,0.,0.));
#36151=DIRECTION('center_axis',(1.,0.,0.));
#36152=DIRECTION('ref_axis',(0.,1.,0.));
#36153=DIRECTION('',(-1.,0.,0.));
#36154=DIRECTION('center_axis',(1.,0.,0.));
#36155=DIRECTION('ref_axis',(0.,1.,0.));
#36156=DIRECTION('',(-1.,0.,0.));
#36157=DIRECTION('center_axis',(1.,0.,0.));
#36158=DIRECTION('ref_axis',(0.,1.,0.));
#36159=DIRECTION('',(-1.,0.,0.));
#36160=DIRECTION('center_axis',(1.,0.,0.));
#36161=DIRECTION('ref_axis',(0.,1.,0.));
#36162=DIRECTION('',(-1.,0.,0.));
#36163=DIRECTION('center_axis',(1.,0.,0.));
#36164=DIRECTION('ref_axis',(0.,1.,0.));
#36165=DIRECTION('',(-1.,0.,0.));
#36166=DIRECTION('center_axis',(1.,0.,0.));
#36167=DIRECTION('ref_axis',(0.,1.,0.));
#36168=DIRECTION('',(-1.,0.,0.));
#36169=DIRECTION('center_axis',(1.,0.,0.));
#36170=DIRECTION('ref_axis',(0.,1.,1.18505573263654E-13));
#36171=DIRECTION('',(1.,0.,0.));
#36172=DIRECTION('center_axis',(1.,0.,0.));
#36173=DIRECTION('ref_axis',(0.,1.,1.18505573263654E-13));
#36174=DIRECTION('center_axis',(1.,0.,0.));
#36175=DIRECTION('ref_axis',(0.,1.,1.18505573263654E-13));
#36176=DIRECTION('',(1.,0.,0.));
#36177=DIRECTION('center_axis',(1.,0.,0.));
#36178=DIRECTION('ref_axis',(0.,1.,1.18505573263654E-13));
#36179=DIRECTION('center_axis',(1.,0.,0.));
#36180=DIRECTION('ref_axis',(0.,1.,1.18505573263654E-13));
#36181=DIRECTION('',(1.,0.,0.));
#36182=DIRECTION('center_axis',(1.,0.,0.));
#36183=DIRECTION('ref_axis',(0.,1.,1.18505573263654E-13));
#36184=DIRECTION('',(1.,0.,0.));
#36185=DIRECTION('center_axis',(1.,0.,0.));
#36186=DIRECTION('ref_axis',(0.,1.,1.18505573263654E-13));
#36187=DIRECTION('',(1.,0.,0.));
#36188=DIRECTION('center_axis',(1.,0.,0.));
#36189=DIRECTION('ref_axis',(0.,1.,1.18505573263654E-13));
#36190=DIRECTION('',(1.,0.,0.));
#36191=DIRECTION('center_axis',(1.,0.,0.));
#36192=DIRECTION('ref_axis',(0.,1.,1.18505573263654E-13));
#36193=DIRECTION('',(1.,0.,0.));
#36194=DIRECTION('center_axis',(1.,0.,0.));
#36195=DIRECTION('ref_axis',(0.,1.,1.18505573263654E-13));
#36196=DIRECTION('',(1.,0.,0.));
#36197=DIRECTION('center_axis',(1.,0.,0.));
#36198=DIRECTION('ref_axis',(0.,1.,1.18505573263654E-13));
#36199=DIRECTION('',(1.,0.,0.));
#36200=DIRECTION('center_axis',(1.,0.,0.));
#36201=DIRECTION('ref_axis',(0.,1.,1.18505573263654E-13));
#36202=DIRECTION('',(1.,0.,0.));
#36203=DIRECTION('center_axis',(1.,0.,0.));
#36204=DIRECTION('ref_axis',(0.,1.,1.18505573263654E-13));
#36205=DIRECTION('',(1.,0.,0.));
#36206=DIRECTION('center_axis',(1.,0.,0.));
#36207=DIRECTION('ref_axis',(0.,1.,1.18505573263654E-13));
#36208=DIRECTION('',(1.,0.,0.));
#36209=DIRECTION('center_axis',(1.,0.,0.));
#36210=DIRECTION('ref_axis',(0.,1.,1.18505573263654E-13));
#36211=DIRECTION('',(1.,0.,0.));
#36212=DIRECTION('center_axis',(1.,0.,0.));
#36213=DIRECTION('ref_axis',(0.,1.,1.18505573263654E-13));
#36214=DIRECTION('',(1.,0.,0.));
#36215=DIRECTION('center_axis',(1.,0.,0.));
#36216=DIRECTION('ref_axis',(0.,1.,1.18505573263654E-13));
#36217=DIRECTION('',(1.,0.,0.));
#36218=DIRECTION('center_axis',(1.,0.,0.));
#36219=DIRECTION('ref_axis',(0.,1.,1.18505573263654E-13));
#36220=DIRECTION('',(1.,0.,0.));
#36221=DIRECTION('center_axis',(1.,0.,0.));
#36222=DIRECTION('ref_axis',(0.,1.,1.18505573263654E-13));
#36223=DIRECTION('',(1.,0.,0.));
#36224=DIRECTION('center_axis',(1.,0.,0.));
#36225=DIRECTION('ref_axis',(0.,1.,1.18505573263654E-13));
#36226=DIRECTION('',(1.,0.,0.));
#36227=DIRECTION('center_axis',(1.,0.,0.));
#36228=DIRECTION('ref_axis',(0.,1.,1.18505573263654E-13));
#36229=DIRECTION('',(1.,0.,0.));
#36230=DIRECTION('center_axis',(1.,0.,0.));
#36231=DIRECTION('ref_axis',(0.,1.,1.18505573263654E-13));
#36232=DIRECTION('',(1.,0.,0.));
#36233=DIRECTION('center_axis',(1.,0.,0.));
#36234=DIRECTION('ref_axis',(0.,0.,-1.));
#36235=DIRECTION('center_axis',(1.,0.,0.));
#36236=DIRECTION('ref_axis',(0.,1.,0.));
#36237=DIRECTION('center_axis',(1.,0.,0.));
#36238=DIRECTION('ref_axis',(0.,1.,0.));
#36239=DIRECTION('center_axis',(-1.,0.,0.));
#36240=DIRECTION('ref_axis',(0.,1.,1.18505573263654E-13));
#36241=DIRECTION('center_axis',(1.,0.,0.));
#36242=DIRECTION('ref_axis',(0.,1.,1.18505573263654E-13));
#36243=DIRECTION('center_axis',(0.,-0.451966109673778,0.892035109009926));
#36244=DIRECTION('ref_axis',(0.,-0.892035109009926,-0.451966109673778));
#36245=DIRECTION('',(-1.,0.,0.));
#36246=DIRECTION('',(0.,-0.892035109009926,-0.451966109673778));
#36247=DIRECTION('',(1.,0.,0.));
#36248=DIRECTION('',(0.,-0.892035109009926,-0.451966109673778));
#36249=DIRECTION('center_axis',(1.,0.,0.));
#36250=DIRECTION('ref_axis',(0.,-0.17364817766693,-0.984807753012208));
#36251=DIRECTION('center_axis',(-1.,0.,0.));
#36252=DIRECTION('ref_axis',(0.,1.,0.));
#36253=DIRECTION('',(0.,0.68365729580961,-0.729803193940867));
#36254=DIRECTION('center_axis',(0.,-0.729803193940867,-0.683657295809611));
#36255=DIRECTION('ref_axis',(0.,0.68365729580961,-0.729803193940867));
#36256=DIRECTION('',(1.,0.,0.));
#36257=DIRECTION('',(0.,0.68365729580961,-0.729803193940867));
#36258=DIRECTION('center_axis',(1.,0.,0.));
#36259=DIRECTION('ref_axis',(0.,-0.17364817766693,-0.984807753012208));
#36260=DIRECTION('center_axis',(1.,0.,0.));
#36261=DIRECTION('ref_axis',(0.,1.,0.));
#36262=DIRECTION('center_axis',(0.,-0.290199457811006,0.956966182624129));
#36263=DIRECTION('ref_axis',(0.,-0.956966182624129,-0.290199457811006));
#36264=DIRECTION('',(-1.,0.,0.));
#36265=DIRECTION('',(0.,-0.956966182624129,-0.290199457811006));
#36266=DIRECTION('',(1.,0.,0.));
#36267=DIRECTION('',(0.,-0.956966182624129,-0.290199457811006));
#36268=DIRECTION('center_axis',(1.,0.,0.));
#36269=DIRECTION('ref_axis',(0.,-0.342020143325669,-0.939692620785908));
#36270=DIRECTION('center_axis',(-1.,0.,0.));
#36271=DIRECTION('ref_axis',(0.,1.,0.));
#36272=DIRECTION('',(0.,0.546542010633327,-0.837431687132079));
#36273=DIRECTION('center_axis',(0.,-0.837431687132079,-0.546542010633327));
#36274=DIRECTION('ref_axis',(0.,0.546542010633327,-0.837431687132079));
#36275=DIRECTION('',(1.,0.,0.));
#36276=DIRECTION('',(0.,0.546542010633327,-0.837431687132079));
#36277=DIRECTION('center_axis',(1.,0.,0.));
#36278=DIRECTION('ref_axis',(0.,-0.342020143325669,-0.939692620785908));
#36279=DIRECTION('center_axis',(1.,0.,0.));
#36280=DIRECTION('ref_axis',(0.,1.,0.));
#36281=DIRECTION('center_axis',(0.,-0.11961524227066,0.992820323027551));
#36282=DIRECTION('ref_axis',(0.,-0.992820323027551,-0.11961524227066));
#36283=DIRECTION('',(-1.,0.,0.));
#36284=DIRECTION('',(0.,-0.992820323027551,-0.11961524227066));
#36285=DIRECTION('',(1.,0.,0.));
#36286=DIRECTION('',(0.,-0.992820323027551,-0.11961524227066));
#36287=DIRECTION('center_axis',(1.,0.,0.));
#36288=DIRECTION('ref_axis',(0.,-0.5,-0.866025403784438));
#36289=DIRECTION('center_axis',(-1.,0.,0.));
#36290=DIRECTION('ref_axis',(0.,1.,0.));
#36291=DIRECTION('',(0.,0.392820323027553,-0.919615242270662));
#36292=DIRECTION('center_axis',(0.,-0.919615242270662,-0.392820323027553));
#36293=DIRECTION('ref_axis',(0.,0.392820323027553,-0.919615242270662));
#36294=DIRECTION('',(1.,0.,0.));
#36295=DIRECTION('',(0.,0.392820323027553,-0.919615242270662));
#36296=DIRECTION('center_axis',(1.,0.,0.));
#36297=DIRECTION('ref_axis',(0.,-0.5,-0.866025403784438));
#36298=DIRECTION('center_axis',(1.,0.,0.));
#36299=DIRECTION('ref_axis',(0.,1.,0.));
#36300=DIRECTION('center_axis',(0.,0.0546034218778482,0.998508120307106));
#36301=DIRECTION('ref_axis',(0.,-0.998508120307106,0.0546034218778482));
#36302=DIRECTION('',(-1.,0.,0.));
#36303=DIRECTION('',(0.,-0.998508120307106,0.0546034218778482));
#36304=DIRECTION('',(1.,0.,0.));
#36305=DIRECTION('',(0.,-0.998508120307106,0.0546034218778482));
#36306=DIRECTION('center_axis',(1.,0.,0.));
#36307=DIRECTION('ref_axis',(0.,-0.64278760968654,-0.766044443118978));
#36308=DIRECTION('center_axis',(-1.,0.,0.));
#36309=DIRECTION('ref_axis',(0.,1.,0.));
#36310=DIRECTION('',(0.,0.227162988683261,-0.973856753620618));
#36311=DIRECTION('center_axis',(0.,-0.973856753620618,-0.227162988683262));
#36312=DIRECTION('ref_axis',(0.,0.227162988683261,-0.973856753620618));
#36313=DIRECTION('',(1.,0.,0.));
#36314=DIRECTION('',(0.,0.227162988683261,-0.973856753620618));
#36315=DIRECTION('center_axis',(1.,0.,0.));
#36316=DIRECTION('ref_axis',(0.,-0.64278760968654,-0.766044443118978));
#36317=DIRECTION('center_axis',(1.,0.,0.));
#36318=DIRECTION('ref_axis',(0.,1.,0.));
#36319=DIRECTION('center_axis',(0.,0.227162988683262,0.973856753620618));
#36320=DIRECTION('ref_axis',(0.,-0.973856753620618,0.227162988683262));
#36321=DIRECTION('',(-1.,0.,0.));
#36322=DIRECTION('',(0.,-0.973856753620618,0.227162988683262));
#36323=DIRECTION('',(1.,0.,0.));
#36324=DIRECTION('',(0.,-0.973856753620618,0.227162988683262));
#36325=DIRECTION('center_axis',(1.,0.,0.));
#36326=DIRECTION('ref_axis',(0.,-0.766044443118978,-0.642787609686539));
#36327=DIRECTION('center_axis',(-1.,0.,0.));
#36328=DIRECTION('ref_axis',(0.,1.,0.));
#36329=DIRECTION('',(0.,0.0546034218778476,-0.998508120307106));
#36330=DIRECTION('center_axis',(0.,-0.998508120307106,-0.0546034218778476));
#36331=DIRECTION('ref_axis',(0.,0.0546034218778476,-0.998508120307106));
#36332=DIRECTION('',(1.,0.,0.));
#36333=DIRECTION('',(0.,0.0546034218778476,-0.998508120307106));
#36334=DIRECTION('center_axis',(1.,0.,0.));
#36335=DIRECTION('ref_axis',(0.,-0.766044443118978,-0.642787609686539));
#36336=DIRECTION('center_axis',(1.,0.,0.));
#36337=DIRECTION('ref_axis',(0.,1.,0.));
#36338=DIRECTION('center_axis',(0.,0.392820323027554,0.919615242270662));
#36339=DIRECTION('ref_axis',(0.,-0.919615242270662,0.392820323027554));
#36340=DIRECTION('',(-1.,0.,0.));
#36341=DIRECTION('',(0.,-0.919615242270662,0.392820323027554));
#36342=DIRECTION('',(1.,0.,0.));
#36343=DIRECTION('',(0.,-0.919615242270662,0.392820323027554));
#36344=DIRECTION('center_axis',(1.,0.,0.));
#36345=DIRECTION('ref_axis',(0.,-0.866025403784439,-0.5));
#36346=DIRECTION('center_axis',(-1.,0.,0.));
#36347=DIRECTION('ref_axis',(0.,1.,0.));
#36348=DIRECTION('',(0.,-0.11961524227066,-0.992820323027551));
#36349=DIRECTION('center_axis',(0.,-0.992820323027551,0.11961524227066));
#36350=DIRECTION('ref_axis',(0.,-0.11961524227066,-0.992820323027551));
#36351=DIRECTION('',(1.,0.,0.));
#36352=DIRECTION('',(0.,-0.11961524227066,-0.992820323027551));
#36353=DIRECTION('center_axis',(1.,0.,0.));
#36354=DIRECTION('ref_axis',(0.,-0.866025403784439,-0.5));
#36355=DIRECTION('center_axis',(1.,0.,0.));
#36356=DIRECTION('ref_axis',(0.,1.,0.));
#36357=DIRECTION('center_axis',(0.,0.546542010633329,0.837431687132078));
#36358=DIRECTION('ref_axis',(0.,-0.837431687132078,0.546542010633329));
#36359=DIRECTION('',(-1.,0.,0.));
#36360=DIRECTION('',(0.,-0.837431687132078,0.546542010633329));
#36361=DIRECTION('',(1.,0.,0.));
#36362=DIRECTION('',(0.,-0.837431687132078,0.546542010633329));
#36363=DIRECTION('center_axis',(1.,0.,0.));
#36364=DIRECTION('ref_axis',(0.,-0.939692620785909,-0.342020143325668));
#36365=DIRECTION('center_axis',(-1.,0.,0.));
#36366=DIRECTION('ref_axis',(0.,1.,0.));
#36367=DIRECTION('',(0.,-0.290199457811008,-0.956966182624129));
#36368=DIRECTION('center_axis',(0.,-0.956966182624129,0.290199457811008));
#36369=DIRECTION('ref_axis',(0.,-0.290199457811008,-0.956966182624129));
#36370=DIRECTION('',(1.,0.,0.));
#36371=DIRECTION('',(0.,-0.290199457811008,-0.956966182624129));
#36372=DIRECTION('center_axis',(1.,0.,0.));
#36373=DIRECTION('ref_axis',(0.,-0.939692620785909,-0.342020143325668));
#36374=DIRECTION('center_axis',(1.,0.,0.));
#36375=DIRECTION('ref_axis',(0.,1.,0.));
#36376=DIRECTION('center_axis',(0.,0.683657295809611,0.729803193940867));
#36377=DIRECTION('ref_axis',(0.,-0.729803193940867,0.683657295809611));
#36378=DIRECTION('',(-1.,0.,0.));
#36379=DIRECTION('',(0.,-0.729803193940867,0.683657295809611));
#36380=DIRECTION('',(1.,0.,0.));
#36381=DIRECTION('',(0.,-0.729803193940867,0.683657295809611));
#36382=DIRECTION('center_axis',(1.,0.,0.));
#36383=DIRECTION('ref_axis',(0.,-0.984807753012208,-0.17364817766693));
#36384=DIRECTION('center_axis',(-1.,0.,0.));
#36385=DIRECTION('ref_axis',(0.,1.,0.));
#36386=DIRECTION('',(0.,-0.451966109673778,-0.892035109009926));
#36387=DIRECTION('center_axis',(0.,-0.892035109009926,0.451966109673778));
#36388=DIRECTION('ref_axis',(0.,-0.451966109673778,-0.892035109009926));
#36389=DIRECTION('',(1.,0.,0.));
#36390=DIRECTION('',(0.,-0.451966109673778,-0.892035109009926));
#36391=DIRECTION('center_axis',(1.,0.,0.));
#36392=DIRECTION('ref_axis',(0.,-0.984807753012208,-0.17364817766693));
#36393=DIRECTION('center_axis',(1.,0.,0.));
#36394=DIRECTION('ref_axis',(0.,1.,0.));
#36395=DIRECTION('center_axis',(0.,0.800000000000002,0.599999999999997));
#36396=DIRECTION('ref_axis',(0.,-0.599999999999997,0.800000000000002));
#36397=DIRECTION('',(-1.,0.,0.));
#36398=DIRECTION('',(0.,-0.599999999999997,0.800000000000002));
#36399=DIRECTION('',(1.,0.,0.));
#36400=DIRECTION('',(0.,-0.599999999999997,0.800000000000002));
#36401=DIRECTION('center_axis',(1.,0.,0.));
#36402=DIRECTION('ref_axis',(0.,-1.,1.83697019872103E-16));
#36403=DIRECTION('center_axis',(-1.,0.,0.));
#36404=DIRECTION('ref_axis',(0.,1.,0.));
#36405=DIRECTION('',(0.,-0.599999999999998,-0.800000000000002));
#36406=DIRECTION('center_axis',(0.,-0.800000000000002,0.599999999999998));
#36407=DIRECTION('ref_axis',(0.,-0.599999999999998,-0.800000000000002));
#36408=DIRECTION('',(1.,0.,0.));
#36409=DIRECTION('',(0.,-0.599999999999998,-0.800000000000002));
#36410=DIRECTION('center_axis',(1.,0.,0.));
#36411=DIRECTION('ref_axis',(0.,-1.,1.83697019872103E-16));
#36412=DIRECTION('center_axis',(1.,0.,0.));
#36413=DIRECTION('ref_axis',(0.,1.,0.));
#36414=DIRECTION('center_axis',(0.,0.892035109009926,0.451966109673778));
#36415=DIRECTION('ref_axis',(0.,-0.451966109673778,0.892035109009926));
#36416=DIRECTION('',(-1.,0.,0.));
#36417=DIRECTION('',(0.,-0.451966109673778,0.892035109009926));
#36418=DIRECTION('',(1.,0.,0.));
#36419=DIRECTION('',(0.,-0.451966109673778,0.892035109009926));
#36420=DIRECTION('center_axis',(1.,0.,0.));
#36421=DIRECTION('ref_axis',(0.,-0.984807753012208,0.17364817766693));
#36422=DIRECTION('center_axis',(-1.,0.,0.));
#36423=DIRECTION('ref_axis',(0.,1.,0.));
#36424=DIRECTION('',(0.,-0.729803193940867,-0.683657295809611));
#36425=DIRECTION('center_axis',(0.,-0.683657295809611,0.729803193940867));
#36426=DIRECTION('ref_axis',(0.,-0.729803193940867,-0.683657295809611));
#36427=DIRECTION('',(1.,0.,0.));
#36428=DIRECTION('',(0.,-0.729803193940867,-0.683657295809611));
#36429=DIRECTION('center_axis',(1.,0.,0.));
#36430=DIRECTION('ref_axis',(0.,-0.984807753012208,0.17364817766693));
#36431=DIRECTION('center_axis',(1.,0.,0.));
#36432=DIRECTION('ref_axis',(0.,1.,0.));
#36433=DIRECTION('center_axis',(0.,0.956966182624129,0.290199457811006));
#36434=DIRECTION('ref_axis',(0.,-0.290199457811006,0.956966182624129));
#36435=DIRECTION('',(-1.,0.,0.));
#36436=DIRECTION('',(0.,-0.290199457811006,0.956966182624129));
#36437=DIRECTION('',(1.,0.,0.));
#36438=DIRECTION('',(0.,-0.290199457811006,0.956966182624129));
#36439=DIRECTION('center_axis',(1.,0.,0.));
#36440=DIRECTION('ref_axis',(0.,-0.939692620785908,0.342020143325669));
#36441=DIRECTION('center_axis',(-1.,0.,0.));
#36442=DIRECTION('ref_axis',(0.,1.,0.));
#36443=DIRECTION('',(0.,-0.837431687132079,-0.546542010633328));
#36444=DIRECTION('center_axis',(0.,-0.546542010633328,0.837431687132079));
#36445=DIRECTION('ref_axis',(0.,-0.837431687132079,-0.546542010633328));
#36446=DIRECTION('',(1.,0.,0.));
#36447=DIRECTION('',(0.,-0.837431687132079,-0.546542010633328));
#36448=DIRECTION('center_axis',(1.,0.,0.));
#36449=DIRECTION('ref_axis',(0.,-0.939692620785908,0.342020143325669));
#36450=DIRECTION('center_axis',(1.,0.,0.));
#36451=DIRECTION('ref_axis',(0.,1.,0.));
#36452=DIRECTION('center_axis',(0.,0.992820323027551,0.11961524227066));
#36453=DIRECTION('ref_axis',(0.,-0.11961524227066,0.992820323027551));
#36454=DIRECTION('',(-1.,0.,0.));
#36455=DIRECTION('',(0.,-0.11961524227066,0.992820323027551));
#36456=DIRECTION('',(1.,0.,0.));
#36457=DIRECTION('',(0.,-0.11961524227066,0.992820323027551));
#36458=DIRECTION('center_axis',(1.,0.,0.));
#36459=DIRECTION('ref_axis',(0.,-0.866025403784438,0.5));
#36460=DIRECTION('center_axis',(-1.,0.,0.));
#36461=DIRECTION('ref_axis',(0.,1.,0.));
#36462=DIRECTION('',(0.,-0.919615242270662,-0.392820323027553));
#36463=DIRECTION('center_axis',(0.,-0.392820323027553,0.919615242270662));
#36464=DIRECTION('ref_axis',(0.,-0.919615242270662,-0.392820323027553));
#36465=DIRECTION('',(1.,0.,0.));
#36466=DIRECTION('',(0.,-0.919615242270662,-0.392820323027553));
#36467=DIRECTION('center_axis',(1.,0.,0.));
#36468=DIRECTION('ref_axis',(0.,-0.866025403784438,0.5));
#36469=DIRECTION('center_axis',(1.,0.,0.));
#36470=DIRECTION('ref_axis',(0.,1.,0.));
#36471=DIRECTION('center_axis',(0.,0.998508120307106,-0.054603421877848));
#36472=DIRECTION('ref_axis',(0.,0.054603421877848,0.998508120307106));
#36473=DIRECTION('',(-1.,0.,0.));
#36474=DIRECTION('',(0.,0.054603421877848,0.998508120307106));
#36475=DIRECTION('',(1.,0.,0.));
#36476=DIRECTION('',(0.,0.054603421877848,0.998508120307106));
#36477=DIRECTION('center_axis',(1.,0.,0.));
#36478=DIRECTION('ref_axis',(0.,-0.766044443118978,0.642787609686539));
#36479=DIRECTION('center_axis',(-1.,0.,0.));
#36480=DIRECTION('ref_axis',(0.,1.,0.));
#36481=DIRECTION('',(0.,-0.973856753620618,-0.227162988683262));
#36482=DIRECTION('center_axis',(0.,-0.227162988683262,0.973856753620618));
#36483=DIRECTION('ref_axis',(0.,-0.973856753620618,-0.227162988683262));
#36484=DIRECTION('',(1.,0.,0.));
#36485=DIRECTION('',(0.,-0.973856753620618,-0.227162988683262));
#36486=DIRECTION('center_axis',(1.,0.,0.));
#36487=DIRECTION('ref_axis',(0.,-0.766044443118978,0.642787609686539));
#36488=DIRECTION('center_axis',(1.,0.,0.));
#36489=DIRECTION('ref_axis',(0.,1.,0.));
#36490=DIRECTION('center_axis',(0.,0.973856753620618,-0.227162988683262));
#36491=DIRECTION('ref_axis',(0.,0.227162988683262,0.973856753620618));
#36492=DIRECTION('',(-1.,0.,0.));
#36493=DIRECTION('',(0.,0.227162988683262,0.973856753620618));
#36494=DIRECTION('',(1.,0.,0.));
#36495=DIRECTION('',(0.,0.227162988683262,0.973856753620618));
#36496=DIRECTION('center_axis',(1.,0.,0.));
#36497=DIRECTION('ref_axis',(0.,-0.642787609686539,0.766044443118978));
#36498=DIRECTION('center_axis',(-1.,0.,0.));
#36499=DIRECTION('ref_axis',(0.,1.,0.));
#36500=DIRECTION('',(0.,-0.998508120307106,-0.0546034218778477));
#36501=DIRECTION('center_axis',(0.,-0.0546034218778477,0.998508120307106));
#36502=DIRECTION('ref_axis',(0.,-0.998508120307106,-0.0546034218778477));
#36503=DIRECTION('',(1.,0.,0.));
#36504=DIRECTION('',(0.,-0.998508120307106,-0.0546034218778477));
#36505=DIRECTION('center_axis',(1.,0.,0.));
#36506=DIRECTION('ref_axis',(0.,-0.642787609686539,0.766044443118978));
#36507=DIRECTION('center_axis',(1.,0.,0.));
#36508=DIRECTION('ref_axis',(0.,1.,0.));
#36509=DIRECTION('center_axis',(0.,0.919615242270662,-0.392820323027554));
#36510=DIRECTION('ref_axis',(0.,0.392820323027554,0.919615242270662));
#36511=DIRECTION('',(-1.,0.,0.));
#36512=DIRECTION('',(0.,0.392820323027554,0.919615242270662));
#36513=DIRECTION('',(1.,0.,0.));
#36514=DIRECTION('',(0.,0.392820323027554,0.919615242270662));
#36515=DIRECTION('center_axis',(1.,0.,0.));
#36516=DIRECTION('ref_axis',(0.,-0.5,0.866025403784439));
#36517=DIRECTION('center_axis',(-1.,0.,0.));
#36518=DIRECTION('ref_axis',(0.,1.,0.));
#36519=DIRECTION('',(0.,-0.992820323027551,0.11961524227066));
#36520=DIRECTION('center_axis',(0.,0.11961524227066,0.992820323027551));
#36521=DIRECTION('ref_axis',(0.,-0.992820323027551,0.11961524227066));
#36522=DIRECTION('',(1.,0.,0.));
#36523=DIRECTION('',(0.,-0.992820323027551,0.11961524227066));
#36524=DIRECTION('center_axis',(1.,0.,0.));
#36525=DIRECTION('ref_axis',(0.,-0.5,0.866025403784439));
#36526=DIRECTION('center_axis',(1.,0.,0.));
#36527=DIRECTION('ref_axis',(0.,1.,0.));
#36528=DIRECTION('center_axis',(0.,0.837431687132078,-0.546542010633328));
#36529=DIRECTION('ref_axis',(0.,0.546542010633328,0.837431687132078));
#36530=DIRECTION('',(-1.,0.,0.));
#36531=DIRECTION('',(0.,0.546542010633328,0.837431687132078));
#36532=DIRECTION('',(1.,0.,0.));
#36533=DIRECTION('',(0.,0.546542010633328,0.837431687132078));
#36534=DIRECTION('center_axis',(1.,0.,0.));
#36535=DIRECTION('ref_axis',(0.,-0.342020143325669,0.939692620785909));
#36536=DIRECTION('center_axis',(-1.,0.,0.));
#36537=DIRECTION('ref_axis',(0.,1.,0.));
#36538=DIRECTION('',(0.,-0.956966182624129,0.290199457811007));
#36539=DIRECTION('center_axis',(0.,0.290199457811007,0.956966182624129));
#36540=DIRECTION('ref_axis',(0.,-0.956966182624129,0.290199457811007));
#36541=DIRECTION('',(1.,0.,0.));
#36542=DIRECTION('',(0.,-0.956966182624129,0.290199457811007));
#36543=DIRECTION('center_axis',(1.,0.,0.));
#36544=DIRECTION('ref_axis',(0.,-0.342020143325669,0.939692620785909));
#36545=DIRECTION('center_axis',(1.,0.,0.));
#36546=DIRECTION('ref_axis',(0.,1.,0.));
#36547=DIRECTION('center_axis',(0.,0.729803193940867,-0.683657295809611));
#36548=DIRECTION('ref_axis',(0.,0.683657295809611,0.729803193940867));
#36549=DIRECTION('',(-1.,0.,0.));
#36550=DIRECTION('',(0.,0.683657295809611,0.729803193940867));
#36551=DIRECTION('',(1.,0.,0.));
#36552=DIRECTION('',(0.,0.683657295809611,0.729803193940867));
#36553=DIRECTION('center_axis',(1.,0.,0.));
#36554=DIRECTION('ref_axis',(0.,-0.17364817766693,0.984807753012208));
#36555=DIRECTION('center_axis',(-1.,0.,0.));
#36556=DIRECTION('ref_axis',(0.,1.,0.));
#36557=DIRECTION('',(0.,-0.892035109009926,0.451966109673778));
#36558=DIRECTION('center_axis',(0.,0.451966109673778,0.892035109009926));
#36559=DIRECTION('ref_axis',(0.,-0.892035109009926,0.451966109673778));
#36560=DIRECTION('',(1.,0.,0.));
#36561=DIRECTION('',(0.,-0.892035109009926,0.451966109673778));
#36562=DIRECTION('center_axis',(1.,0.,0.));
#36563=DIRECTION('ref_axis',(0.,-0.17364817766693,0.984807753012208));
#36564=DIRECTION('center_axis',(1.,0.,0.));
#36565=DIRECTION('ref_axis',(0.,1.,0.));
#36566=DIRECTION('center_axis',(0.,0.599999999999997,-0.800000000000002));
#36567=DIRECTION('ref_axis',(0.,0.800000000000002,0.599999999999997));
#36568=DIRECTION('',(-1.,0.,0.));
#36569=DIRECTION('',(0.,0.800000000000002,0.599999999999997));
#36570=DIRECTION('',(1.,0.,0.));
#36571=DIRECTION('',(0.,0.800000000000002,0.599999999999997));
#36572=DIRECTION('center_axis',(1.,0.,0.));
#36573=DIRECTION('ref_axis',(0.,1.22464679914735E-16,1.));
#36574=DIRECTION('center_axis',(-1.,0.,0.));
#36575=DIRECTION('ref_axis',(0.,1.,0.));
#36576=DIRECTION('',(0.,-0.800000000000002,0.599999999999998));
#36577=DIRECTION('center_axis',(-1.,0.,0.));
#36578=DIRECTION('ref_axis',(0.,1.,0.));
#36579=DIRECTION('center_axis',(0.,0.599999999999998,0.800000000000002));
#36580=DIRECTION('ref_axis',(0.,-0.800000000000002,0.599999999999998));
#36581=DIRECTION('',(1.,0.,0.));
#36582=DIRECTION('',(0.,-0.800000000000002,0.599999999999998));
#36583=DIRECTION('center_axis',(1.,0.,0.));
#36584=DIRECTION('ref_axis',(0.,1.22464679914735E-16,1.));
#36585=DIRECTION('center_axis',(1.,0.,0.));
#36586=DIRECTION('ref_axis',(0.,1.,0.));
#36587=DIRECTION('center_axis',(1.,0.,0.));
#36588=DIRECTION('ref_axis',(0.,1.,0.));
#36589=DIRECTION('center_axis',(0.,0.451966109673778,-0.892035109009926));
#36590=DIRECTION('ref_axis',(0.,0.892035109009926,0.451966109673777));
#36591=DIRECTION('',(-1.,0.,0.));
#36592=DIRECTION('',(0.,0.892035109009926,0.451966109673777));
#36593=DIRECTION('',(1.,0.,0.));
#36594=DIRECTION('',(0.,0.892035109009926,0.451966109673777));
#36595=DIRECTION('center_axis',(1.,0.,0.));
#36596=DIRECTION('ref_axis',(0.,0.173648177666931,0.984807753012208));
#36597=DIRECTION('center_axis',(-1.,0.,0.));
#36598=DIRECTION('ref_axis',(0.,1.,0.));
#36599=DIRECTION('',(0.,-0.68365729580961,0.729803193940867));
#36600=DIRECTION('center_axis',(0.,0.729803193940867,0.68365729580961));
#36601=DIRECTION('ref_axis',(0.,-0.68365729580961,0.729803193940867));
#36602=DIRECTION('',(1.,0.,0.));
#36603=DIRECTION('',(0.,-0.68365729580961,0.729803193940867));
#36604=DIRECTION('center_axis',(1.,0.,0.));
#36605=DIRECTION('ref_axis',(0.,0.173648177666931,0.984807753012208));
#36606=DIRECTION('center_axis',(1.,0.,0.));
#36607=DIRECTION('ref_axis',(0.,1.,0.));
#36608=DIRECTION('center_axis',(0.,0.290199457811007,-0.956966182624129));
#36609=DIRECTION('ref_axis',(0.,0.956966182624129,0.290199457811007));
#36610=DIRECTION('',(-1.,0.,0.));
#36611=DIRECTION('',(0.,0.956966182624129,0.290199457811007));
#36612=DIRECTION('',(1.,0.,0.));
#36613=DIRECTION('',(0.,0.956966182624129,0.290199457811007));
#36614=DIRECTION('center_axis',(1.,0.,0.));
#36615=DIRECTION('ref_axis',(0.,0.342020143325669,0.939692620785908));
#36616=DIRECTION('center_axis',(-1.,0.,0.));
#36617=DIRECTION('ref_axis',(0.,1.,0.));
#36618=DIRECTION('',(0.,-0.546542010633328,0.837431687132078));
#36619=DIRECTION('center_axis',(0.,0.837431687132078,0.546542010633328));
#36620=DIRECTION('ref_axis',(0.,-0.546542010633328,0.837431687132078));
#36621=DIRECTION('',(1.,0.,0.));
#36622=DIRECTION('',(0.,-0.546542010633328,0.837431687132078));
#36623=DIRECTION('center_axis',(1.,0.,0.));
#36624=DIRECTION('ref_axis',(0.,0.342020143325669,0.939692620785908));
#36625=DIRECTION('center_axis',(1.,0.,0.));
#36626=DIRECTION('ref_axis',(0.,1.,0.));
#36627=DIRECTION('center_axis',(0.,0.11961524227066,-0.992820323027551));
#36628=DIRECTION('ref_axis',(0.,0.992820323027551,0.11961524227066));
#36629=DIRECTION('',(-1.,0.,0.));
#36630=DIRECTION('',(0.,0.992820323027551,0.11961524227066));
#36631=DIRECTION('',(1.,0.,0.));
#36632=DIRECTION('',(0.,0.992820323027551,0.11961524227066));
#36633=DIRECTION('center_axis',(1.,0.,0.));
#36634=DIRECTION('ref_axis',(0.,0.5,0.866025403784439));
#36635=DIRECTION('center_axis',(-1.,0.,0.));
#36636=DIRECTION('ref_axis',(0.,1.,0.));
#36637=DIRECTION('',(0.,-0.392820323027554,0.919615242270662));
#36638=DIRECTION('center_axis',(0.,0.919615242270662,0.392820323027554));
#36639=DIRECTION('ref_axis',(0.,-0.392820323027554,0.919615242270662));
#36640=DIRECTION('',(1.,0.,0.));
#36641=DIRECTION('',(0.,-0.392820323027554,0.919615242270662));
#36642=DIRECTION('center_axis',(1.,0.,0.));
#36643=DIRECTION('ref_axis',(0.,0.5,0.866025403784439));
#36644=DIRECTION('center_axis',(1.,0.,0.));
#36645=DIRECTION('ref_axis',(0.,1.,0.));
#36646=DIRECTION('center_axis',(0.,-0.054603421877848,-0.998508120307106));
#36647=DIRECTION('ref_axis',(0.,0.998508120307106,-0.054603421877848));
#36648=DIRECTION('',(-1.,0.,0.));
#36649=DIRECTION('',(0.,0.998508120307106,-0.054603421877848));
#36650=DIRECTION('',(1.,0.,0.));
#36651=DIRECTION('',(0.,0.998508120307106,-0.054603421877848));
#36652=DIRECTION('center_axis',(1.,0.,0.));
#36653=DIRECTION('ref_axis',(0.,0.642787609686539,0.766044443118978));
#36654=DIRECTION('center_axis',(-1.,0.,0.));
#36655=DIRECTION('ref_axis',(0.,1.,0.));
#36656=DIRECTION('',(0.,-0.227162988683262,0.973856753620618));
#36657=DIRECTION('center_axis',(0.,0.973856753620618,0.227162988683262));
#36658=DIRECTION('ref_axis',(0.,-0.227162988683262,0.973856753620618));
#36659=DIRECTION('',(1.,0.,0.));
#36660=DIRECTION('',(0.,-0.227162988683262,0.973856753620618));
#36661=DIRECTION('center_axis',(1.,0.,0.));
#36662=DIRECTION('ref_axis',(0.,0.642787609686539,0.766044443118978));
#36663=DIRECTION('center_axis',(1.,0.,0.));
#36664=DIRECTION('ref_axis',(0.,1.,0.));
#36665=DIRECTION('center_axis',(0.,-0.227162988683262,-0.973856753620618));
#36666=DIRECTION('ref_axis',(0.,0.973856753620618,-0.227162988683262));
#36667=DIRECTION('',(-1.,0.,0.));
#36668=DIRECTION('',(0.,0.973856753620618,-0.227162988683262));
#36669=DIRECTION('',(1.,0.,0.));
#36670=DIRECTION('',(0.,0.973856753620618,-0.227162988683262));
#36671=DIRECTION('center_axis',(1.,0.,0.));
#36672=DIRECTION('ref_axis',(0.,0.766044443118978,0.642787609686539));
#36673=DIRECTION('center_axis',(-1.,0.,0.));
#36674=DIRECTION('ref_axis',(0.,1.,0.));
#36675=DIRECTION('',(0.,-0.0546034218778478,0.998508120307106));
#36676=DIRECTION('center_axis',(0.,0.998508120307106,0.0546034218778478));
#36677=DIRECTION('ref_axis',(0.,-0.0546034218778478,0.998508120307106));
#36678=DIRECTION('',(1.,0.,0.));
#36679=DIRECTION('',(0.,-0.0546034218778478,0.998508120307106));
#36680=DIRECTION('center_axis',(1.,0.,0.));
#36681=DIRECTION('ref_axis',(0.,0.766044443118978,0.642787609686539));
#36682=DIRECTION('center_axis',(1.,0.,0.));
#36683=DIRECTION('ref_axis',(0.,1.,0.));
#36684=DIRECTION('center_axis',(0.,-0.392820323027554,-0.919615242270662));
#36685=DIRECTION('ref_axis',(0.,0.919615242270662,-0.392820323027554));
#36686=DIRECTION('',(-1.,0.,0.));
#36687=DIRECTION('',(0.,0.919615242270662,-0.392820323027554));
#36688=DIRECTION('',(1.,0.,0.));
#36689=DIRECTION('',(0.,0.919615242270662,-0.392820323027554));
#36690=DIRECTION('center_axis',(1.,0.,0.));
#36691=DIRECTION('ref_axis',(0.,0.866025403784439,0.5));
#36692=DIRECTION('center_axis',(-1.,0.,0.));
#36693=DIRECTION('ref_axis',(0.,1.,0.));
#36694=DIRECTION('',(0.,0.11961524227066,0.992820323027551));
#36695=DIRECTION('center_axis',(0.,0.992820323027551,-0.11961524227066));
#36696=DIRECTION('ref_axis',(0.,0.11961524227066,0.992820323027551));
#36697=DIRECTION('',(1.,0.,0.));
#36698=DIRECTION('',(0.,0.11961524227066,0.992820323027551));
#36699=DIRECTION('center_axis',(1.,0.,0.));
#36700=DIRECTION('ref_axis',(0.,0.866025403784439,0.5));
#36701=DIRECTION('center_axis',(1.,0.,0.));
#36702=DIRECTION('ref_axis',(0.,1.,0.));
#36703=DIRECTION('center_axis',(0.,-0.546542010633328,-0.837431687132078));
#36704=DIRECTION('ref_axis',(0.,0.837431687132078,-0.546542010633328));
#36705=DIRECTION('',(-1.,0.,0.));
#36706=DIRECTION('',(0.,0.837431687132078,-0.546542010633328));
#36707=DIRECTION('',(1.,0.,0.));
#36708=DIRECTION('',(0.,0.837431687132078,-0.546542010633328));
#36709=DIRECTION('center_axis',(1.,0.,0.));
#36710=DIRECTION('ref_axis',(0.,0.939692620785908,0.342020143325669));
#36711=DIRECTION('center_axis',(-1.,0.,0.));
#36712=DIRECTION('ref_axis',(0.,1.,0.));
#36713=DIRECTION('',(0.,0.290199457811007,0.956966182624129));
#36714=DIRECTION('center_axis',(0.,0.956966182624129,-0.290199457811007));
#36715=DIRECTION('ref_axis',(0.,0.290199457811007,0.956966182624129));
#36716=DIRECTION('',(1.,0.,0.));
#36717=DIRECTION('',(0.,0.290199457811007,0.956966182624129));
#36718=DIRECTION('center_axis',(1.,0.,0.));
#36719=DIRECTION('ref_axis',(0.,0.939692620785908,0.342020143325669));
#36720=DIRECTION('center_axis',(1.,0.,0.));
#36721=DIRECTION('ref_axis',(0.,1.,0.));
#36722=DIRECTION('center_axis',(0.,-0.683657295809611,-0.729803193940867));
#36723=DIRECTION('ref_axis',(0.,0.729803193940867,-0.683657295809611));
#36724=DIRECTION('',(-1.,0.,0.));
#36725=DIRECTION('',(0.,0.729803193940867,-0.683657295809611));
#36726=DIRECTION('',(1.,0.,0.));
#36727=DIRECTION('',(0.,0.729803193940867,-0.683657295809611));
#36728=DIRECTION('center_axis',(1.,0.,0.));
#36729=DIRECTION('ref_axis',(0.,0.984807753012208,0.17364817766693));
#36730=DIRECTION('center_axis',(-1.,0.,0.));
#36731=DIRECTION('ref_axis',(0.,1.,0.));
#36732=DIRECTION('',(0.,0.451966109673778,0.892035109009926));
#36733=DIRECTION('center_axis',(0.,0.892035109009926,-0.451966109673778));
#36734=DIRECTION('ref_axis',(0.,0.451966109673778,0.892035109009926));
#36735=DIRECTION('',(1.,0.,0.));
#36736=DIRECTION('',(0.,0.451966109673778,0.892035109009926));
#36737=DIRECTION('center_axis',(1.,0.,0.));
#36738=DIRECTION('ref_axis',(0.,0.984807753012208,0.17364817766693));
#36739=DIRECTION('center_axis',(1.,0.,0.));
#36740=DIRECTION('ref_axis',(0.,1.,0.));
#36741=DIRECTION('center_axis',(0.,-0.800000000000002,-0.599999999999998));
#36742=DIRECTION('ref_axis',(0.,0.599999999999998,-0.800000000000002));
#36743=DIRECTION('',(-1.,0.,0.));
#36744=DIRECTION('',(0.,0.599999999999998,-0.800000000000002));
#36745=DIRECTION('',(1.,0.,0.));
#36746=DIRECTION('',(0.,0.599999999999998,-0.800000000000002));
#36747=DIRECTION('center_axis',(1.,0.,0.));
#36748=DIRECTION('ref_axis',(0.,1.,-6.12323399573677E-17));
#36749=DIRECTION('center_axis',(-1.,0.,0.));
#36750=DIRECTION('ref_axis',(0.,1.,0.));
#36751=DIRECTION('',(0.,0.599999999999998,0.800000000000002));
#36752=DIRECTION('center_axis',(0.,0.800000000000002,-0.599999999999998));
#36753=DIRECTION('ref_axis',(0.,0.599999999999998,0.800000000000002));
#36754=DIRECTION('',(1.,0.,0.));
#36755=DIRECTION('',(0.,0.599999999999998,0.800000000000002));
#36756=DIRECTION('center_axis',(1.,0.,0.));
#36757=DIRECTION('ref_axis',(0.,1.,-6.12323399573677E-17));
#36758=DIRECTION('center_axis',(1.,0.,0.));
#36759=DIRECTION('ref_axis',(0.,1.,0.));
#36760=DIRECTION('center_axis',(0.,-0.892035109009926,-0.451966109673778));
#36761=DIRECTION('ref_axis',(0.,0.451966109673778,-0.892035109009926));
#36762=DIRECTION('',(-1.,0.,0.));
#36763=DIRECTION('',(0.,0.451966109673778,-0.892035109009926));
#36764=DIRECTION('',(1.,0.,0.));
#36765=DIRECTION('',(0.,0.451966109673778,-0.892035109009926));
#36766=DIRECTION('center_axis',(1.,0.,0.));
#36767=DIRECTION('ref_axis',(0.,0.984807753012208,-0.17364817766693));
#36768=DIRECTION('center_axis',(-1.,0.,0.));
#36769=DIRECTION('ref_axis',(0.,1.,0.));
#36770=DIRECTION('',(0.,0.729803193940867,0.68365729580961));
#36771=DIRECTION('center_axis',(0.,0.683657295809611,-0.729803193940867));
#36772=DIRECTION('ref_axis',(0.,0.729803193940867,0.68365729580961));
#36773=DIRECTION('',(1.,0.,0.));
#36774=DIRECTION('',(0.,0.729803193940867,0.68365729580961));
#36775=DIRECTION('center_axis',(1.,0.,0.));
#36776=DIRECTION('ref_axis',(0.,0.984807753012208,-0.17364817766693));
#36777=DIRECTION('center_axis',(1.,0.,0.));
#36778=DIRECTION('ref_axis',(0.,1.,0.));
#36779=DIRECTION('center_axis',(0.,-0.956966182624129,-0.290199457811007));
#36780=DIRECTION('ref_axis',(0.,0.290199457811007,-0.956966182624129));
#36781=DIRECTION('',(-1.,0.,0.));
#36782=DIRECTION('',(0.,0.290199457811007,-0.956966182624129));
#36783=DIRECTION('',(1.,0.,0.));
#36784=DIRECTION('',(0.,0.290199457811007,-0.956966182624129));
#36785=DIRECTION('center_axis',(1.,0.,0.));
#36786=DIRECTION('ref_axis',(0.,0.939692620785908,-0.342020143325669));
#36787=DIRECTION('center_axis',(-1.,0.,0.));
#36788=DIRECTION('ref_axis',(0.,1.,0.));
#36789=DIRECTION('',(0.,0.837431687132078,0.546542010633328));
#36790=DIRECTION('center_axis',(0.,0.546542010633328,-0.837431687132078));
#36791=DIRECTION('ref_axis',(0.,0.837431687132078,0.546542010633328));
#36792=DIRECTION('',(1.,0.,0.));
#36793=DIRECTION('',(0.,0.837431687132078,0.546542010633328));
#36794=DIRECTION('center_axis',(1.,0.,0.));
#36795=DIRECTION('ref_axis',(0.,0.939692620785908,-0.342020143325669));
#36796=DIRECTION('center_axis',(1.,0.,0.));
#36797=DIRECTION('ref_axis',(0.,1.,0.));
#36798=DIRECTION('center_axis',(0.,-0.992820323027551,-0.11961524227066));
#36799=DIRECTION('ref_axis',(0.,0.11961524227066,-0.992820323027551));
#36800=DIRECTION('',(-1.,0.,0.));
#36801=DIRECTION('',(0.,0.11961524227066,-0.992820323027551));
#36802=DIRECTION('',(1.,0.,0.));
#36803=DIRECTION('',(0.,0.11961524227066,-0.992820323027551));
#36804=DIRECTION('center_axis',(1.,0.,0.));
#36805=DIRECTION('ref_axis',(0.,0.866025403784439,-0.5));
#36806=DIRECTION('center_axis',(-1.,0.,0.));
#36807=DIRECTION('ref_axis',(0.,1.,0.));
#36808=DIRECTION('',(0.,0.919615242270662,0.392820323027554));
#36809=DIRECTION('center_axis',(0.,0.392820323027554,-0.919615242270662));
#36810=DIRECTION('ref_axis',(0.,0.919615242270662,0.392820323027554));
#36811=DIRECTION('',(1.,0.,0.));
#36812=DIRECTION('',(0.,0.919615242270662,0.392820323027554));
#36813=DIRECTION('center_axis',(1.,0.,0.));
#36814=DIRECTION('ref_axis',(0.,0.866025403784439,-0.5));
#36815=DIRECTION('center_axis',(1.,0.,0.));
#36816=DIRECTION('ref_axis',(0.,1.,0.));
#36817=DIRECTION('center_axis',(0.,-0.998508120307106,0.0546034218778478));
#36818=DIRECTION('ref_axis',(0.,-0.0546034218778478,-0.998508120307106));
#36819=DIRECTION('',(-1.,0.,0.));
#36820=DIRECTION('',(0.,-0.0546034218778478,-0.998508120307106));
#36821=DIRECTION('',(1.,0.,0.));
#36822=DIRECTION('',(0.,-0.0546034218778478,-0.998508120307106));
#36823=DIRECTION('center_axis',(1.,0.,0.));
#36824=DIRECTION('ref_axis',(0.,0.766044443118978,-0.642787609686539));
#36825=DIRECTION('center_axis',(-1.,0.,0.));
#36826=DIRECTION('ref_axis',(0.,1.,0.));
#36827=DIRECTION('',(0.,0.973856753620618,0.227162988683262));
#36828=DIRECTION('center_axis',(0.,0.227162988683262,-0.973856753620618));
#36829=DIRECTION('ref_axis',(0.,0.973856753620618,0.227162988683262));
#36830=DIRECTION('',(1.,0.,0.));
#36831=DIRECTION('',(0.,0.973856753620618,0.227162988683262));
#36832=DIRECTION('center_axis',(1.,0.,0.));
#36833=DIRECTION('ref_axis',(0.,0.766044443118978,-0.642787609686539));
#36834=DIRECTION('center_axis',(1.,0.,0.));
#36835=DIRECTION('ref_axis',(0.,1.,0.));
#36836=DIRECTION('center_axis',(0.,-0.973856753620618,0.227162988683262));
#36837=DIRECTION('ref_axis',(0.,-0.227162988683262,-0.973856753620618));
#36838=DIRECTION('',(-1.,0.,0.));
#36839=DIRECTION('',(0.,-0.227162988683262,-0.973856753620618));
#36840=DIRECTION('',(1.,0.,0.));
#36841=DIRECTION('',(0.,-0.227162988683262,-0.973856753620618));
#36842=DIRECTION('center_axis',(1.,0.,0.));
#36843=DIRECTION('ref_axis',(0.,0.642787609686539,-0.766044443118978));
#36844=DIRECTION('center_axis',(-1.,0.,0.));
#36845=DIRECTION('ref_axis',(0.,1.,0.));
#36846=DIRECTION('',(0.,0.998508120307106,0.0546034218778477));
#36847=DIRECTION('center_axis',(0.,0.0546034218778477,-0.998508120307106));
#36848=DIRECTION('ref_axis',(0.,0.998508120307106,0.0546034218778477));
#36849=DIRECTION('',(1.,0.,0.));
#36850=DIRECTION('',(0.,0.998508120307106,0.0546034218778477));
#36851=DIRECTION('center_axis',(1.,0.,0.));
#36852=DIRECTION('ref_axis',(0.,0.642787609686539,-0.766044443118978));
#36853=DIRECTION('center_axis',(1.,0.,0.));
#36854=DIRECTION('ref_axis',(0.,1.,0.));
#36855=DIRECTION('center_axis',(0.,-0.919615242270662,0.392820323027554));
#36856=DIRECTION('ref_axis',(0.,-0.392820323027554,-0.919615242270662));
#36857=DIRECTION('',(-1.,0.,0.));
#36858=DIRECTION('',(0.,-0.392820323027554,-0.919615242270662));
#36859=DIRECTION('',(1.,0.,0.));
#36860=DIRECTION('',(0.,-0.392820323027554,-0.919615242270662));
#36861=DIRECTION('center_axis',(1.,0.,0.));
#36862=DIRECTION('ref_axis',(0.,0.5,-0.866025403784439));
#36863=DIRECTION('center_axis',(-1.,0.,0.));
#36864=DIRECTION('ref_axis',(0.,1.,0.));
#36865=DIRECTION('',(0.,0.992820323027551,-0.11961524227066));
#36866=DIRECTION('center_axis',(0.,-0.11961524227066,-0.992820323027551));
#36867=DIRECTION('ref_axis',(0.,0.992820323027551,-0.11961524227066));
#36868=DIRECTION('',(1.,0.,0.));
#36869=DIRECTION('',(0.,0.992820323027551,-0.11961524227066));
#36870=DIRECTION('center_axis',(1.,0.,0.));
#36871=DIRECTION('ref_axis',(0.,0.5,-0.866025403784439));
#36872=DIRECTION('center_axis',(1.,0.,0.));
#36873=DIRECTION('ref_axis',(0.,1.,0.));
#36874=DIRECTION('center_axis',(0.,-0.837431687132078,0.546542010633328));
#36875=DIRECTION('ref_axis',(0.,-0.546542010633328,-0.837431687132078));
#36876=DIRECTION('',(-1.,0.,0.));
#36877=DIRECTION('',(0.,-0.546542010633328,-0.837431687132078));
#36878=DIRECTION('',(1.,0.,0.));
#36879=DIRECTION('',(0.,-0.546542010633328,-0.837431687132078));
#36880=DIRECTION('center_axis',(1.,0.,0.));
#36881=DIRECTION('ref_axis',(0.,0.342020143325669,-0.939692620785908));
#36882=DIRECTION('center_axis',(-1.,0.,0.));
#36883=DIRECTION('ref_axis',(0.,1.,0.));
#36884=DIRECTION('',(0.,0.956966182624129,-0.290199457811007));
#36885=DIRECTION('center_axis',(0.,-0.290199457811007,-0.956966182624129));
#36886=DIRECTION('ref_axis',(0.,0.956966182624129,-0.290199457811007));
#36887=DIRECTION('',(1.,0.,0.));
#36888=DIRECTION('',(0.,0.956966182624129,-0.290199457811007));
#36889=DIRECTION('center_axis',(1.,0.,0.));
#36890=DIRECTION('ref_axis',(0.,0.342020143325669,-0.939692620785908));
#36891=DIRECTION('center_axis',(1.,0.,0.));
#36892=DIRECTION('ref_axis',(0.,1.,0.));
#36893=DIRECTION('center_axis',(0.,-0.729803193940867,0.683657295809611));
#36894=DIRECTION('ref_axis',(0.,-0.683657295809611,-0.729803193940867));
#36895=DIRECTION('',(-1.,0.,0.));
#36896=DIRECTION('',(0.,-0.683657295809611,-0.729803193940867));
#36897=DIRECTION('',(1.,0.,0.));
#36898=DIRECTION('',(0.,-0.683657295809611,-0.729803193940867));
#36899=DIRECTION('center_axis',(1.,0.,0.));
#36900=DIRECTION('ref_axis',(0.,0.17364817766693,-0.984807753012208));
#36901=DIRECTION('center_axis',(-1.,0.,0.));
#36902=DIRECTION('ref_axis',(0.,1.,0.));
#36903=DIRECTION('',(0.,0.892035109009926,-0.451966109673778));
#36904=DIRECTION('center_axis',(0.,-0.451966109673778,-0.892035109009926));
#36905=DIRECTION('ref_axis',(0.,0.892035109009926,-0.451966109673778));
#36906=DIRECTION('',(1.,0.,0.));
#36907=DIRECTION('',(0.,0.892035109009926,-0.451966109673778));
#36908=DIRECTION('center_axis',(1.,0.,0.));
#36909=DIRECTION('ref_axis',(0.,0.17364817766693,-0.984807753012208));
#36910=DIRECTION('center_axis',(1.,0.,0.));
#36911=DIRECTION('ref_axis',(0.,1.,0.));
#36912=DIRECTION('center_axis',(0.,-0.599999999999998,0.800000000000002));
#36913=DIRECTION('ref_axis',(0.,-0.800000000000002,-0.599999999999998));
#36914=DIRECTION('',(-1.,0.,0.));
#36915=DIRECTION('',(0.,-0.800000000000002,-0.599999999999998));
#36916=DIRECTION('',(1.,0.,0.));
#36917=DIRECTION('',(0.,-0.800000000000002,-0.599999999999998));
#36918=DIRECTION('center_axis',(1.,0.,0.));
#36919=DIRECTION('ref_axis',(0.,0.,-1.));
#36920=DIRECTION('center_axis',(-1.,0.,0.));
#36921=DIRECTION('ref_axis',(0.,1.,0.));
#36922=DIRECTION('',(0.,0.800000000000002,-0.599999999999998));
#36923=DIRECTION('center_axis',(0.,-0.599999999999998,-0.800000000000002));
#36924=DIRECTION('ref_axis',(0.,0.800000000000002,-0.599999999999998));
#36925=DIRECTION('',(1.,0.,0.));
#36926=DIRECTION('',(0.,0.800000000000002,-0.599999999999998));
#36927=DIRECTION('center_axis',(1.,0.,0.));
#36928=DIRECTION('ref_axis',(0.,0.,-1.));
#36929=DIRECTION('center_axis',(1.,0.,0.));
#36930=DIRECTION('ref_axis',(0.,1.,0.));
#36931=DIRECTION('center_axis',(0.,0.5,0.866025403784439));
#36932=DIRECTION('ref_axis',(0.,0.866025403784439,-0.5));
#36933=DIRECTION('',(0.,0.866025403784439,-0.5));
#36934=DIRECTION('',(-1.,0.,0.));
#36935=DIRECTION('',(0.,0.866025403784439,-0.5));
#36936=DIRECTION('',(-1.,0.,0.));
#36937=DIRECTION('center_axis',(0.,-0.5,0.866025403784439));
#36938=DIRECTION('ref_axis',(0.,0.866025403784439,0.5));
#36939=DIRECTION('',(0.,0.866025403784439,0.5));
#36940=DIRECTION('',(-1.,0.,0.));
#36941=DIRECTION('',(0.,0.866025403784439,0.5));
#36942=DIRECTION('center_axis',(0.,-1.,-1.20185167898973E-16));
#36943=DIRECTION('ref_axis',(0.,-1.20185167898973E-16,1.));
#36944=DIRECTION('',(0.,-1.20185167898973E-16,1.));
#36945=DIRECTION('',(-1.,0.,0.));
#36946=DIRECTION('',(0.,-1.20185167898973E-16,1.));
#36947=DIRECTION('center_axis',(0.,-0.5,-0.866025403784439));
#36948=DIRECTION('ref_axis',(0.,-0.866025403784439,0.5));
#36949=DIRECTION('',(0.,-0.866025403784439,0.5));
#36950=DIRECTION('',(-1.,0.,0.));
#36951=DIRECTION('',(0.,-0.866025403784439,0.5));
#36952=DIRECTION('center_axis',(0.,0.5,-0.866025403784439));
#36953=DIRECTION('ref_axis',(0.,-0.866025403784439,-0.5));
#36954=DIRECTION('',(0.,-0.866025403784439,-0.5));
#36955=DIRECTION('',(-1.,0.,0.));
#36956=DIRECTION('',(0.,-0.866025403784439,-0.5));
#36957=DIRECTION('center_axis',(0.,1.,-3.60555503696918E-16));
#36958=DIRECTION('ref_axis',(0.,-3.60555503696918E-16,-1.));
#36959=DIRECTION('',(0.,-3.60555503696918E-16,-1.));
#36960=DIRECTION('',(0.,-3.60555503696918E-16,-1.));
#36961=DIRECTION('center_axis',(-1.,0.,0.));
#36962=DIRECTION('ref_axis',(0.,0.,1.));
#36963=DIRECTION('center_axis',(-1.,0.,0.));
#36964=DIRECTION('ref_axis',(0.,0.,1.));
#36965=DIRECTION('center_axis',(1.,0.,0.));
#36966=DIRECTION('ref_axis',(0.,0.,-1.));
#36967=DIRECTION('center_axis',(1.,0.,0.));
#36968=DIRECTION('ref_axis',(0.,1.,0.));
#36969=DIRECTION('',(-0.707106781186546,0.707106781186549,8.65956056235495E-17));
#36970=DIRECTION('center_axis',(1.,0.,0.));
#36971=DIRECTION('ref_axis',(0.,1.,0.));
#36972=DIRECTION('center_axis',(1.,0.,0.));
#36973=DIRECTION('ref_axis',(0.,1.,0.));
#36974=DIRECTION('center_axis',(-1.,0.,0.));
#36975=DIRECTION('ref_axis',(0.,0.,1.));
#36976=DIRECTION('center_axis',(1.,0.,0.));
#36977=DIRECTION('ref_axis',(0.,0.,-1.));
#36978=DIRECTION('center_axis',(1.,0.,0.));
#36979=DIRECTION('ref_axis',(0.,1.,0.));
#36980=DIRECTION('center_axis',(1.,0.,0.));
#36981=DIRECTION('ref_axis',(0.,0.,-1.));
#36982=DIRECTION('',(-1.,0.,0.));
#36983=DIRECTION('',(-1.,0.,0.));
#36984=DIRECTION('center_axis',(-1.,0.,0.));
#36985=DIRECTION('ref_axis',(0.,1.,0.));
#36986=DIRECTION('center_axis',(1.,0.,0.));
#36987=DIRECTION('ref_axis',(0.,0.,-1.));
#36988=DIRECTION('',(-0.707106781186547,-0.707106781186548,-8.65956056235494E-17));
#36989=DIRECTION('center_axis',(1.,0.,0.));
#36990=DIRECTION('ref_axis',(0.,0.,-1.));
#36991=DIRECTION('axis',(0.,0.,1.));
#36992=DIRECTION('refdir',(1.,0.,0.));
#36993=DIRECTION('center_axis',(0.547750005235851,-0.72455327535185,0.418321028566615));
#36994=DIRECTION('ref_axis',(0.606949534647157,0.,-0.794740374205061));
#36995=DIRECTION('',(0.677497944020809,0.0907675134870615,-0.729902592366237));
#36996=DIRECTION('',(0.,0.499999999999999,0.866025403784439));
#36997=DIRECTION('',(-0.677497944020809,-0.677497944020809,-0.286344323664976));
#36998=DIRECTION('center_axis',(0.,-0.866025403784439,0.5));
#36999=DIRECTION('ref_axis',(0.,-0.5,-0.866025403784439));
#37000=DIRECTION('',(0.,-0.5,-0.866025403784439));
#37001=DIRECTION('',(1.,0.,0.));
#37002=DIRECTION('',(-1.,0.,0.));
#37003=DIRECTION('center_axis',(0.547750005235853,0.,0.83664205713323));
#37004=DIRECTION('ref_axis',(0.83664205713323,0.,-0.547750005235853));
#37005=DIRECTION('',(0.67749794402081,-0.586730430533748,-0.44355826870126));
#37006=DIRECTION('',(0.,1.,0.));
#37007=DIRECTION('',(-0.677497944020809,-0.586730430533747,0.443558268701262));
#37008=DIRECTION('center_axis',(0.,0.,1.));
#37009=DIRECTION('ref_axis',(1.,0.,0.));
#37010=DIRECTION('',(0.,-1.,0.));
#37011=DIRECTION('',(1.,0.,0.));
#37012=DIRECTION('',(-1.,0.,0.));
#37013=DIRECTION('center_axis',(0.707106781186548,-0.353553390593274,0.612372435695794));
#37014=DIRECTION('ref_axis',(0.654653670707977,0.,-0.755928946018455));
#37015=DIRECTION('',(0.,0.866025403784439,0.5));
#37016=DIRECTION('',(0.,-0.866025403784439,-0.5));
#37017=DIRECTION('center_axis',(0.547750005235853,-0.72455327535185,-0.418321028566614));
#37018=DIRECTION('ref_axis',(-0.606949534647155,0.,-0.794740374205062));
#37019=DIRECTION('',(0.677497944020809,0.677497944020809,-0.286344323664976));
#37020=DIRECTION('',(0.,-0.499999999999999,0.866025403784439));
#37021=DIRECTION('',(-0.67749794402081,-0.0907675134870647,-0.729902592366236));
#37022=DIRECTION('center_axis',(0.,-0.866025403784439,-0.499999999999999));
#37023=DIRECTION('ref_axis',(0.,0.499999999999999,-0.866025403784439));
#37024=DIRECTION('',(0.,0.499999999999999,-0.866025403784439));
#37025=DIRECTION('',(1.,0.,0.));
#37026=DIRECTION('',(-1.,0.,0.));
#37027=DIRECTION('center_axis',(0.54775000523585,0.72455327535185,0.418321028566616));
#37028=DIRECTION('ref_axis',(0.606949534647158,0.,-0.79474037420506));
#37029=DIRECTION('',(0.67749794402081,-0.67749794402081,0.286344323664975));
#37030=DIRECTION('',(0.,0.5,-0.866025403784439));
#37031=DIRECTION('',(-0.677497944020809,0.0907675134870601,0.729902592366237));
#37032=DIRECTION('center_axis',(0.,0.866025403784439,0.5));
#37033=DIRECTION('ref_axis',(1.,0.,0.));
#37034=DIRECTION('',(0.,-0.5,0.866025403784439));
#37035=DIRECTION('',(1.,0.,0.));
#37036=DIRECTION('',(-1.,0.,0.));
#37037=DIRECTION('center_axis',(0.707106781186547,0.353553390593274,0.612372435695795));
#37038=DIRECTION('ref_axis',(0.654653670707977,0.,-0.755928946018454));
#37039=DIRECTION('',(0.,0.866025403784439,-0.5));
#37040=DIRECTION('',(0.,-0.866025403784439,0.5));
#37041=DIRECTION('center_axis',(0.54775000523585,-1.07255430515093E-15,
-0.836642057133232));
#37042=DIRECTION('ref_axis',(-0.836642057133232,0.,-0.54775000523585));
#37043=DIRECTION('',(0.677497944020808,0.58673043053375,0.443558268701259));
#37044=DIRECTION('',(0.,-1.,1.28197512425571E-15));
#37045=DIRECTION('',(-0.67749794402081,0.586730430533747,-0.44355826870126));
#37046=DIRECTION('center_axis',(0.,-1.28197512425571E-15,-1.));
#37047=DIRECTION('ref_axis',(-1.,0.,0.));
#37048=DIRECTION('',(0.,1.,-1.28197512425571E-15));
#37049=DIRECTION('',(1.,0.,0.));
#37050=DIRECTION('',(-1.,0.,0.));
#37051=DIRECTION('center_axis',(0.54775000523585,0.72455327535185,-0.418321028566616));
#37052=DIRECTION('ref_axis',(-0.606949534647158,0.,-0.794740374205059));
#37053=DIRECTION('',(0.677497944020809,-0.0907675134870586,0.729902592366237));
#37054=DIRECTION('',(0.,-0.500000000000001,-0.866025403784438));
#37055=DIRECTION('',(-0.677497944020809,0.677497944020809,0.286344323664978));
#37056=DIRECTION('center_axis',(0.,0.866025403784438,-0.500000000000001));
#37057=DIRECTION('ref_axis',(-1.,0.,0.));
#37058=DIRECTION('',(0.,0.500000000000001,0.866025403784438));
#37059=DIRECTION('',(1.,0.,0.));
#37060=DIRECTION('',(-1.,0.,0.));
#37061=DIRECTION('center_axis',(0.707106781186548,0.707106781186548,-1.94248565072931E-16));
#37062=DIRECTION('ref_axis',(-2.74708955197652E-16,0.,-1.));
#37063=DIRECTION('',(0.,-2.74708955197652E-16,-1.));
#37064=DIRECTION('',(0.,2.74708955197652E-16,1.));
#37065=DIRECTION('center_axis',(0.707106781186547,0.353553390593274,-0.612372435695795));
#37066=DIRECTION('ref_axis',(-0.654653670707978,0.,-0.755928946018454));
#37067=DIRECTION('',(0.,-0.866025403784439,-0.5));
#37068=DIRECTION('',(0.,0.866025403784439,0.5));
#37069=DIRECTION('center_axis',(0.707106781186548,-0.353553390593274,-0.612372435695794));
#37070=DIRECTION('ref_axis',(-0.654653670707977,0.,-0.755928946018455));
#37071=DIRECTION('',(0.,-0.866025403784439,0.5));
#37072=DIRECTION('',(0.,0.866025403784439,-0.5));
#37073=DIRECTION('center_axis',(0.707106781186548,-0.707106781186548,-9.71242825364656E-17));
#37074=DIRECTION('ref_axis',(-1.37354477598826E-16,0.,-1.));
#37075=DIRECTION('',(0.,-1.37354477598826E-16,1.));
#37076=DIRECTION('',(0.,1.37354477598826E-16,-1.));
#37077=DIRECTION('center_axis',(0.,-0.5,0.866025403784439));
#37078=DIRECTION('ref_axis',(0.,-0.866025403784439,-0.5));
#37079=DIRECTION('',(0.,-0.866025403784439,-0.5));
#37080=DIRECTION('center_axis',(0.,0.5,0.866025403784439));
#37081=DIRECTION('ref_axis',(0.,-0.866025403784439,0.5));
#37082=DIRECTION('',(0.,-0.866025403784439,0.5));
#37083=DIRECTION('center_axis',(0.,1.,-2.74708955197652E-16));
#37084=DIRECTION('ref_axis',(0.,2.74708955197652E-16,1.));
#37085=DIRECTION('',(0.,2.74708955197652E-16,1.));
#37086=DIRECTION('center_axis',(1.,0.,0.));
#37087=DIRECTION('ref_axis',(0.,0.,-1.));
#37088=DIRECTION('',(0.,-0.866025403784439,0.5));
#37089=DIRECTION('',(0.,3.20493781063927E-16,1.));
#37090=DIRECTION('',(0.,0.866025403784439,0.5));
#37091=DIRECTION('',(0.,0.866025403784439,-0.5));
#37092=DIRECTION('',(0.,1.60246890531964E-16,-1.));
#37093=DIRECTION('',(0.,-0.866025403784439,-0.5));
#37094=DIRECTION('center_axis',(0.707106781186547,0.353553390593274,0.612372435695795));
#37095=DIRECTION('ref_axis',(0.654653670707978,0.,-0.755928946018454));
#37096=DIRECTION('',(-0.654653670707977,-4.69765578524213E-16,0.755928946018454));
#37097=DIRECTION('',(0.,-0.866025403784439,0.5));
#37098=DIRECTION('',(-0.654653670707978,0.654653670707977,0.377964473009227));
#37099=DIRECTION('center_axis',(0.707106781186548,-0.353553390593273,0.612372435695795));
#37100=DIRECTION('ref_axis',(0.654653670707977,0.,-0.755928946018455));
#37101=DIRECTION('',(-0.654653670707977,-0.654653670707976,0.377964473009229));
#37102=DIRECTION('',(0.,-0.866025403784439,-0.5));
#37103=DIRECTION('center_axis',(0.707106781186547,-0.353553390593274,-0.612372435695795));
#37104=DIRECTION('ref_axis',(-0.654653670707978,0.,-0.755928946018454));
#37105=DIRECTION('',(-0.654653670707977,1.00453536761267E-15,-0.755928946018454));
#37106=DIRECTION('',(0.,0.866025403784439,-0.5));
#37107=DIRECTION('',(0.654653670707978,0.654653670707977,0.377964473009227));
#37108=DIRECTION('center_axis',(0.707106781186548,0.353553390593274,-0.612372435695794));
#37109=DIRECTION('ref_axis',(-0.654653670707977,0.,-0.755928946018455));
#37110=DIRECTION('',(0.,0.866025403784439,0.5));
#37111=DIRECTION('',(-0.654653670707977,0.654653670707977,-0.377964473009228));
#37112=DIRECTION('center_axis',(0.707106781186547,-0.707106781186548,2.2662332591842E-16));
#37113=DIRECTION('ref_axis',(3.20493781063928E-16,0.,-1.));
#37114=DIRECTION('',(0.,-3.20493781063927E-16,-1.));
#37115=DIRECTION('center_axis',(0.707106781186547,0.707106781186548,1.1331166295921E-16));
#37116=DIRECTION('ref_axis',(1.60246890531964E-16,0.,-1.));
#37117=DIRECTION('',(0.,-1.60246890531964E-16,1.));
#37118=DIRECTION('center_axis',(0.,0.5,-0.866025403784439));
#37119=DIRECTION('ref_axis',(0.,-0.866025403784439,-0.5));
#37120=DIRECTION('',(-1.,0.,0.));
#37121=DIRECTION('',(0.,-0.866025403784439,-0.5));
#37122=DIRECTION('',(-1.,0.,0.));
#37123=DIRECTION('center_axis',(0.,1.,-3.20493781063927E-16));
#37124=DIRECTION('ref_axis',(0.,-3.20493781063927E-16,-1.));
#37125=DIRECTION('',(-1.,0.,0.));
#37126=DIRECTION('',(0.,-3.20493781063927E-16,-1.));
#37127=DIRECTION('center_axis',(0.,0.5,0.866025403784439));
#37128=DIRECTION('ref_axis',(0.,0.866025403784439,-0.5));
#37129=DIRECTION('',(-1.,0.,0.));
#37130=DIRECTION('',(0.,0.866025403784439,-0.5));
#37131=DIRECTION('center_axis',(0.,-0.5,0.866025403784439));
#37132=DIRECTION('ref_axis',(0.,0.866025403784439,0.5));
#37133=DIRECTION('',(-1.,0.,0.));
#37134=DIRECTION('',(0.,0.866025403784439,0.5));
#37135=DIRECTION('center_axis',(0.,-1.,-1.60246890531964E-16));
#37136=DIRECTION('ref_axis',(0.,-1.60246890531964E-16,1.));
#37137=DIRECTION('',(-1.,0.,0.));
#37138=DIRECTION('',(0.,-1.60246890531964E-16,1.));
#37139=DIRECTION('center_axis',(0.,-0.5,-0.866025403784439));
#37140=DIRECTION('ref_axis',(0.,-0.866025403784439,0.5));
#37141=DIRECTION('',(0.,-0.866025403784439,0.5));
#37142=DIRECTION('center_axis',(-1.,0.,0.));
#37143=DIRECTION('ref_axis',(0.,0.,1.));
#37144=DIRECTION('center_axis',(1.,0.,0.));
#37145=DIRECTION('ref_axis',(0.,0.,-1.));
#37146=DIRECTION('',(0.,0.866025403784439,0.5));
#37147=DIRECTION('',(0.,0.866025403784439,-0.5));
#37148=DIRECTION('',(0.,1.37354477598826E-16,-1.));
#37149=DIRECTION('center_axis',(1.,0.,0.));
#37150=DIRECTION('ref_axis',(0.,0.,-1.));
#37151=DIRECTION('center_axis',(0.,0.5,-0.866025403784439));
#37152=DIRECTION('ref_axis',(0.,0.866025403784439,0.5));
#37153=DIRECTION('center_axis',(0.,-0.5,-0.866025403784439));
#37154=DIRECTION('ref_axis',(0.,0.866025403784439,-0.5));
#37155=DIRECTION('center_axis',(0.,-1.,-1.37354477598826E-16));
#37156=DIRECTION('ref_axis',(0.,1.37354477598826E-16,-1.));
#37157=DIRECTION('center_axis',(-1.,0.,0.));
#37158=DIRECTION('ref_axis',(0.,0.,1.));
#37159=DIRECTION('center_axis',(1.,0.,0.));
#37160=DIRECTION('ref_axis',(0.,0.,-1.));
#37161=DIRECTION('center_axis',(1.,0.,0.));
#37162=DIRECTION('ref_axis',(0.,1.,0.));
#37163=DIRECTION('center_axis',(1.,0.,0.));
#37164=DIRECTION('ref_axis',(0.,0.,-1.));
#37165=DIRECTION('',(-0.707106781186548,0.707106781186547,8.65956056235492E-17));
#37166=DIRECTION('center_axis',(1.,0.,0.));
#37167=DIRECTION('ref_axis',(0.,1.,0.));
#37168=DIRECTION('',(-1.,0.,0.));
#37169=DIRECTION('axis',(0.,0.,1.));
#37170=DIRECTION('refdir',(1.,0.,0.));
#37171=DIRECTION('center_axis',(1.,0.,0.));
#37172=DIRECTION('ref_axis',(0.,1.,0.));
#37173=DIRECTION('',(-1.,0.,0.));
#37174=DIRECTION('center_axis',(1.,0.,0.));
#37175=DIRECTION('ref_axis',(0.,1.,0.));
#37176=DIRECTION('center_axis',(1.,0.,0.));
#37177=DIRECTION('ref_axis',(0.,1.,0.));
#37178=DIRECTION('',(-1.,0.,0.));
#37179=DIRECTION('center_axis',(1.,0.,0.));
#37180=DIRECTION('ref_axis',(0.,1.,0.));
#37181=DIRECTION('',(-1.,0.,0.));
#37182=DIRECTION('center_axis',(1.,0.,0.));
#37183=DIRECTION('ref_axis',(0.,1.,0.));
#37184=DIRECTION('',(-1.,0.,0.));
#37185=DIRECTION('center_axis',(1.,0.,0.));
#37186=DIRECTION('ref_axis',(0.,1.,0.));
#37187=DIRECTION('',(-1.,0.,0.));
#37188=DIRECTION('center_axis',(1.,0.,0.));
#37189=DIRECTION('ref_axis',(0.,1.,0.));
#37190=DIRECTION('',(-1.,0.,0.));
#37191=DIRECTION('center_axis',(1.,0.,0.));
#37192=DIRECTION('ref_axis',(0.,1.,0.));
#37193=DIRECTION('',(-1.,0.,0.));
#37194=DIRECTION('center_axis',(1.,0.,0.));
#37195=DIRECTION('ref_axis',(0.,1.,0.));
#37196=DIRECTION('',(-1.,0.,0.));
#37197=DIRECTION('center_axis',(1.,0.,0.));
#37198=DIRECTION('ref_axis',(0.,1.,0.));
#37199=DIRECTION('',(-1.,0.,0.));
#37200=DIRECTION('center_axis',(1.,0.,0.));
#37201=DIRECTION('ref_axis',(0.,1.,0.));
#37202=DIRECTION('',(-1.,0.,0.));
#37203=DIRECTION('center_axis',(1.,0.,0.));
#37204=DIRECTION('ref_axis',(0.,1.,0.));
#37205=DIRECTION('',(-1.,0.,0.));
#37206=DIRECTION('center_axis',(1.,0.,0.));
#37207=DIRECTION('ref_axis',(0.,1.,0.));
#37208=DIRECTION('',(-1.,0.,0.));
#37209=DIRECTION('center_axis',(1.,0.,0.));
#37210=DIRECTION('ref_axis',(0.,1.,0.));
#37211=DIRECTION('',(-1.,0.,0.));
#37212=DIRECTION('center_axis',(1.,0.,0.));
#37213=DIRECTION('ref_axis',(0.,1.,0.));
#37214=DIRECTION('center_axis',(1.,0.,0.));
#37215=DIRECTION('ref_axis',(0.,1.,6.79493845743686E-14));
#37216=DIRECTION('',(1.,0.,0.));
#37217=DIRECTION('center_axis',(1.,0.,0.));
#37218=DIRECTION('ref_axis',(0.,1.,6.79493845743686E-14));
#37219=DIRECTION('center_axis',(1.,0.,0.));
#37220=DIRECTION('ref_axis',(0.,1.,6.79493845743686E-14));
#37221=DIRECTION('',(1.,0.,0.));
#37222=DIRECTION('center_axis',(1.,0.,0.));
#37223=DIRECTION('ref_axis',(0.,1.,6.79493845743686E-14));
#37224=DIRECTION('',(1.,0.,0.));
#37225=DIRECTION('center_axis',(1.,0.,0.));
#37226=DIRECTION('ref_axis',(0.,1.,6.79493845743686E-14));
#37227=DIRECTION('',(1.,0.,0.));
#37228=DIRECTION('center_axis',(1.,0.,0.));
#37229=DIRECTION('ref_axis',(0.,1.,6.79493845743686E-14));
#37230=DIRECTION('',(1.,0.,0.));
#37231=DIRECTION('center_axis',(1.,0.,0.));
#37232=DIRECTION('ref_axis',(0.,1.,6.79493845743686E-14));
#37233=DIRECTION('',(1.,0.,0.));
#37234=DIRECTION('center_axis',(1.,0.,0.));
#37235=DIRECTION('ref_axis',(0.,1.,6.79493845743686E-14));
#37236=DIRECTION('',(1.,0.,0.));
#37237=DIRECTION('center_axis',(1.,0.,0.));
#37238=DIRECTION('ref_axis',(0.,1.,6.79493845743686E-14));
#37239=DIRECTION('',(1.,0.,0.));
#37240=DIRECTION('center_axis',(1.,0.,0.));
#37241=DIRECTION('ref_axis',(0.,1.,6.79493845743686E-14));
#37242=DIRECTION('',(1.,0.,0.));
#37243=DIRECTION('center_axis',(1.,0.,0.));
#37244=DIRECTION('ref_axis',(0.,1.,6.79493845743686E-14));
#37245=DIRECTION('',(1.,0.,0.));
#37246=DIRECTION('center_axis',(1.,0.,0.));
#37247=DIRECTION('ref_axis',(0.,1.,6.79493845743686E-14));
#37248=DIRECTION('',(1.,0.,0.));
#37249=DIRECTION('center_axis',(1.,0.,0.));
#37250=DIRECTION('ref_axis',(0.,1.,6.79493845743686E-14));
#37251=DIRECTION('',(1.,0.,0.));
#37252=DIRECTION('center_axis',(1.,0.,0.));
#37253=DIRECTION('ref_axis',(0.,0.,-1.));
#37254=DIRECTION('center_axis',(1.,0.,0.));
#37255=DIRECTION('ref_axis',(0.,1.,0.));
#37256=DIRECTION('center_axis',(1.,0.,0.));
#37257=DIRECTION('ref_axis',(0.,1.,0.));
#37258=DIRECTION('center_axis',(-1.,0.,0.));
#37259=DIRECTION('ref_axis',(0.,1.,6.79493845743686E-14));
#37260=DIRECTION('center_axis',(1.,0.,0.));
#37261=DIRECTION('ref_axis',(0.,1.,6.79493845743686E-14));
#37262=DIRECTION('center_axis',(0.,-0.5,-0.866025403784439));
#37263=DIRECTION('ref_axis',(0.,-0.866025403784439,0.5));
#37264=DIRECTION('',(-1.,0.,0.));
#37265=DIRECTION('',(0.,-0.866025403784439,0.5));
#37266=DIRECTION('',(-1.,0.,0.));
#37267=DIRECTION('center_axis',(0.,-1.,-1.60246890531964E-16));
#37268=DIRECTION('ref_axis',(0.,-1.60246890531964E-16,1.));
#37269=DIRECTION('',(0.,-1.60246890531964E-16,1.));
#37270=DIRECTION('',(-1.,0.,0.));
#37271=DIRECTION('center_axis',(0.,-0.5,0.866025403784439));
#37272=DIRECTION('ref_axis',(0.,0.866025403784439,0.5));
#37273=DIRECTION('',(0.,0.866025403784439,0.5));
#37274=DIRECTION('',(-1.,0.,0.));
#37275=DIRECTION('center_axis',(0.,0.5,0.866025403784439));
#37276=DIRECTION('ref_axis',(0.,0.866025403784439,-0.5));
#37277=DIRECTION('',(0.,0.866025403784439,-0.5));
#37278=DIRECTION('',(-1.,0.,0.));
#37279=DIRECTION('center_axis',(0.,0.5,-0.866025403784439));
#37280=DIRECTION('ref_axis',(0.,-0.866025403784439,-0.5));
#37281=DIRECTION('',(-1.,0.,0.));
#37282=DIRECTION('',(0.,-0.866025403784439,-0.5));
#37283=DIRECTION('center_axis',(0.,1.,-3.20493781063927E-16));
#37284=DIRECTION('ref_axis',(0.,-3.20493781063927E-16,-1.));
#37285=DIRECTION('',(0.,-3.20493781063927E-16,-1.));
#37286=DIRECTION('center_axis',(-1.,0.,0.));
#37287=DIRECTION('ref_axis',(0.,0.,1.));
#37288=DIRECTION('center_axis',(-1.,0.,0.));
#37289=DIRECTION('ref_axis',(0.,0.,1.));
#37290=DIRECTION('center_axis',(1.,0.,0.));
#37291=DIRECTION('ref_axis',(0.,0.,-1.));
#37292=DIRECTION('center_axis',(1.,0.,0.));
#37293=DIRECTION('ref_axis',(0.,1.,0.));
#37294=DIRECTION('',(-0.707106781186548,0.707106781186547,8.65956056235493E-17));
#37295=DIRECTION('center_axis',(1.,0.,0.));
#37296=DIRECTION('ref_axis',(0.,1.,0.));
#37297=DIRECTION('center_axis',(1.,0.,0.));
#37298=DIRECTION('ref_axis',(0.,1.,0.));
#37299=DIRECTION('center_axis',(-1.,0.,0.));
#37300=DIRECTION('ref_axis',(0.,0.,1.));
#37301=DIRECTION('center_axis',(1.,0.,0.));
#37302=DIRECTION('ref_axis',(0.,0.,-1.));
#37303=DIRECTION('',(0.,0.,1.));
#37304=DIRECTION('',(1.,0.,0.));
#37305=DIRECTION('',(0.,0.,1.));
#37306=DIRECTION('',(1.,0.,0.));
#37307=DIRECTION('',(0.,0.,1.));
#37308=DIRECTION('',(1.,0.,0.));
#37309=DIRECTION('',(0.,0.,1.));
#37310=DIRECTION('',(1.,0.,0.));
#37311=DIRECTION('',(0.,0.,-1.));
#37312=DIRECTION('',(0.,1.,0.));
#37313=DIRECTION('',(0.,0.,-1.));
#37314=DIRECTION('',(0.,1.,0.));
#37315=DIRECTION('',(0.,0.,-1.));
#37316=DIRECTION('',(0.,1.,0.));
#37317=DIRECTION('',(0.,0.,-1.));
#37318=DIRECTION('',(0.,1.,0.));
#37319=DIRECTION('',(0.,0.,-1.));
#37320=DIRECTION('',(0.,1.,0.));
#37321=DIRECTION('',(0.,0.,1.));
#37322=DIRECTION('',(1.,0.,0.));
#37323=DIRECTION('',(0.,0.,-1.));
#37324=DIRECTION('',(0.,1.,0.));
#37325=DIRECTION('',(0.,0.,-1.));
#37326=DIRECTION('',(0.,1.,0.));
#37327=DIRECTION('',(0.,0.,-1.));
#37328=DIRECTION('',(0.,1.,0.));
#37329=DIRECTION('',(0.,0.,-1.));
#37330=DIRECTION('',(0.,1.,0.));
#37331=DIRECTION('',(0.,0.,-1.));
#37332=DIRECTION('',(0.,1.,0.));
#37333=DIRECTION('',(0.,0.,1.));
#37334=DIRECTION('',(1.,0.,0.));
#37335=DIRECTION('',(0.,0.,1.));
#37336=DIRECTION('',(1.,0.,0.));
#37337=DIRECTION('',(0.,0.,-1.));
#37338=DIRECTION('',(0.,1.,0.));
#37339=DIRECTION('',(0.,0.,1.));
#37340=DIRECTION('',(0.,-1.,0.));
#37341=DIRECTION('',(0.,0.,1.));
#37342=DIRECTION('',(0.,-1.,0.));
#37343=DIRECTION('',(0.,0.,1.));
#37344=DIRECTION('',(0.,-1.,0.));
#37345=DIRECTION('',(0.,0.,1.));
#37346=DIRECTION('',(0.,-1.,0.));
#37347=DIRECTION('',(0.,0.,1.));
#37348=DIRECTION('',(0.,-1.,0.));
#37349=DIRECTION('',(0.,0.,1.));
#37350=DIRECTION('',(0.,-1.,0.));
#37351=DIRECTION('',(0.,0.,1.));
#37352=DIRECTION('',(0.,-1.,0.));
#37353=DIRECTION('',(0.,0.,1.));
#37354=DIRECTION('',(0.,-1.,0.));
#37355=DIRECTION('',(0.,0.,-1.));
#37356=DIRECTION('',(0.,1.,0.));
#37357=DIRECTION('',(0.,0.,-1.));
#37358=DIRECTION('',(0.,1.,0.));
#37359=DIRECTION('',(0.,0.,-1.));
#37360=DIRECTION('',(0.,1.,0.));
#37361=DIRECTION('',(0.,0.,-1.));
#37362=DIRECTION('',(0.,1.,0.));
#37363=DIRECTION('',(0.,1.,0.));
#37364=DIRECTION('',(0.,0.,1.));
#37365=DIRECTION('',(0.,1.,0.));
#37366=DIRECTION('',(0.,0.,1.));
#37367=DIRECTION('',(0.,0.,-1.));
#37368=DIRECTION('',(-1.,0.,0.));
#37369=DIRECTION('',(0.,0.,-1.));
#37370=DIRECTION('',(-1.,0.,0.));
#37371=DIRECTION('',(0.,0.,-1.));
#37372=DIRECTION('',(-1.,0.,0.));
#37373=DIRECTION('',(0.,0.,-1.));
#37374=DIRECTION('',(-1.,0.,0.));
#37375=CARTESIAN_POINT('',(0.,0.,0.));
#37376=CARTESIAN_POINT('',(0.,0.,0.));
#37377=CARTESIAN_POINT('Origin',(0.,46.,0.));
#37378=CARTESIAN_POINT('',(76.9075363365802,47.,50.));
#37379=CARTESIAN_POINT('',(77.2269383052313,46.,50.));
#37380=CARTESIAN_POINT('Ctrl Pts',(77.2269383052313,46.,50.));
#37381=CARTESIAN_POINT('Ctrl Pts',(77.2269383052313,46.2329198319017,50.));
#37382=CARTESIAN_POINT('Ctrl Pts',(77.1653607660612,46.5055561829699,50.));
#37383=CARTESIAN_POINT('Ctrl Pts',(77.0254295449815,46.8110812445886,50.));
#37384=CARTESIAN_POINT('Ctrl Pts',(76.9710438766786,46.9077781744567,50.));
#37385=CARTESIAN_POINT('Ctrl Pts',(76.9075363365807,46.9999999999992,50.));
#37386=CARTESIAN_POINT('',(-1.12667505521556E-14,46.,-92.));
#37387=CARTESIAN_POINT('Origin',(0.,46.,0.));
#37388=CARTESIAN_POINT('',(1.10218211923262E-14,48.,-90.));
#37389=CARTESIAN_POINT('Origin',(-1.10218211923262E-14,46.,-90.));
#37390=CARTESIAN_POINT('Origin',(0.,48.,0.));
#37391=CARTESIAN_POINT('',(-77.0527954329529,45.9999999996096,50.2679491919803));
#37392=CARTESIAN_POINT('Origin',(0.,46.,0.));
#37393=CARTESIAN_POINT('',(-75.5696311051099,47.,52.));
#37394=CARTESIAN_POINT('Ctrl Pts',(-75.5696311051099,47.,52.));
#37395=CARTESIAN_POINT('Ctrl Pts',(-75.5700201424603,47.,51.999434626749));
#37396=CARTESIAN_POINT('Ctrl Pts',(-75.570409287503,46.9999997602648,51.9988693275745));
#37397=CARTESIAN_POINT('Ctrl Pts',(-75.5720130884468,46.9999977855239,51.9965404836838));
#37398=CARTESIAN_POINT('Ctrl Pts',(-75.5732286826425,46.9999939579146,51.994777587995));
#37399=CARTESIAN_POINT('Ctrl Pts',(-75.5765121990975,46.999977349045,51.9900217507738));
#37400=CARTESIAN_POINT('Ctrl Pts',(-75.5785820799728,46.9999601799197,51.9870301822449));
#37401=CARTESIAN_POINT('Ctrl Pts',(-75.5887090256785,46.9998436332333,51.972425137894));
#37402=CARTESIAN_POINT('Ctrl Pts',(-75.5968078544418,46.9996500011623,51.9608415795779));
#37403=CARTESIAN_POINT('Ctrl Pts',(-75.6621771593858,46.997297854563,51.8681016030327));
#37404=CARTESIAN_POINT('Ctrl Pts',(-75.7215624039282,46.9903378312819,51.7885093232287));
#37405=CARTESIAN_POINT('Ctrl Pts',(-75.9151544327206,46.9541413446516,51.540847638037));
#37406=CARTESIAN_POINT('Ctrl Pts',(-76.0564163554542,46.9079528904244,51.3776580388172));
#37407=CARTESIAN_POINT('Ctrl Pts',(-76.4041124085987,46.7468902883554,50.9947551668813));
#37408=CARTESIAN_POINT('Ctrl Pts',(-76.6102052861138,46.6079794397508,50.7845705159268));
#37409=CARTESIAN_POINT('Ctrl Pts',(-76.8970989561146,46.3036584894847,50.4719619095292));
#37410=CARTESIAN_POINT('Ctrl Pts',(-76.9933165723146,46.1579139502934,50.3591208541419));
#37411=CARTESIAN_POINT('Ctrl Pts',(-77.0527954326587,46.0000000000002,50.2679491924312));
#37412=CARTESIAN_POINT('Origin',(0.,47.,0.));
#37413=CARTESIAN_POINT('Origin',(0.,24.,0.));
#37414=CARTESIAN_POINT('',(77.2269383052313,2.,50.));
#37415=CARTESIAN_POINT('',(77.2269383052313,24.,50.));
#37416=CARTESIAN_POINT('',(43.1452924241198,2.,-81.2556689815375));
#37417=CARTESIAN_POINT('Origin',(0.,2.,0.));
#37418=CARTESIAN_POINT('',(39.,2.,-83.3246662159531));
#37419=CARTESIAN_POINT('Origin',(0.,2.,0.));
#37420=CARTESIAN_POINT('',(45.,8.,-80.2433797892387));
#37421=CARTESIAN_POINT('Ctrl Pts',(39.,2.,-83.3246662159531));
#37422=CARTESIAN_POINT('Ctrl Pts',(39.7682076868648,2.,-82.965107622462));
#37423=CARTESIAN_POINT('Ctrl Pts',(40.5861518890197,2.1556365878507,-82.5680240102596));
#37424=CARTESIAN_POINT('Ctrl Pts',(42.0962197288883,2.79558990411642,-81.8084506557891));
#37425=CARTESIAN_POINT('Ctrl Pts',(42.7886063451273,3.27986145745522,-81.4464457673431));
#37426=CARTESIAN_POINT('Ctrl Pts',(43.825446345948,4.36512188826461,-80.8927389962394));
#37427=CARTESIAN_POINT('Ctrl Pts',(44.2621585987635,5.01413618672815,-80.6534196360022));
#37428=CARTESIAN_POINT('Ctrl Pts',(44.8497980701861,6.45547542071794,-80.3281295509505));
#37429=CARTESIAN_POINT('Ctrl Pts',(45.,7.24837120717834,-80.2433797892387));
#37430=CARTESIAN_POINT('Ctrl Pts',(45.,8.00000000000001,-80.2433797892387));
#37431=CARTESIAN_POINT('',(45.,36.,-80.2433797892387));
#37432=CARTESIAN_POINT('',(45.,24.,-80.2433797892387));
#37433=CARTESIAN_POINT('',(39.,42.,-83.3246662159531));
#37434=CARTESIAN_POINT('Ctrl Pts',(45.,36.,-80.2433797892387));
#37435=CARTESIAN_POINT('Ctrl Pts',(45.,36.7516287928217,-80.2433797892387));
#37436=CARTESIAN_POINT('Ctrl Pts',(44.8497980701861,37.5445245792821,-80.3281295509505));
#37437=CARTESIAN_POINT('Ctrl Pts',(44.2621585987635,38.9858638132718,-80.6534196360022));
#37438=CARTESIAN_POINT('Ctrl Pts',(43.8254463459479,39.6348781117354,-80.8927389962394));
#37439=CARTESIAN_POINT('Ctrl Pts',(42.7886063451273,40.7201385425448,-81.4464457673431));
#37440=CARTESIAN_POINT('Ctrl Pts',(42.0962197288883,41.2044100958836,-81.8084506557891));
#37441=CARTESIAN_POINT('Ctrl Pts',(40.5861518890197,41.8443634121493,-82.5680240102596));
#37442=CARTESIAN_POINT('Ctrl Pts',(39.7682076868648,42.,-82.965107622462));
#37443=CARTESIAN_POINT('Ctrl Pts',(39.,42.,-83.3246662159531));
#37444=CARTESIAN_POINT('',(-39.,42.,-83.3246662159531));
#37445=CARTESIAN_POINT('Origin',(0.,42.,0.));
#37446=CARTESIAN_POINT('',(-45.,36.,-80.2433797892387));
#37447=CARTESIAN_POINT('Ctrl Pts',(-39.,42.,-83.3246662159531));
#37448=CARTESIAN_POINT('Ctrl Pts',(-39.7682076868648,42.,-82.965107622462));
#37449=CARTESIAN_POINT('Ctrl Pts',(-40.5861518890197,41.8443634121493,-82.5680240102596));
#37450=CARTESIAN_POINT('Ctrl Pts',(-42.0962197288883,41.2044100958836,-81.8084506557891));
#37451=CARTESIAN_POINT('Ctrl Pts',(-42.7886063451273,40.7201385425448,-81.4464457673431));
#37452=CARTESIAN_POINT('Ctrl Pts',(-43.8254463459479,39.6348781117354,-80.8927389962394));
#37453=CARTESIAN_POINT('Ctrl Pts',(-44.2621585987635,38.9858638132719,-80.6534196360022));
#37454=CARTESIAN_POINT('Ctrl Pts',(-44.8497980701861,37.5445245792821,-80.3281295509504));
#37455=CARTESIAN_POINT('Ctrl Pts',(-45.,36.7516287928217,-80.2433797892387));
#37456=CARTESIAN_POINT('Ctrl Pts',(-45.,36.,-80.2433797892387));
#37457=CARTESIAN_POINT('',(-45.,8.,-80.2433797892387));
#37458=CARTESIAN_POINT('',(-45.,24.,-80.2433797892387));
#37459=CARTESIAN_POINT('',(-39.,2.,-83.3246662159531));
#37460=CARTESIAN_POINT('Ctrl Pts',(-45.,8.00000000000001,-80.2433797892387));
#37461=CARTESIAN_POINT('Ctrl Pts',(-45.,7.24837120717834,-80.2433797892387));
#37462=CARTESIAN_POINT('Ctrl Pts',(-44.8497980701861,6.45547542071794,-80.3281295509505));
#37463=CARTESIAN_POINT('Ctrl Pts',(-44.2621585987635,5.01413618672815,-80.6534196360022));
#37464=CARTESIAN_POINT('Ctrl Pts',(-43.8254463459479,4.36512188826461,-80.8927389962394));
#37465=CARTESIAN_POINT('Ctrl Pts',(-42.7886063451273,3.27986145745522,-81.4464457673431));
#37466=CARTESIAN_POINT('Ctrl Pts',(-42.0962197288883,2.79558990411642,-81.8084506557891));
#37467=CARTESIAN_POINT('Ctrl Pts',(-40.5861518890197,2.1556365878507,-82.5680240102596));
#37468=CARTESIAN_POINT('Ctrl Pts',(-39.7682076868648,2.,-82.965107622462));
#37469=CARTESIAN_POINT('Ctrl Pts',(-39.,2.,-83.3246662159531));
#37470=CARTESIAN_POINT('',(-75.8946638440411,2.,52.));
#37471=CARTESIAN_POINT('Origin',(0.,2.,0.));
#37472=CARTESIAN_POINT('',(-77.2269383052313,4.,50.));
#37473=CARTESIAN_POINT('Ctrl Pts',(-75.8946638440411,2.,52.));
#37474=CARTESIAN_POINT('Ctrl Pts',(-76.0674525460939,2.,51.7478126834933));
#37475=CARTESIAN_POINT('Ctrl Pts',(-76.2523381437454,2.05028979164384,51.4749989417307));
#37476=CARTESIAN_POINT('Ctrl Pts',(-76.5947876563318,2.26685914288403,50.9640372439704));
#37477=CARTESIAN_POINT('Ctrl Pts',(-76.7523839779586,2.43326063418965,50.7259626978856));
#37478=CARTESIAN_POINT('Ctrl Pts',(-76.9789947123575,2.80370034162261,50.3812329006827));
#37479=CARTESIAN_POINT('Ctrl Pts',(-77.0709575562652,3.01592897574302,50.2402273896437));
#37480=CARTESIAN_POINT('Ctrl Pts',(-77.1949935065466,3.48961682480797,50.0494348028582));
#37481=CARTESIAN_POINT('Ctrl Pts',(-77.2269383052313,3.75125143583077,50.));
#37482=CARTESIAN_POINT('Ctrl Pts',(-77.2269383052313,4.,50.));
#37483=CARTESIAN_POINT('',(-77.2269383052313,45.,50.));
#37484=CARTESIAN_POINT('',(-77.2269383052313,24.,50.));
#37485=CARTESIAN_POINT('Ctrl Pts',(-77.2269383052313,45.,50.));
#37486=CARTESIAN_POINT('Ctrl Pts',(-77.2269383052313,45.2487485641692,50.));
#37487=CARTESIAN_POINT('Ctrl Pts',(-77.1949935065466,45.510383175192,50.0494348028582));
#37488=CARTESIAN_POINT('Ctrl Pts',(-77.109956799136,45.8351346277627,50.1802386008037));
#37489=CARTESIAN_POINT('Ctrl Pts',(-77.082972874874,45.919880120673,50.2216919585661));
#37490=CARTESIAN_POINT('Ctrl Pts',(-77.0527954328532,45.9999999994838,50.2679491921331));
#37491=CARTESIAN_POINT('Origin',(0.,48.,0.));
#37492=CARTESIAN_POINT('',(-46.0621933088198,48.,-41.0121933088198));
#37493=CARTESIAN_POINT('Origin',(-41.0121933088198,48.,-41.0121933088198));
#37494=CARTESIAN_POINT('',(-46.0621933088198,48.,41.0121933088198));
#37495=CARTESIAN_POINT('Origin',(-41.0121933088198,48.,41.0121933088198));
#37496=CARTESIAN_POINT('',(35.9621933088198,48.,41.0121933088198));
#37497=CARTESIAN_POINT('Origin',(41.0121933088198,48.,41.0121933088198));
#37498=CARTESIAN_POINT('',(35.9621933088197,48.,-41.0121933088198));
#37499=CARTESIAN_POINT('Origin',(41.0121933088197,48.,-41.0121933088198));
#37500=CARTESIAN_POINT('',(1.59204083889156E-15,48.,-13.));
#37501=CARTESIAN_POINT('Origin',(0.,48.,0.));
#37502=CARTESIAN_POINT('Origin',(0.,2.,0.));
#37503=CARTESIAN_POINT('',(42.207351284465,1.66533453693773E-15,-79.4892413949823));
#37504=CARTESIAN_POINT('Origin',(42.207351284465,2.,-79.4892413949823));
#37505=CARTESIAN_POINT('Origin',(0.,1.66533453693773E-15,0.));
#37506=CARTESIAN_POINT('Origin',(0.,2.,0.));
#37507=CARTESIAN_POINT('Origin',(0.,2.,0.));
#37508=CARTESIAN_POINT('Origin',(0.,0.,91.));
#37509=CARTESIAN_POINT('',(26.3300414539374,0.,-75.7581216659255));
#37510=CARTESIAN_POINT('Origin',(31.3800414539374,0.,-75.7581216659255));
#37511=CARTESIAN_POINT('',(-80.8081216659255,0.,-31.3800414539373));
#37512=CARTESIAN_POINT('Origin',(-75.7581216659255,0.,-31.3800414539373));
#37513=CARTESIAN_POINT('',(-80.8081216659255,0.,31.3800414539374));
#37514=CARTESIAN_POINT('Origin',(-75.7581216659255,0.,31.3800414539374));
#37515=CARTESIAN_POINT('',(26.3300414539374,0.,75.7581216659255));
#37516=CARTESIAN_POINT('Origin',(31.3800414539374,0.,75.7581216659255));
#37517=CARTESIAN_POINT('',(-36.4300414539374,0.,75.7581216659255));
#37518=CARTESIAN_POINT('Origin',(-31.3800414539374,0.,75.7581216659255));
#37519=CARTESIAN_POINT('',(70.7081216659255,0.,31.3800414539374));
#37520=CARTESIAN_POINT('Origin',(75.7581216659255,0.,31.3800414539374));
#37521=CARTESIAN_POINT('',(-36.4300414539373,0.,-75.7581216659255));
#37522=CARTESIAN_POINT('Origin',(-31.3800414539373,0.,-75.7581216659255));
#37523=CARTESIAN_POINT('',(70.7081216659255,0.,-31.3800414539373));
#37524=CARTESIAN_POINT('Origin',(75.7581216659255,0.,-31.3800414539373));
#37525=CARTESIAN_POINT('',(8.84194988984389E-15,0.,-72.2));
#37526=CARTESIAN_POINT('Origin',(0.,0.,0.));
#37527=CARTESIAN_POINT('Origin',(-73.,28.,-138.));
#37528=CARTESIAN_POINT('',(-75.,41.,-138.));
#37529=CARTESIAN_POINT('',(-73.,41.,-140.));
#37530=CARTESIAN_POINT('Origin',(-73.,41.,-138.));
#37531=CARTESIAN_POINT('',(-73.,-11.,-140.));
#37532=CARTESIAN_POINT('',(-73.,28.,-140.));
#37533=CARTESIAN_POINT('',(-75.,-11.,-138.));
#37534=CARTESIAN_POINT('Origin',(-73.,-11.,-138.));
#37535=CARTESIAN_POINT('',(-75.,28.,-138.));
#37536=CARTESIAN_POINT('Ctrl Pts',(-73.,-11.,-140.));
#37537=CARTESIAN_POINT('Ctrl Pts',(-73.,-13.,-140.));
#37538=CARTESIAN_POINT('Ctrl Pts',(-71.,-13.,-140.));
#37539=CARTESIAN_POINT('Ctrl Pts',(-75.,-11.,-140.));
#37540=CARTESIAN_POINT('Ctrl Pts',(-75.,-15.,-140.));
#37541=CARTESIAN_POINT('Ctrl Pts',(-71.,-15.,-140.));
#37542=CARTESIAN_POINT('Ctrl Pts',(-75.,-11.,-138.));
#37543=CARTESIAN_POINT('Ctrl Pts',(-75.,-15.,-138.));
#37544=CARTESIAN_POINT('Ctrl Pts',(-71.,-15.,-138.));
#37545=CARTESIAN_POINT('',(-71.,-13.,-140.));
#37546=CARTESIAN_POINT('',(-71.,-15.,-138.));
#37547=CARTESIAN_POINT('Origin',(-71.,-13.,-138.));
#37548=CARTESIAN_POINT('Origin',(-71.,-11.,-138.));
#37549=CARTESIAN_POINT('Origin',(-71.,-11.,-140.));
#37550=CARTESIAN_POINT('Origin',(-35.5,-13.,-138.));
#37551=CARTESIAN_POINT('',(71.,-13.,-140.));
#37552=CARTESIAN_POINT('',(71.,-15.,-138.));
#37553=CARTESIAN_POINT('Origin',(71.,-13.,-138.));
#37554=CARTESIAN_POINT('',(-35.5,-15.,-138.));
#37555=CARTESIAN_POINT('',(-35.5,-13.,-140.));
#37556=CARTESIAN_POINT('Ctrl Pts',(71.,-13.,-140.));
#37557=CARTESIAN_POINT('Ctrl Pts',(73.,-13.,-140.));
#37558=CARTESIAN_POINT('Ctrl Pts',(73.,-11.,-140.));
#37559=CARTESIAN_POINT('Ctrl Pts',(71.,-15.,-140.));
#37560=CARTESIAN_POINT('Ctrl Pts',(75.,-15.,-140.));
#37561=CARTESIAN_POINT('Ctrl Pts',(75.,-11.,-140.));
#37562=CARTESIAN_POINT('Ctrl Pts',(71.,-15.,-138.));
#37563=CARTESIAN_POINT('Ctrl Pts',(75.,-15.,-138.));
#37564=CARTESIAN_POINT('Ctrl Pts',(75.,-11.,-138.));
#37565=CARTESIAN_POINT('',(73.,-11.,-140.));
#37566=CARTESIAN_POINT('',(75.,-11.,-138.));
#37567=CARTESIAN_POINT('Origin',(73.,-11.,-138.));
#37568=CARTESIAN_POINT('Origin',(71.,-11.,-138.));
#37569=CARTESIAN_POINT('Origin',(71.,-11.,-140.));
#37570=CARTESIAN_POINT('Origin',(73.,2.,-138.));
#37571=CARTESIAN_POINT('',(73.,41.,-140.));
#37572=CARTESIAN_POINT('',(75.,41.,-138.));
#37573=CARTESIAN_POINT('Origin',(73.,41.,-138.));
#37574=CARTESIAN_POINT('',(75.,2.,-138.));
#37575=CARTESIAN_POINT('',(73.,2.,-140.));
#37576=CARTESIAN_POINT('Ctrl Pts',(73.,41.,-140.));
#37577=CARTESIAN_POINT('Ctrl Pts',(73.,43.,-140.));
#37578=CARTESIAN_POINT('Ctrl Pts',(71.,43.,-140.));
#37579=CARTESIAN_POINT('Ctrl Pts',(75.,41.,-140.));
#37580=CARTESIAN_POINT('Ctrl Pts',(75.,45.,-140.));
#37581=CARTESIAN_POINT('Ctrl Pts',(71.,45.,-140.));
#37582=CARTESIAN_POINT('Ctrl Pts',(75.,41.,-138.));
#37583=CARTESIAN_POINT('Ctrl Pts',(75.,45.,-138.));
#37584=CARTESIAN_POINT('Ctrl Pts',(71.,45.,-138.));
#37585=CARTESIAN_POINT('',(71.,43.,-140.));
#37586=CARTESIAN_POINT('',(71.,45.,-138.));
#37587=CARTESIAN_POINT('Origin',(71.,43.,-138.));
#37588=CARTESIAN_POINT('Origin',(71.,41.,-138.));
#37589=CARTESIAN_POINT('Origin',(71.,41.,-140.));
#37590=CARTESIAN_POINT('Origin',(35.5,43.,-138.));
#37591=CARTESIAN_POINT('',(-71.,43.,-140.));
#37592=CARTESIAN_POINT('',(-71.,45.,-138.));
#37593=CARTESIAN_POINT('Origin',(-71.,43.,-138.));
#37594=CARTESIAN_POINT('',(35.5,45.,-138.));
#37595=CARTESIAN_POINT('',(35.5,43.,-140.));
#37596=CARTESIAN_POINT('Ctrl Pts',(-71.,43.,-140.));
#37597=CARTESIAN_POINT('Ctrl Pts',(-73.,43.,-140.));
#37598=CARTESIAN_POINT('Ctrl Pts',(-73.,41.,-140.));
#37599=CARTESIAN_POINT('Ctrl Pts',(-71.,45.,-140.));
#37600=CARTESIAN_POINT('Ctrl Pts',(-75.,45.,-140.));
#37601=CARTESIAN_POINT('Ctrl Pts',(-75.,41.,-140.));
#37602=CARTESIAN_POINT('Ctrl Pts',(-71.,45.,-138.));
#37603=CARTESIAN_POINT('Ctrl Pts',(-75.,45.,-138.));
#37604=CARTESIAN_POINT('Ctrl Pts',(-75.,41.,-138.));
#37605=CARTESIAN_POINT('Origin',(-71.,41.,-138.));
#37606=CARTESIAN_POINT('Origin',(-71.,41.,-140.));
#37607=CARTESIAN_POINT('Origin',(71.,41.,-140.));
#37608=CARTESIAN_POINT('',(71.,45.,-127.));
#37609=CARTESIAN_POINT('',(71.,45.,-140.));
#37610=CARTESIAN_POINT('',(75.,41.,-127.));
#37611=CARTESIAN_POINT('Origin',(71.,41.,-127.));
#37612=CARTESIAN_POINT('',(75.,41.,-140.));
#37613=CARTESIAN_POINT('Origin',(71.,45.,-140.));
#37614=CARTESIAN_POINT('',(-71.,45.,-127.));
#37615=CARTESIAN_POINT('',(-71.,45.,-140.));
#37616=CARTESIAN_POINT('',(35.5,45.,-127.));
#37617=CARTESIAN_POINT('Origin',(-71.,41.,-140.));
#37618=CARTESIAN_POINT('',(-75.,41.,-127.));
#37619=CARTESIAN_POINT('',(-75.,41.,-140.));
#37620=CARTESIAN_POINT('Origin',(-71.,41.,-127.));
#37621=CARTESIAN_POINT('Origin',(-75.,41.,-140.));
#37622=CARTESIAN_POINT('',(-75.,-11.,-127.));
#37623=CARTESIAN_POINT('',(-75.,-11.,-140.));
#37624=CARTESIAN_POINT('',(-75.,28.,-127.));
#37625=CARTESIAN_POINT('Origin',(0.,15.,-140.));
#37626=CARTESIAN_POINT('',(53.,15.,-140.));
#37627=CARTESIAN_POINT('Origin',(60.,15.,-140.));
#37628=CARTESIAN_POINT('',(-67.,15.,-140.));
#37629=CARTESIAN_POINT('Origin',(-60.,15.,-140.));
#37630=CARTESIAN_POINT('Origin',(-35.5,-13.,-127.));
#37631=CARTESIAN_POINT('',(-71.,-13.,-125.));
#37632=CARTESIAN_POINT('',(-71.,-15.,-127.));
#37633=CARTESIAN_POINT('Origin',(-71.,-13.,-127.));
#37634=CARTESIAN_POINT('',(71.,-15.,-127.));
#37635=CARTESIAN_POINT('',(-35.5,-15.,-127.));
#37636=CARTESIAN_POINT('',(71.,-13.,-125.));
#37637=CARTESIAN_POINT('Origin',(71.,-13.,-127.));
#37638=CARTESIAN_POINT('',(-35.5,-13.,-125.));
#37639=CARTESIAN_POINT('Ctrl Pts',(71.,-15.,-127.));
#37640=CARTESIAN_POINT('Ctrl Pts',(75.,-15.,-127.));
#37641=CARTESIAN_POINT('Ctrl Pts',(75.,-11.,-127.));
#37642=CARTESIAN_POINT('Ctrl Pts',(71.,-15.,-125.));
#37643=CARTESIAN_POINT('Ctrl Pts',(75.,-15.,-125.));
#37644=CARTESIAN_POINT('Ctrl Pts',(75.,-11.,-125.));
#37645=CARTESIAN_POINT('Ctrl Pts',(71.,-13.,-125.));
#37646=CARTESIAN_POINT('Ctrl Pts',(73.,-13.,-125.));
#37647=CARTESIAN_POINT('Ctrl Pts',(73.,-11.,-125.));
#37648=CARTESIAN_POINT('',(75.,-11.,-127.));
#37649=CARTESIAN_POINT('',(73.,-11.,-125.));
#37650=CARTESIAN_POINT('Origin',(73.,-11.,-127.));
#37651=CARTESIAN_POINT('Origin',(71.,-11.,-125.));
#37652=CARTESIAN_POINT('Origin',(71.,-11.,-127.));
#37653=CARTESIAN_POINT('Origin',(73.,2.,-127.));
#37654=CARTESIAN_POINT('',(73.,41.,-125.));
#37655=CARTESIAN_POINT('Origin',(73.,41.,-127.));
#37656=CARTESIAN_POINT('',(73.,2.,-125.));
#37657=CARTESIAN_POINT('',(75.,2.,-127.));
#37658=CARTESIAN_POINT('Ctrl Pts',(75.,41.,-127.));
#37659=CARTESIAN_POINT('Ctrl Pts',(75.,45.,-127.));
#37660=CARTESIAN_POINT('Ctrl Pts',(71.,45.,-127.));
#37661=CARTESIAN_POINT('Ctrl Pts',(75.,41.,-125.));
#37662=CARTESIAN_POINT('Ctrl Pts',(75.,45.,-125.));
#37663=CARTESIAN_POINT('Ctrl Pts',(71.,45.,-125.));
#37664=CARTESIAN_POINT('Ctrl Pts',(73.,41.,-125.));
#37665=CARTESIAN_POINT('Ctrl Pts',(73.,43.,-125.));
#37666=CARTESIAN_POINT('Ctrl Pts',(71.,43.,-125.));
#37667=CARTESIAN_POINT('',(71.,43.,-125.));
#37668=CARTESIAN_POINT('Origin',(71.,43.,-127.));
#37669=CARTESIAN_POINT('Origin',(71.,41.,-125.));
#37670=CARTESIAN_POINT('Origin',(35.5,43.,-127.));
#37671=CARTESIAN_POINT('',(-71.,43.,-125.));
#37672=CARTESIAN_POINT('Origin',(-71.,43.,-127.));
#37673=CARTESIAN_POINT('',(35.5,43.,-125.));
#37674=CARTESIAN_POINT('Ctrl Pts',(-71.,45.,-127.));
#37675=CARTESIAN_POINT('Ctrl Pts',(-75.,45.,-127.));
#37676=CARTESIAN_POINT('Ctrl Pts',(-75.,41.,-127.));
#37677=CARTESIAN_POINT('Ctrl Pts',(-71.,45.,-125.));
#37678=CARTESIAN_POINT('Ctrl Pts',(-75.,45.,-125.));
#37679=CARTESIAN_POINT('Ctrl Pts',(-75.,41.,-125.));
#37680=CARTESIAN_POINT('Ctrl Pts',(-71.,43.,-125.));
#37681=CARTESIAN_POINT('Ctrl Pts',(-73.,43.,-125.));
#37682=CARTESIAN_POINT('Ctrl Pts',(-73.,41.,-125.));
#37683=CARTESIAN_POINT('',(-73.,41.,-125.));
#37684=CARTESIAN_POINT('Origin',(-73.,41.,-127.));
#37685=CARTESIAN_POINT('Origin',(-71.,41.,-125.));
#37686=CARTESIAN_POINT('Origin',(-73.,28.,-127.));
#37687=CARTESIAN_POINT('',(-73.,-11.,-125.));
#37688=CARTESIAN_POINT('Origin',(-73.,-11.,-127.));
#37689=CARTESIAN_POINT('',(-73.,28.,-125.));
#37690=CARTESIAN_POINT('Ctrl Pts',(-75.,-11.,-127.));
#37691=CARTESIAN_POINT('Ctrl Pts',(-75.,-15.,-127.));
#37692=CARTESIAN_POINT('Ctrl Pts',(-71.,-15.,-127.));
#37693=CARTESIAN_POINT('Ctrl Pts',(-75.,-11.,-125.));
#37694=CARTESIAN_POINT('Ctrl Pts',(-75.,-15.,-125.));
#37695=CARTESIAN_POINT('Ctrl Pts',(-71.,-15.,-125.));
#37696=CARTESIAN_POINT('Ctrl Pts',(-73.,-11.,-125.));
#37697=CARTESIAN_POINT('Ctrl Pts',(-73.,-13.,-125.));
#37698=CARTESIAN_POINT('Ctrl Pts',(-71.,-13.,-125.));
#37699=CARTESIAN_POINT('Origin',(-71.,-11.,-125.));
#37700=CARTESIAN_POINT('Origin',(-71.,-11.,-127.));
#37701=CARTESIAN_POINT('Origin',(75.,-11.,-140.));
#37702=CARTESIAN_POINT('',(75.,-11.,-140.));
#37703=CARTESIAN_POINT('Origin',(71.,-11.,-140.));
#37704=CARTESIAN_POINT('',(71.,-15.,-140.));
#37705=CARTESIAN_POINT('Origin',(-71.,-15.,-140.));
#37706=CARTESIAN_POINT('',(-71.,-15.,-140.));
#37707=CARTESIAN_POINT('Origin',(0.,15.,-125.));
#37708=CARTESIAN_POINT('',(39.,2.,-125.));
#37709=CARTESIAN_POINT('',(45.,8.,-125.));
#37710=CARTESIAN_POINT('Origin',(39.,8.00000000000001,-125.));
#37711=CARTESIAN_POINT('',(-39.,2.,-125.));
#37712=CARTESIAN_POINT('',(-39.,2.,-125.));
#37713=CARTESIAN_POINT('',(-45.,8.,-125.));
#37714=CARTESIAN_POINT('Origin',(-39.,8.00000000000001,-125.));
#37715=CARTESIAN_POINT('',(-45.,36.,-125.));
#37716=CARTESIAN_POINT('',(-45.,36.,-125.));
#37717=CARTESIAN_POINT('',(-39.,42.,-125.));
#37718=CARTESIAN_POINT('Origin',(-39.,36.,-125.));
#37719=CARTESIAN_POINT('',(39.,42.,-125.));
#37720=CARTESIAN_POINT('',(39.,42.,-125.));
#37721=CARTESIAN_POINT('',(45.,36.,-125.));
#37722=CARTESIAN_POINT('Origin',(39.,36.,-125.));
#37723=CARTESIAN_POINT('',(45.,8.,-125.));
#37724=CARTESIAN_POINT('',(53.,15.,-125.));
#37725=CARTESIAN_POINT('Origin',(60.,15.,-125.));
#37726=CARTESIAN_POINT('',(-67.,15.,-125.));
#37727=CARTESIAN_POINT('Origin',(-60.,15.,-125.));
#37728=CARTESIAN_POINT('Origin',(-52.,27.5,112.));
#37729=CARTESIAN_POINT('',(-52.,30.5,114.));
#37730=CARTESIAN_POINT('',(-54.,30.5,112.));
#37731=CARTESIAN_POINT('Origin',(-52.,30.5,112.));
#37732=CARTESIAN_POINT('',(-54.,18.5,112.));
#37733=CARTESIAN_POINT('',(-54.,27.5,112.));
#37734=CARTESIAN_POINT('',(-52.,18.5,114.));
#37735=CARTESIAN_POINT('Origin',(-52.,18.5,112.));
#37736=CARTESIAN_POINT('',(-52.,27.5,114.));
#37737=CARTESIAN_POINT('Ctrl Pts',(-54.,18.5,112.));
#37738=CARTESIAN_POINT('Ctrl Pts',(-54.,15.5,112.));
#37739=CARTESIAN_POINT('Ctrl Pts',(-51.,15.5,112.));
#37740=CARTESIAN_POINT('Ctrl Pts',(-54.,18.5,114.));
#37741=CARTESIAN_POINT('Ctrl Pts',(-54.,15.5,114.));
#37742=CARTESIAN_POINT('Ctrl Pts',(-51.,15.5,114.));
#37743=CARTESIAN_POINT('Ctrl Pts',(-52.,18.5,114.));
#37744=CARTESIAN_POINT('Ctrl Pts',(-52.,17.5,114.));
#37745=CARTESIAN_POINT('Ctrl Pts',(-51.,17.5,114.));
#37746=CARTESIAN_POINT('',(-51.,15.5,112.));
#37747=CARTESIAN_POINT('',(-51.,17.5,114.));
#37748=CARTESIAN_POINT('Origin',(-51.,17.5,112.));
#37749=CARTESIAN_POINT('Origin',(-51.,18.5,114.));
#37750=CARTESIAN_POINT('Origin',(-51.,18.5,112.));
#37751=CARTESIAN_POINT('Origin',(-48.,17.5,112.));
#37752=CARTESIAN_POINT('',(-39.,15.5,112.));
#37753=CARTESIAN_POINT('',(-39.,17.5,114.));
#37754=CARTESIAN_POINT('Origin',(-39.,17.5,112.));
#37755=CARTESIAN_POINT('',(-48.,17.5,114.));
#37756=CARTESIAN_POINT('',(-48.,15.5,112.));
#37757=CARTESIAN_POINT('Ctrl Pts',(-39.,15.5,112.));
#37758=CARTESIAN_POINT('Ctrl Pts',(-36.,15.5,112.));
#37759=CARTESIAN_POINT('Ctrl Pts',(-36.,18.5,112.));
#37760=CARTESIAN_POINT('Ctrl Pts',(-39.,15.5,114.));
#37761=CARTESIAN_POINT('Ctrl Pts',(-36.,15.5,114.));
#37762=CARTESIAN_POINT('Ctrl Pts',(-36.,18.5,114.));
#37763=CARTESIAN_POINT('Ctrl Pts',(-39.,17.5,114.));
#37764=CARTESIAN_POINT('Ctrl Pts',(-38.,17.5,114.));
#37765=CARTESIAN_POINT('Ctrl Pts',(-38.,18.5,114.));
#37766=CARTESIAN_POINT('',(-36.,18.5,112.));
#37767=CARTESIAN_POINT('',(-38.,18.5,114.));
#37768=CARTESIAN_POINT('Origin',(-38.,18.5,112.));
#37769=CARTESIAN_POINT('Origin',(-39.,18.5,114.));
#37770=CARTESIAN_POINT('Origin',(-39.,18.5,112.));
#37771=CARTESIAN_POINT('Origin',(-38.,21.5,112.));
#37772=CARTESIAN_POINT('',(-36.,30.5,112.));
#37773=CARTESIAN_POINT('',(-38.,30.5,114.));
#37774=CARTESIAN_POINT('Origin',(-38.,30.5,112.));
#37775=CARTESIAN_POINT('',(-38.,21.5,114.));
#37776=CARTESIAN_POINT('',(-36.,21.5,112.));
#37777=CARTESIAN_POINT('Ctrl Pts',(-36.,30.5,112.));
#37778=CARTESIAN_POINT('Ctrl Pts',(-36.,33.5,112.));
#37779=CARTESIAN_POINT('Ctrl Pts',(-39.,33.5,112.));
#37780=CARTESIAN_POINT('Ctrl Pts',(-36.,30.5,114.));
#37781=CARTESIAN_POINT('Ctrl Pts',(-36.,33.5,114.));
#37782=CARTESIAN_POINT('Ctrl Pts',(-39.,33.5,114.));
#37783=CARTESIAN_POINT('Ctrl Pts',(-38.,30.5,114.));
#37784=CARTESIAN_POINT('Ctrl Pts',(-38.,31.5,114.));
#37785=CARTESIAN_POINT('Ctrl Pts',(-39.,31.5,114.));
#37786=CARTESIAN_POINT('',(-39.,33.5,112.));
#37787=CARTESIAN_POINT('',(-39.,31.5,114.));
#37788=CARTESIAN_POINT('Origin',(-39.,31.5,112.));
#37789=CARTESIAN_POINT('Origin',(-39.,30.5,114.));
#37790=CARTESIAN_POINT('Origin',(-39.,30.5,112.));
#37791=CARTESIAN_POINT('Origin',(-42.,31.5,112.));
#37792=CARTESIAN_POINT('',(-51.,33.5,112.));
#37793=CARTESIAN_POINT('',(-51.,31.5,114.));
#37794=CARTESIAN_POINT('Origin',(-51.,31.5,112.));
#37795=CARTESIAN_POINT('',(-42.,31.5,114.));
#37796=CARTESIAN_POINT('',(-42.,33.5,112.));
#37797=CARTESIAN_POINT('Ctrl Pts',(-51.,33.5,112.));
#37798=CARTESIAN_POINT('Ctrl Pts',(-54.,33.5,112.));
#37799=CARTESIAN_POINT('Ctrl Pts',(-54.,30.5,112.));
#37800=CARTESIAN_POINT('Ctrl Pts',(-51.,33.5,114.));
#37801=CARTESIAN_POINT('Ctrl Pts',(-54.,33.5,114.));
#37802=CARTESIAN_POINT('Ctrl Pts',(-54.,30.5,114.));
#37803=CARTESIAN_POINT('Ctrl Pts',(-51.,31.5,114.));
#37804=CARTESIAN_POINT('Ctrl Pts',(-52.,31.5,114.));
#37805=CARTESIAN_POINT('Ctrl Pts',(-52.,30.5,114.));
#37806=CARTESIAN_POINT('Origin',(-51.,30.5,114.));
#37807=CARTESIAN_POINT('Origin',(-51.,30.5,112.));
#37808=CARTESIAN_POINT('Origin',(-39.,18.5,110.));
#37809=CARTESIAN_POINT('',(-39.,15.5,110.));
#37810=CARTESIAN_POINT('',(-39.,15.5,110.));
#37811=CARTESIAN_POINT('',(-36.,18.5,110.));
#37812=CARTESIAN_POINT('Origin',(-39.,18.5,110.));
#37813=CARTESIAN_POINT('',(-36.,18.5,110.));
#37814=CARTESIAN_POINT('Origin',(-51.,15.5,110.));
#37815=CARTESIAN_POINT('',(-51.,15.5,110.));
#37816=CARTESIAN_POINT('',(-51.,15.5,110.));
#37817=CARTESIAN_POINT('',(-25.5,15.5,110.));
#37818=CARTESIAN_POINT('Origin',(-51.,18.5,110.));
#37819=CARTESIAN_POINT('',(-54.,18.5,110.));
#37820=CARTESIAN_POINT('',(-54.,18.5,110.));
#37821=CARTESIAN_POINT('Origin',(-51.,18.5,110.));
#37822=CARTESIAN_POINT('Origin',(-54.,30.5,110.));
#37823=CARTESIAN_POINT('',(-54.,30.5,110.));
#37824=CARTESIAN_POINT('',(-54.,30.5,110.));
#37825=CARTESIAN_POINT('',(-54.,27.5,110.));
#37826=CARTESIAN_POINT('Origin',(-45.,24.5,114.));
#37827=CARTESIAN_POINT('',(-51.9,24.5,114.));
#37828=CARTESIAN_POINT('Origin',(-45.,24.5,114.));
#37829=CARTESIAN_POINT('Origin',(38.,27.5,112.));
#37830=CARTESIAN_POINT('',(38.,30.5,114.));
#37831=CARTESIAN_POINT('',(36.,30.5,112.));
#37832=CARTESIAN_POINT('Origin',(38.,30.5,112.));
#37833=CARTESIAN_POINT('',(36.,18.5,112.));
#37834=CARTESIAN_POINT('',(36.,27.5,112.));
#37835=CARTESIAN_POINT('',(38.,18.5,114.));
#37836=CARTESIAN_POINT('Origin',(38.,18.5,112.));
#37837=CARTESIAN_POINT('',(38.,27.5,114.));
#37838=CARTESIAN_POINT('Ctrl Pts',(36.,18.5,112.));
#37839=CARTESIAN_POINT('Ctrl Pts',(36.,15.5,112.));
#37840=CARTESIAN_POINT('Ctrl Pts',(39.,15.5,112.));
#37841=CARTESIAN_POINT('Ctrl Pts',(36.,18.5,114.));
#37842=CARTESIAN_POINT('Ctrl Pts',(36.,15.5,114.));
#37843=CARTESIAN_POINT('Ctrl Pts',(39.,15.5,114.));
#37844=CARTESIAN_POINT('Ctrl Pts',(38.,18.5,114.));
#37845=CARTESIAN_POINT('Ctrl Pts',(38.,17.5,114.));
#37846=CARTESIAN_POINT('Ctrl Pts',(39.,17.5,114.));
#37847=CARTESIAN_POINT('',(39.,15.5,112.));
#37848=CARTESIAN_POINT('',(39.,17.5,114.));
#37849=CARTESIAN_POINT('Origin',(39.,17.5,112.));
#37850=CARTESIAN_POINT('Origin',(39.,18.5,114.));
#37851=CARTESIAN_POINT('Origin',(39.,18.5,112.));
#37852=CARTESIAN_POINT('Origin',(42.,17.5,112.));
#37853=CARTESIAN_POINT('',(51.,15.5,112.));
#37854=CARTESIAN_POINT('',(51.,17.5,114.));
#37855=CARTESIAN_POINT('Origin',(51.,17.5,112.));
#37856=CARTESIAN_POINT('',(42.,17.5,114.));
#37857=CARTESIAN_POINT('',(42.,15.5,112.));
#37858=CARTESIAN_POINT('Ctrl Pts',(51.,15.5,112.));
#37859=CARTESIAN_POINT('Ctrl Pts',(54.,15.5,112.));
#37860=CARTESIAN_POINT('Ctrl Pts',(54.,18.5,112.));
#37861=CARTESIAN_POINT('Ctrl Pts',(51.,15.5,114.));
#37862=CARTESIAN_POINT('Ctrl Pts',(54.,15.5,114.));
#37863=CARTESIAN_POINT('Ctrl Pts',(54.,18.5,114.));
#37864=CARTESIAN_POINT('Ctrl Pts',(51.,17.5,114.));
#37865=CARTESIAN_POINT('Ctrl Pts',(52.,17.5,114.));
#37866=CARTESIAN_POINT('Ctrl Pts',(52.,18.5,114.));
#37867=CARTESIAN_POINT('',(54.,18.5,112.));
#37868=CARTESIAN_POINT('',(52.,18.5,114.));
#37869=CARTESIAN_POINT('Origin',(52.,18.5,112.));
#37870=CARTESIAN_POINT('Origin',(51.,18.5,114.));
#37871=CARTESIAN_POINT('Origin',(51.,18.5,112.));
#37872=CARTESIAN_POINT('Origin',(52.,21.5,112.));
#37873=CARTESIAN_POINT('',(54.,30.5,112.));
#37874=CARTESIAN_POINT('',(52.,30.5,114.));
#37875=CARTESIAN_POINT('Origin',(52.,30.5,112.));
#37876=CARTESIAN_POINT('',(52.,21.5,114.));
#37877=CARTESIAN_POINT('',(54.,21.5,112.));
#37878=CARTESIAN_POINT('Ctrl Pts',(54.,30.5,112.));
#37879=CARTESIAN_POINT('Ctrl Pts',(54.,33.5,112.));
#37880=CARTESIAN_POINT('Ctrl Pts',(51.,33.5,112.));
#37881=CARTESIAN_POINT('Ctrl Pts',(54.,30.5,114.));
#37882=CARTESIAN_POINT('Ctrl Pts',(54.,33.5,114.));
#37883=CARTESIAN_POINT('Ctrl Pts',(51.,33.5,114.));
#37884=CARTESIAN_POINT('Ctrl Pts',(52.,30.5,114.));
#37885=CARTESIAN_POINT('Ctrl Pts',(52.,31.5,114.));
#37886=CARTESIAN_POINT('Ctrl Pts',(51.,31.5,114.));
#37887=CARTESIAN_POINT('',(51.,33.5,112.));
#37888=CARTESIAN_POINT('',(51.,31.5,114.));
#37889=CARTESIAN_POINT('Origin',(51.,31.5,112.));
#37890=CARTESIAN_POINT('Origin',(51.,30.5,114.));
#37891=CARTESIAN_POINT('Origin',(51.,30.5,112.));
#37892=CARTESIAN_POINT('Origin',(48.,31.5,112.));
#37893=CARTESIAN_POINT('',(39.,33.5,112.));
#37894=CARTESIAN_POINT('',(39.,31.5,114.));
#37895=CARTESIAN_POINT('Origin',(39.,31.5,112.));
#37896=CARTESIAN_POINT('',(48.,31.5,114.));
#37897=CARTESIAN_POINT('',(48.,33.5,112.));
#37898=CARTESIAN_POINT('Ctrl Pts',(39.,33.5,112.));
#37899=CARTESIAN_POINT('Ctrl Pts',(36.,33.5,112.));
#37900=CARTESIAN_POINT('Ctrl Pts',(36.,30.5,112.));
#37901=CARTESIAN_POINT('Ctrl Pts',(39.,33.5,114.));
#37902=CARTESIAN_POINT('Ctrl Pts',(36.,33.5,114.));
#37903=CARTESIAN_POINT('Ctrl Pts',(36.,30.5,114.));
#37904=CARTESIAN_POINT('Ctrl Pts',(39.,31.5,114.));
#37905=CARTESIAN_POINT('Ctrl Pts',(38.,31.5,114.));
#37906=CARTESIAN_POINT('Ctrl Pts',(38.,30.5,114.));
#37907=CARTESIAN_POINT('Origin',(39.,30.5,114.));
#37908=CARTESIAN_POINT('Origin',(39.,30.5,112.));
#37909=CARTESIAN_POINT('Origin',(51.,18.5,110.));
#37910=CARTESIAN_POINT('',(51.,15.5,110.));
#37911=CARTESIAN_POINT('',(51.,15.5,110.));
#37912=CARTESIAN_POINT('',(54.,18.5,110.));
#37913=CARTESIAN_POINT('Origin',(51.,18.5,110.));
#37914=CARTESIAN_POINT('',(54.,18.5,110.));
#37915=CARTESIAN_POINT('Origin',(39.,15.5,110.));
#37916=CARTESIAN_POINT('',(39.,15.5,110.));
#37917=CARTESIAN_POINT('',(39.,15.5,110.));
#37918=CARTESIAN_POINT('',(19.5,15.5,110.));
#37919=CARTESIAN_POINT('Origin',(39.,18.5,110.));
#37920=CARTESIAN_POINT('',(36.,18.5,110.));
#37921=CARTESIAN_POINT('',(36.,18.5,110.));
#37922=CARTESIAN_POINT('Origin',(39.,18.5,110.));
#37923=CARTESIAN_POINT('Origin',(36.,30.5,110.));
#37924=CARTESIAN_POINT('',(36.,30.5,110.));
#37925=CARTESIAN_POINT('',(36.,30.5,110.));
#37926=CARTESIAN_POINT('',(36.,27.5,110.));
#37927=CARTESIAN_POINT('Origin',(45.,24.5,114.));
#37928=CARTESIAN_POINT('',(38.1,24.5,114.));
#37929=CARTESIAN_POINT('Origin',(45.,24.5,114.));
#37930=CARTESIAN_POINT('Origin',(0.,2.,0.));
#37931=CARTESIAN_POINT('',(-8.59702053001442E-15,2.,-70.2));
#37932=CARTESIAN_POINT('Origin',(-8.84194988984389E-15,2.,-72.2));
#37933=CARTESIAN_POINT('Origin',(0.,2.,0.));
#37934=CARTESIAN_POINT('Origin',(0.,2.45,0.));
#37935=CARTESIAN_POINT('',(-8.59702053001442E-15,9.,-70.2));
#37936=CARTESIAN_POINT('',(-8.59702053001442E-15,2.45,-70.2));
#37937=CARTESIAN_POINT('',(-35.1,9.,60.7949833456676));
#37938=CARTESIAN_POINT('Origin',(1.55431223447522E-14,9.,2.22044604925031E-15));
#37939=CARTESIAN_POINT('',(-35.1,7.,60.7949833456676));
#37940=CARTESIAN_POINT('',(-35.1,5.,60.7949833456676));
#37941=CARTESIAN_POINT('',(-33.353701286408,5.,61.770305248534));
#37942=CARTESIAN_POINT('Ctrl Pts',(-35.1,7.,60.7949833456676));
#37943=CARTESIAN_POINT('Ctrl Pts',(-35.1,6.74887417302153,60.7949833456676));
#37944=CARTESIAN_POINT('Ctrl Pts',(-35.0565641212333,6.48100990452462,60.8201260037975));
#37945=CARTESIAN_POINT('Ctrl Pts',(-34.8795797765736,5.98825083345615,60.9217968358934));
#37946=CARTESIAN_POINT('Ctrl Pts',(-34.7459927648389,5.76335612152486,60.9982583355795));
#37947=CARTESIAN_POINT('Ctrl Pts',(-34.4369258181726,5.40818751436047,61.1732758953421));
#37948=CARTESIAN_POINT('Ctrl Pts',(-34.2408331115211,5.25425928439315,61.2834894043871));
#37949=CARTESIAN_POINT('Ctrl Pts',(-33.8097426473724,5.05016619199587,61.5223701418215));
#37950=CARTESIAN_POINT('Ctrl Pts',(-33.574708028271,5.,61.6509697066304));
#37951=CARTESIAN_POINT('Ctrl Pts',(-33.353701286408,5.,61.770305248534));
#37952=CARTESIAN_POINT('',(33.3537012864079,5.,61.770305248534));
#37953=CARTESIAN_POINT('Origin',(0.,5.,0.));
#37954=CARTESIAN_POINT('',(35.1,7.,60.7949833456676));
#37955=CARTESIAN_POINT('Ctrl Pts',(33.353701286408,5.,61.770305248534));
#37956=CARTESIAN_POINT('Ctrl Pts',(33.574708028271,5.,61.6509697066305));
#37957=CARTESIAN_POINT('Ctrl Pts',(33.8097426473723,5.05016619199587,61.5223701418215));
#37958=CARTESIAN_POINT('Ctrl Pts',(34.2408331115211,5.25425928439315,61.2834894043871));
#37959=CARTESIAN_POINT('Ctrl Pts',(34.4369258181726,5.40818751436047,61.1732758953421));
#37960=CARTESIAN_POINT('Ctrl Pts',(34.7459927648389,5.76335612152486,60.9982583355795));
#37961=CARTESIAN_POINT('Ctrl Pts',(34.8795797765736,5.98825083345615,60.9217968358934));
#37962=CARTESIAN_POINT('Ctrl Pts',(35.0565641212333,6.48100990452463,60.8201260037975));
#37963=CARTESIAN_POINT('Ctrl Pts',(35.1,6.74887417302153,60.7949833456676));
#37964=CARTESIAN_POINT('Ctrl Pts',(35.1,7.,60.7949833456676));
#37965=CARTESIAN_POINT('',(35.1,9.,60.7949833456676));
#37966=CARTESIAN_POINT('',(35.1,5.,60.7949833456676));
#37967=CARTESIAN_POINT('Origin',(1.55431223447522E-14,9.,2.22044604925031E-15));
#37968=CARTESIAN_POINT('Origin',(0.,7.,0.));
#37969=CARTESIAN_POINT('',(-2.70034619211991E-15,5.,-22.05));
#37970=CARTESIAN_POINT('Origin',(0.,5.,0.));
#37971=CARTESIAN_POINT('',(-2.45541683229044E-15,7.,-20.05));
#37972=CARTESIAN_POINT('Origin',(-2.70034619211991E-15,7.,-22.05));
#37973=CARTESIAN_POINT('Origin',(0.,7.,0.));
#37974=CARTESIAN_POINT('Origin',(0.,5.,20.05));
#37975=CARTESIAN_POINT('',(25.7497613597537,5.,48.5998949578673));
#37976=CARTESIAN_POINT('',(16.8589015289006,5.,33.2004740078565));
#37977=CARTESIAN_POINT('',(-25.7497613597537,5.,48.5998949578673));
#37978=CARTESIAN_POINT('',(-20.1589015289006,5.,38.9162416728338));
#37979=CARTESIAN_POINT('Origin',(-2.22044604925031E-15,5.,-1.11022302462516E-15));
#37980=CARTESIAN_POINT('Origin',(0.,17.5,0.));
#37981=CARTESIAN_POINT('',(-2.45541683229044E-15,30.,-20.05));
#37982=CARTESIAN_POINT('',(-2.45541683229044E-15,17.5,-20.05));
#37983=CARTESIAN_POINT('Origin',(0.,30.,0.));
#37984=CARTESIAN_POINT('Origin',(16.8589015289006,7.,33.2004740078565));
#37985=CARTESIAN_POINT('',(28.5,7.,49.363448015713));
#37986=CARTESIAN_POINT('',(18.5909523364695,7.,32.2004740078565));
#37987=CARTESIAN_POINT('Ctrl Pts',(25.7497613597537,5.,48.5998949578673));
#37988=CARTESIAN_POINT('Ctrl Pts',(25.7526780842804,5.,48.6007336279338));
#37989=CARTESIAN_POINT('Ctrl Pts',(25.7555948357263,5.00000332839376,48.6015722116644));
#37990=CARTESIAN_POINT('Ctrl Pts',(26.0511801116044,5.00067799125553,48.6865452392508));
#37991=CARTESIAN_POINT('Ctrl Pts',(26.3460171339481,5.03486692594129,48.7703312615877));
#37992=CARTESIAN_POINT('Ctrl Pts',(26.9009050741236,5.17036553160275,48.9263173337706));
#37993=CARTESIAN_POINT('Ctrl Pts',(27.1656717084766,5.26888612938734,48.9999335178016));
#37994=CARTESIAN_POINT('Ctrl Pts',(27.6543280663132,5.53732121577603,49.1345826791917));
#37995=CARTESIAN_POINT('Ctrl Pts',(27.8815247792677,5.70887974191627,49.1965246803542));
#37996=CARTESIAN_POINT('Ctrl Pts',(28.2058967874217,6.07814435711566,49.2844121204924));
#37997=CARTESIAN_POINT('Ctrl Pts',(28.3204632986599,6.25786799621181,49.3152504654719));
#37998=CARTESIAN_POINT('Ctrl Pts',(28.464178087957,6.63005485401211,49.3538606820259));
#37999=CARTESIAN_POINT('Ctrl Pts',(28.5,6.812926309153,49.363448015713));
#38000=CARTESIAN_POINT('Ctrl Pts',(28.5,7.,49.363448015713));
#38001=CARTESIAN_POINT('Origin',(-2.22044604925031E-15,7.,-1.11022302462516E-15));
#38002=CARTESIAN_POINT('',(-28.5,7.,49.363448015713));
#38003=CARTESIAN_POINT('Origin',(-2.22044604925031E-15,7.,-1.11022302462516E-15));
#38004=CARTESIAN_POINT('Ctrl Pts',(-25.7497613597537,5.,48.5998949578673));
#38005=CARTESIAN_POINT('Ctrl Pts',(-25.7526780842808,5.,48.6007336279339));
#38006=CARTESIAN_POINT('Ctrl Pts',(-25.7555948357259,5.00000332839376,48.6015722116643));
#38007=CARTESIAN_POINT('Ctrl Pts',(-26.0511801116162,5.00067799125556,48.6865452392533));
#38008=CARTESIAN_POINT('Ctrl Pts',(-26.34601713395,5.03486692594175,48.7703312615882));
#38009=CARTESIAN_POINT('Ctrl Pts',(-26.9009050741237,5.17036553160276,48.9263173337706));
#38010=CARTESIAN_POINT('Ctrl Pts',(-27.1656717084766,5.26888612938735,48.9999335178016));
#38011=CARTESIAN_POINT('Ctrl Pts',(-27.6543280663132,5.53732121577604,49.1345826791917));
#38012=CARTESIAN_POINT('Ctrl Pts',(-27.8815247792676,5.70887974191628,49.1965246803542));
#38013=CARTESIAN_POINT('Ctrl Pts',(-28.2058967874216,6.07814435711566,49.2844121204924));
#38014=CARTESIAN_POINT('Ctrl Pts',(-28.3204632986599,6.25786799621181,49.3152504654719));
#38015=CARTESIAN_POINT('Ctrl Pts',(-28.4641780879569,6.63005485401195,49.3538606820259));
#38016=CARTESIAN_POINT('Ctrl Pts',(-28.5,6.81292630915292,49.363448015713));
#38017=CARTESIAN_POINT('Ctrl Pts',(-28.5,7.,49.363448015713));
#38018=CARTESIAN_POINT('Origin',(-20.1589015289006,7.,38.9162416728338));
#38019=CARTESIAN_POINT('',(-21.8909523364695,7.,37.9162416728338));
#38020=CARTESIAN_POINT('Origin',(28.5,5.,49.363448015713));
#38021=CARTESIAN_POINT('',(28.5,9.,49.363448015713));
#38022=CARTESIAN_POINT('',(28.5,5.,49.363448015713));
#38023=CARTESIAN_POINT('',(35.1,9.,60.7949833456676));
#38024=CARTESIAN_POINT('Origin',(-2.22044604925031E-15,5.,-1.11022302462516E-15));
#38025=CARTESIAN_POINT('',(-28.5,9.,49.363448015713));
#38026=CARTESIAN_POINT('',(-28.5,5.,49.363448015713));
#38027=CARTESIAN_POINT('Origin',(-2.22044604925031E-15,9.,-1.11022302462516E-15));
#38028=CARTESIAN_POINT('Origin',(-35.1,5.,60.7949833456676));
#38029=CARTESIAN_POINT('',(-35.1,9.,60.7949833456676));
#38030=CARTESIAN_POINT('Origin',(90.,24.5,80.));
#38031=CARTESIAN_POINT('',(92.,8.,88.9057565652784));
#38032=CARTESIAN_POINT('',(90.,9.76000000000001,87.9558091983154));
#38033=CARTESIAN_POINT('Origin',(90.,8.,88.9057565652784));
#38034=CARTESIAN_POINT('',(90.0000000000017,24.5,96.75));
#38035=CARTESIAN_POINT('Origin',(90.,24.5,80.));
#38036=CARTESIAN_POINT('',(90.,39.24,87.9558091983154));
#38037=CARTESIAN_POINT('Origin',(90.,24.5,80.));
#38038=CARTESIAN_POINT('',(92.,41.,88.9057565652784));
#38039=CARTESIAN_POINT('Origin',(90.,41.,88.9057565652784));
#38040=CARTESIAN_POINT('Origin',(92.,24.5,80.));
#38041=CARTESIAN_POINT('Ctrl Pts',(90.,39.24,87.9558091983154));
#38042=CARTESIAN_POINT('Ctrl Pts',(90.,39.9925784091656,86.5614814216451));
#38043=CARTESIAN_POINT('Ctrl Pts',(89.6247663405678,40.8156274544267,84.3254689358931));
#38044=CARTESIAN_POINT('Ctrl Pts',(89.2998530158654,41.2636159206073,81.1945680459964));
#38045=CARTESIAN_POINT('Ctrl Pts',(89.2947826313174,41.2634913601257,78.0106147164496));
#38046=CARTESIAN_POINT('Ctrl Pts',(89.7999750759969,40.5929907863474,74.9075303285633));
#38047=CARTESIAN_POINT('Ctrl Pts',(90.0000000000018,39.6162892045687,72.7413546899905));
#38048=CARTESIAN_POINT('Ctrl Pts',(90.,39.2399999999846,72.0441908016561));
#38049=CARTESIAN_POINT('Ctrl Pts',(90.2991993003419,39.24,87.9558091983154));
#38050=CARTESIAN_POINT('Ctrl Pts',(90.3346190349092,40.0066898073963,86.535095061671));
#38051=CARTESIAN_POINT('Ctrl Pts',(90.0027743158155,40.8288120390463,84.2710725121084));
#38052=CARTESIAN_POINT('Ctrl Pts',(89.7146057062673,41.2627924802528,81.1713647613915));
#38053=CARTESIAN_POINT('Ctrl Pts',(89.7085874510504,41.2631573502512,78.0501047601331));
#38054=CARTESIAN_POINT('Ctrl Pts',(90.1626027926756,40.6115887482596,74.958234183941));
#38055=CARTESIAN_POINT('Ctrl Pts',(90.3169091676267,39.6233449036839,72.754547869977));
#38056=CARTESIAN_POINT('Ctrl Pts',(90.2991993003412,39.2399999999843,72.0441908016555));
#38057=CARTESIAN_POINT('Ctrl Pts',(90.8959652150226,39.3605997833875,88.0209020657502));
#38058=CARTESIAN_POINT('Ctrl Pts',(91.0015487583438,40.1907311515419,86.5517823378691));
#38059=CARTESIAN_POINT('Ctrl Pts',(90.7545425049392,41.0725721868577,84.2251614932142));
#38060=CARTESIAN_POINT('Ctrl Pts',(90.53851955239,41.5271753896422,81.1450147849467));
#38061=CARTESIAN_POINT('Ctrl Pts',(90.5305887720896,41.5281747157396,78.0951094062104));
#38062=CARTESIAN_POINT('Ctrl Pts',(90.8842946702604,40.8429080328149,74.9903449798908));
#38063=CARTESIAN_POINT('Ctrl Pts',(90.9487569866831,39.7756654674493,72.7136577981596));
#38064=CARTESIAN_POINT('Ctrl Pts',(90.8959652150205,39.3605997833705,71.9790979342197));
#38065=CARTESIAN_POINT('Ctrl Pts',(91.7377033118041,39.9492389941977,88.3386158546141));
#38066=CARTESIAN_POINT('Ctrl Pts',(91.8947737455775,40.9811300899403,86.8108756400174));
#38067=CARTESIAN_POINT('Ctrl Pts',(91.6657296933035,42.1250155322977,84.3862284321629));
#38068=CARTESIAN_POINT('Ctrl Pts',(91.4529882670294,42.7487257343339,81.1860321244351));
#38069=CARTESIAN_POINT('Ctrl Pts',(91.4440144391454,42.74912106062,78.0267860385529));
#38070=CARTESIAN_POINT('Ctrl Pts',(91.796936898285,41.8127986994321,74.7955406094651));
#38071=CARTESIAN_POINT('Ctrl Pts',(91.8162385286899,40.4651845420497,72.4252542526523));
#38072=CARTESIAN_POINT('Ctrl Pts',(91.7377033118009,39.9492389941766,71.6613841453547));
#38073=CARTESIAN_POINT('Ctrl Pts',(92.,40.6050569235487,88.6925888746107));
#38074=CARTESIAN_POINT('Ctrl Pts',(92.0842395543339,41.8020668522328,87.1438713820414));
#38075=CARTESIAN_POINT('Ctrl Pts',(91.675367371483,43.1416553165464,84.6695040349086));
#38076=CARTESIAN_POINT('Ctrl Pts',(91.304905483517,43.8870217698157,81.2798053980333));
#38077=CARTESIAN_POINT('Ctrl Pts',(91.2970139150286,43.8867145802671,77.8695340412403));
#38078=CARTESIAN_POINT('Ctrl Pts',(91.881114233009,42.7711777978807,74.486873307736));
#38079=CARTESIAN_POINT('Ctrl Pts',(92.0421197771678,41.2035618878683,72.0817698716415));
#38080=CARTESIAN_POINT('Ctrl Pts',(91.9999999999983,40.6050569235242,71.3074111253576));
#38081=CARTESIAN_POINT('Ctrl Pts',(92.,41.,88.9057565652784));
#38082=CARTESIAN_POINT('Ctrl Pts',(92.,42.2636577765839,87.3449418899014));
#38083=CARTESIAN_POINT('Ctrl Pts',(91.4371495108518,43.6456431137762,84.8419428386863));
#38084=CARTESIAN_POINT('Ctrl Pts',(90.9497795237981,44.3978625532585,81.3372030365632));
#38085=CARTESIAN_POINT('Ctrl Pts',(90.9421739469762,44.397653403196,77.7730761751302));
#38086=CARTESIAN_POINT('Ctrl Pts',(91.6999626139954,43.2718128875236,74.2994742483918));
#38087=CARTESIAN_POINT('Ctrl Pts',(92.0000000000027,41.6318288882683,71.8746507723773));
#38088=CARTESIAN_POINT('Ctrl Pts',(92.,40.9999999999741,71.0942434346896));
#38089=CARTESIAN_POINT('',(90.,39.2399999999846,72.0441908016561));
#38090=CARTESIAN_POINT('',(92.,40.9999999999871,71.0942434346896));
#38091=CARTESIAN_POINT('Origin',(90.,40.9999999999828,71.0942434346896));
#38092=CARTESIAN_POINT('Ctrl Pts',(92.,40.9999999999741,71.0942434346896));
#38093=CARTESIAN_POINT('Ctrl Pts',(92.0000000000027,41.6318288882683,71.8746507723773));
#38094=CARTESIAN_POINT('Ctrl Pts',(91.6999626139954,43.2718128875236,74.2994742483918));
#38095=CARTESIAN_POINT('Ctrl Pts',(90.9421739469762,44.397653403196,77.7730761751302));
#38096=CARTESIAN_POINT('Ctrl Pts',(90.9497795237981,44.3978625532585,81.3372030365632));
#38097=CARTESIAN_POINT('Ctrl Pts',(91.4371495108518,43.6456431137762,84.8419428386863));
#38098=CARTESIAN_POINT('Ctrl Pts',(92.,42.2636577765839,87.3449418899014));
#38099=CARTESIAN_POINT('Ctrl Pts',(92.,41.,88.9057565652784));
#38100=CARTESIAN_POINT('Ctrl Pts',(90.,39.24,87.9558091983154));
#38101=CARTESIAN_POINT('Ctrl Pts',(90.,39.9925784091656,86.5614814216451));
#38102=CARTESIAN_POINT('Ctrl Pts',(89.6247663405678,40.8156274544267,84.3254689358931));
#38103=CARTESIAN_POINT('Ctrl Pts',(89.2998530158654,41.2636159206073,81.1945680459964));
#38104=CARTESIAN_POINT('Ctrl Pts',(89.2947826313174,41.2634913601257,78.0106147164496));
#38105=CARTESIAN_POINT('Ctrl Pts',(89.7999750759969,40.5929907863474,74.9075303285633));
#38106=CARTESIAN_POINT('Ctrl Pts',(90.0000000000018,39.6162892045687,72.7413546899905));
#38107=CARTESIAN_POINT('Ctrl Pts',(90.,39.2399999999846,72.0441908016561));
#38108=CARTESIAN_POINT('Origin',(90.,24.5,80.));
#38109=CARTESIAN_POINT('',(90.,9.76,72.0441908016846));
#38110=CARTESIAN_POINT('',(92.,8.,71.0942434347216));
#38111=CARTESIAN_POINT('Origin',(90.,8.,71.0942434347216));
#38112=CARTESIAN_POINT('Origin',(92.,24.5,80.));
#38113=CARTESIAN_POINT('Origin',(90.,24.5,80.));
#38114=CARTESIAN_POINT('Ctrl Pts',(90.,9.75999999999999,72.0441908016846));
#38115=CARTESIAN_POINT('Ctrl Pts',(90.,9.0074215908359,73.4385185783522));
#38116=CARTESIAN_POINT('Ctrl Pts',(89.6266311441226,8.1845886271713,75.6741761987655));
#38117=CARTESIAN_POINT('Ctrl Pts',(89.2991132263711,7.73666063782126,78.8058465499708));
#38118=CARTESIAN_POINT('Ctrl Pts',(89.3000459409121,7.73672873935593,81.19334048201));
#38119=CARTESIAN_POINT('Ctrl Pts',(89.6267478600051,8.18449985726607,84.325124610408));
#38120=CARTESIAN_POINT('Ctrl Pts',(90.,9.00742159083591,86.5614814216478));
#38121=CARTESIAN_POINT('Ctrl Pts',(90.,9.76,87.9558091983154));
#38122=CARTESIAN_POINT('Ctrl Pts',(90.2991993003419,9.75999999999999,72.0441908016846));
#38123=CARTESIAN_POINT('Ctrl Pts',(90.3346190349092,8.99331019260512,73.4649049383263));
#38124=CARTESIAN_POINT('Ctrl Pts',(90.0050584632404,8.1716440685805,75.728826404617));
#38125=CARTESIAN_POINT('Ctrl Pts',(89.7138584041868,7.7375255864327,78.8287976868203));
#38126=CARTESIAN_POINT('Ctrl Pts',(89.7146849504547,7.73748906209263,81.1706049698146));
#38127=CARTESIAN_POINT('Ctrl Pts',(90.0052338960302,8.17159823794263,84.2702498335073));
#38128=CARTESIAN_POINT('Ctrl Pts',(90.3346190349092,8.99331019260513,86.5350950616738));
#38129=CARTESIAN_POINT('Ctrl Pts',(90.2991993003419,9.76,87.9558091983154));
#38130=CARTESIAN_POINT('Ctrl Pts',(90.895972204776,9.639403332612,71.9790996160882));
#38131=CARTESIAN_POINT('Ctrl Pts',(91.001555748097,8.80927196445914,73.4482193439664));
#38132=CARTESIAN_POINT('Ctrl Pts',(90.7577009802419,7.92816993286539,75.7750896491985));
#38133=CARTESIAN_POINT('Ctrl Pts',(90.5378845432001,7.47299912767311,78.8547095061753));
#38134=CARTESIAN_POINT('Ctrl Pts',(90.5384579232711,7.47292007731554,81.1450808709336));
#38135=CARTESIAN_POINT('Ctrl Pts',(90.7580323548137,7.92805069968786,84.2236005862538));
#38136=CARTESIAN_POINT('Ctrl Pts',(91.001555748097,8.80927196445915,86.5517806560335));
#38137=CARTESIAN_POINT('Ctrl Pts',(90.895972204776,9.639403332612,88.0209003839118));
#38138=CARTESIAN_POINT('Ctrl Pts',(91.7377173103273,9.05076546339944,71.661386551342));
#38139=CARTESIAN_POINT('Ctrl Pts',(91.8947877441005,8.01887436765872,73.189126765936));
#38140=CARTESIAN_POINT('Ctrl Pts',(91.6692926181241,6.87547810564428,75.614027382202));
#38141=CARTESIAN_POINT('Ctrl Pts',(91.4520070536192,6.25140468377173,78.8135720334519));
#38142=CARTESIAN_POINT('Ctrl Pts',(91.452718603279,6.25149630787978,81.1863103961658));
#38143=CARTESIAN_POINT('Ctrl Pts',(91.6695544894331,6.87512702275017,84.3845380263156));
#38144=CARTESIAN_POINT('Ctrl Pts',(91.8947877441005,8.01887436765873,86.810873234064));
#38145=CARTESIAN_POINT('Ctrl Pts',(91.7377173103273,9.05076546339944,88.338613448658));
#38146=CARTESIAN_POINT('Ctrl Pts',(92.,8.39494307645129,71.3074111253893));
#38147=CARTESIAN_POINT('Ctrl Pts',(92.0842395543337,7.19793314776939,72.8561286179559));
#38148=CARTESIAN_POINT('Ctrl Pts',(91.678416051393,5.8585488221207,75.3303789281826));
#38149=CARTESIAN_POINT('Ctrl Pts',(91.304319836793,5.11301911897351,78.7203674934503));
#38150=CARTESIAN_POINT('Ctrl Pts',(91.3052869701975,5.11331092315558,81.2790379801232));
#38151=CARTESIAN_POINT('Ctrl Pts',(91.6787682642829,5.85813477479916,84.6685518615818));
#38152=CARTESIAN_POINT('Ctrl Pts',(92.0842395543337,7.1979331477694,87.1438713820441));
#38153=CARTESIAN_POINT('Ctrl Pts',(92.,8.39494307645129,88.6925888746107));
#38154=CARTESIAN_POINT('Ctrl Pts',(92.,8.00000000000001,71.0942434347216));
#38155=CARTESIAN_POINT('Ctrl Pts',(92.,6.73634222341846,72.6550581100958));
#38156=CARTESIAN_POINT('Ctrl Pts',(91.4399467161839,5.35471970980254,75.1576599239912));
#38157=CARTESIAN_POINT('Ctrl Pts',(90.9486698395567,4.60260181723717,78.6632610634002));
#38158=CARTESIAN_POINT('Ctrl Pts',(90.9500689113682,4.60271616682896,81.3358288977724));
#38159=CARTESIAN_POINT('Ctrl Pts',(91.4401217900076,5.35457065585718,84.8415573997105));
#38160=CARTESIAN_POINT('Ctrl Pts',(92.,6.73634222341846,87.3449418899042));
#38161=CARTESIAN_POINT('Ctrl Pts',(92.,8.00000000000001,88.9057565652784));
#38162=CARTESIAN_POINT('Ctrl Pts',(92.,8.00000000000001,88.9057565652784));
#38163=CARTESIAN_POINT('Ctrl Pts',(92.,6.73634222341846,87.3449418899042));
#38164=CARTESIAN_POINT('Ctrl Pts',(91.4401217900076,5.35457065585718,84.8415573997105));
#38165=CARTESIAN_POINT('Ctrl Pts',(90.9500689113682,4.60271616682896,81.3358288977724));
#38166=CARTESIAN_POINT('Ctrl Pts',(90.9486698395567,4.60260181723717,78.6632610634002));
#38167=CARTESIAN_POINT('Ctrl Pts',(91.4399467161839,5.35471970980254,75.1576599239912));
#38168=CARTESIAN_POINT('Ctrl Pts',(92.,6.73634222341846,72.6550581100958));
#38169=CARTESIAN_POINT('Ctrl Pts',(92.,8.00000000000001,71.0942434347216));
#38170=CARTESIAN_POINT('Ctrl Pts',(90.,9.75999999999999,72.0441908016846));
#38171=CARTESIAN_POINT('Ctrl Pts',(90.,9.0074215908359,73.4385185783522));
#38172=CARTESIAN_POINT('Ctrl Pts',(89.6266311441226,8.1845886271713,75.6741761987655));
#38173=CARTESIAN_POINT('Ctrl Pts',(89.2991132263711,7.73666063782126,78.8058465499708));
#38174=CARTESIAN_POINT('Ctrl Pts',(89.3000459409121,7.73672873935593,81.19334048201));
#38175=CARTESIAN_POINT('Ctrl Pts',(89.6267478600051,8.18449985726607,84.325124610408));
#38176=CARTESIAN_POINT('Ctrl Pts',(90.,9.00742159083591,86.5614814216478));
#38177=CARTESIAN_POINT('Ctrl Pts',(90.,9.76,87.9558091983154));
#38178=CARTESIAN_POINT('Origin',(86.,7.99999999999997,50.));
#38179=CARTESIAN_POINT('',(92.,8.,108.));
#38180=CARTESIAN_POINT('',(92.,8.,50.));
#38181=CARTESIAN_POINT('',(86.,2.,108.));
#38182=CARTESIAN_POINT('Origin',(86.,7.99999999999997,108.));
#38183=CARTESIAN_POINT('',(86.,2.,50.));
#38184=CARTESIAN_POINT('',(86.,2.,50.));
#38185=CARTESIAN_POINT('',(92.,8.,50.));
#38186=CARTESIAN_POINT('Origin',(86.,7.99999999999997,50.));
#38187=CARTESIAN_POINT('',(92.,8.,50.));
#38188=CARTESIAN_POINT('Origin',(92.,8.,50.));
#38189=CARTESIAN_POINT('',(92.,41.,108.));
#38190=CARTESIAN_POINT('',(92.,41.,50.));
#38191=CARTESIAN_POINT('',(92.,16.25,108.));
#38192=CARTESIAN_POINT('Origin',(92.,24.5,80.));
#38193=CARTESIAN_POINT('',(70.,24.5,96.75));
#38194=CARTESIAN_POINT('',(92.,24.5,96.75));
#38195=CARTESIAN_POINT('Origin',(70.,24.5,80.));
#38196=CARTESIAN_POINT('Origin',(43.,45.,52.));
#38197=CARTESIAN_POINT('',(-86.,45.,50.));
#38198=CARTESIAN_POINT('',(43.,45.,50.));
#38199=CARTESIAN_POINT('',(-86.,47.,52.));
#38200=CARTESIAN_POINT('Origin',(-86.,45.,52.));
#38201=CARTESIAN_POINT('',(43.,47.,52.));
#38202=CARTESIAN_POINT('Origin',(-90.,32.75,52.));
#38203=CARTESIAN_POINT('',(-92.,41.,52.));
#38204=CARTESIAN_POINT('',(-90.,41.,50.));
#38205=CARTESIAN_POINT('Origin',(-90.,41.,52.));
#38206=CARTESIAN_POINT('',(-90.,8.,50.));
#38207=CARTESIAN_POINT('',(-90.,32.75,50.));
#38208=CARTESIAN_POINT('',(-92.,8.,52.));
#38209=CARTESIAN_POINT('Origin',(-90.,8.,52.));
#38210=CARTESIAN_POINT('',(-92.,32.75,52.));
#38211=CARTESIAN_POINT('Origin',(-86.,7.99999999999997,52.));
#38212=CARTESIAN_POINT('',(-86.,4.00000000000001,50.));
#38213=CARTESIAN_POINT('',(-86.,2.00000000000001,52.));
#38214=CARTESIAN_POINT('Origin',(-86.,4.00000000000001,52.));
#38215=CARTESIAN_POINT('Origin',(-86.,7.99999999999997,52.));
#38216=CARTESIAN_POINT('Origin',(-86.,7.99999999999997,50.));
#38217=CARTESIAN_POINT('Origin',(-43.,4.,52.));
#38218=CARTESIAN_POINT('',(-43.,2.,52.));
#38219=CARTESIAN_POINT('',(-43.,4.,50.));
#38220=CARTESIAN_POINT('Origin',(-86.,41.,52.));
#38221=CARTESIAN_POINT('Origin',(-86.,41.,52.));
#38222=CARTESIAN_POINT('Origin',(-86.,41.,50.));
#38223=CARTESIAN_POINT('Origin',(-86.,7.99999999999997,50.));
#38224=CARTESIAN_POINT('',(-86.,2.00000000000001,108.));
#38225=CARTESIAN_POINT('',(-86.,2.00000000000001,50.));
#38226=CARTESIAN_POINT('',(-92.,8.,108.));
#38227=CARTESIAN_POINT('Origin',(-86.,7.99999999999997,108.));
#38228=CARTESIAN_POINT('',(-92.,8.,88.9057565652784));
#38229=CARTESIAN_POINT('',(-92.,8.,50.));
#38230=CARTESIAN_POINT('',(-92.,8.00000000001294,71.0942434346896));
#38231=CARTESIAN_POINT('Ctrl Pts',(-92.,8.00000000002587,71.0942434346896));
#38232=CARTESIAN_POINT('Ctrl Pts',(-92.0000000000041,7.05225666758454,72.2648544412212));
#38233=CARTESIAN_POINT('Ctrl Pts',(-91.713227279185,6.04343085354599,73.9095997432177));
#38234=CARTESIAN_POINT('Ctrl Pts',(-91.255731456336,5.07242771945905,76.4722824902359));
#38235=CARTESIAN_POINT('Ctrl Pts',(-90.947934136765,4.60143957017688,78.6641302175159));
#38236=CARTESIAN_POINT('Ctrl Pts',(-90.942940568041,4.6025640632853,82.2271784882658));
#38237=CARTESIAN_POINT('Ctrl Pts',(-91.6991668412039,5.72806963647306,85.7013212348271));
#38238=CARTESIAN_POINT('Ctrl Pts',(-92.,7.36817111170808,88.1253492275899));
#38239=CARTESIAN_POINT('Ctrl Pts',(-92.,8.00000000000001,88.9057565652784));
#38240=CARTESIAN_POINT('',(-92.,8.,50.));
#38241=CARTESIAN_POINT('Origin',(-86.,2.,50.));
#38242=CARTESIAN_POINT('',(-86.,2.,50.));
#38243=CARTESIAN_POINT('',(-43.,2.,108.));
#38244=CARTESIAN_POINT('Origin',(0.,24.5,50.));
#38245=CARTESIAN_POINT('Origin',(-90.,32.75,108.));
#38246=CARTESIAN_POINT('',(-90.,41.,110.));
#38247=CARTESIAN_POINT('',(-92.,41.,108.));
#38248=CARTESIAN_POINT('Origin',(-90.,41.,108.));
#38249=CARTESIAN_POINT('',(-92.,32.75,108.));
#38250=CARTESIAN_POINT('',(-90.,8.,110.));
#38251=CARTESIAN_POINT('Origin',(-90.,8.,108.));
#38252=CARTESIAN_POINT('',(-90.,32.75,110.));
#38253=CARTESIAN_POINT('Origin',(-86.,7.99999999999997,108.));
#38254=CARTESIAN_POINT('',(-86.,4.00000000000001,110.));
#38255=CARTESIAN_POINT('Origin',(-86.,4.00000000000001,108.));
#38256=CARTESIAN_POINT('Origin',(-86.,7.99999999999997,110.));
#38257=CARTESIAN_POINT('Origin',(-43.,4.,108.));
#38258=CARTESIAN_POINT('',(86.,4.,110.));
#38259=CARTESIAN_POINT('Origin',(86.,4.,108.));
#38260=CARTESIAN_POINT('',(-43.,4.,110.));
#38261=CARTESIAN_POINT('Origin',(86.,7.99999999999997,108.));
#38262=CARTESIAN_POINT('',(90.,7.99999999999999,110.));
#38263=CARTESIAN_POINT('Origin',(90.,7.99999999999999,108.));
#38264=CARTESIAN_POINT('Origin',(86.,7.99999999999997,110.));
#38265=CARTESIAN_POINT('Origin',(90.,16.25,108.));
#38266=CARTESIAN_POINT('',(90.,41.,110.));
#38267=CARTESIAN_POINT('Origin',(90.,41.,108.));
#38268=CARTESIAN_POINT('',(90.,16.25,110.));
#38269=CARTESIAN_POINT('Origin',(86.,41.,108.));
#38270=CARTESIAN_POINT('',(86.,47.,108.));
#38271=CARTESIAN_POINT('',(86.,45.,110.));
#38272=CARTESIAN_POINT('Origin',(86.,45.,108.));
#38273=CARTESIAN_POINT('Origin',(86.,41.,110.));
#38274=CARTESIAN_POINT('Origin',(86.,41.,108.));
#38275=CARTESIAN_POINT('Origin',(43.,45.,108.));
#38276=CARTESIAN_POINT('',(-86.,47.,108.));
#38277=CARTESIAN_POINT('',(-86.,45.,110.));
#38278=CARTESIAN_POINT('Origin',(-86.,45.,108.));
#38279=CARTESIAN_POINT('',(43.,45.,110.));
#38280=CARTESIAN_POINT('',(43.,47.,108.));
#38281=CARTESIAN_POINT('Origin',(-86.,41.,108.));
#38282=CARTESIAN_POINT('Origin',(-86.,41.,110.));
#38283=CARTESIAN_POINT('Origin',(-86.,41.,108.));
#38284=CARTESIAN_POINT('Origin',(-92.,41.,50.));
#38285=CARTESIAN_POINT('',(-92.,41.,88.9057565652784));
#38286=CARTESIAN_POINT('',(-92.,41.,50.));
#38287=CARTESIAN_POINT('Origin',(-92.,24.5,80.));
#38288=CARTESIAN_POINT('Origin',(0.,24.5,110.));
#38289=CARTESIAN_POINT('',(-51.,33.5,110.));
#38290=CARTESIAN_POINT('Origin',(-51.,30.5,110.));
#38291=CARTESIAN_POINT('',(-39.,33.5,110.));
#38292=CARTESIAN_POINT('',(-19.5,33.5,110.));
#38293=CARTESIAN_POINT('',(-36.,30.5,110.));
#38294=CARTESIAN_POINT('Origin',(-39.,30.5,110.));
#38295=CARTESIAN_POINT('',(-36.,21.5,110.));
#38296=CARTESIAN_POINT('',(39.,33.5,110.));
#38297=CARTESIAN_POINT('Origin',(39.,30.5,110.));
#38298=CARTESIAN_POINT('',(51.,33.5,110.));
#38299=CARTESIAN_POINT('',(25.5,33.5,110.));
#38300=CARTESIAN_POINT('',(54.,30.5,110.));
#38301=CARTESIAN_POINT('Origin',(51.,30.5,110.));
#38302=CARTESIAN_POINT('',(54.,21.5,110.));
#38303=CARTESIAN_POINT('',(-16.75,24.5,110.));
#38304=CARTESIAN_POINT('Origin',(0.,24.5,110.));
#38305=CARTESIAN_POINT('Origin',(-90.,24.5,80.));
#38306=CARTESIAN_POINT('',(-90.,39.24,87.9558091983154));
#38307=CARTESIAN_POINT('Origin',(-90.,41.,88.9057565652784));
#38308=CARTESIAN_POINT('',(-90.0000000000017,24.5,96.75));
#38309=CARTESIAN_POINT('Origin',(-90.,24.5,80.));
#38310=CARTESIAN_POINT('',(-90.,9.76000000000001,87.9558091983154));
#38311=CARTESIAN_POINT('Origin',(-90.,24.5,80.));
#38312=CARTESIAN_POINT('Origin',(-90.,8.,88.9057565652784));
#38313=CARTESIAN_POINT('Ctrl Pts',(-90.,9.76,87.9558091983154));
#38314=CARTESIAN_POINT('Ctrl Pts',(-90.,9.38371079541722,87.2586453099802));
#38315=CARTESIAN_POINT('Ctrl Pts',(-89.7994445608026,8.40693925016618,85.0931803031121));
#38316=CARTESIAN_POINT('Ctrl Pts',(-89.2952937120273,7.73663815324546,81.9896127828507));
#38317=CARTESIAN_POINT('Ctrl Pts',(-89.2986227578434,7.73596845512756,78.8066229943142));
#38318=CARTESIAN_POINT('Ctrl Pts',(-89.5038209708906,8.01646806403338,76.8485723579441));
#38319=CARTESIAN_POINT('Ctrl Pts',(-89.8088181861233,8.59475437500072,74.5592424372745));
#38320=CARTESIAN_POINT('Ctrl Pts',(-90.0000000000027,9.19556619313921,73.0899366341577));
#38321=CARTESIAN_POINT('Ctrl Pts',(-90.,9.7600000000154,72.0441908016561));
#38322=CARTESIAN_POINT('Ctrl Pts',(-90.2991993003419,9.76,87.9558091983154));
#38323=CARTESIAN_POINT('Ctrl Pts',(-90.3169091676255,9.37665509630183,87.2454521299932));
#38324=CARTESIAN_POINT('Ctrl Pts',(-90.1619476924458,8.38826138246784,85.0425306128612));
#38325=CARTESIAN_POINT('Ctrl Pts',(-89.7091767454643,7.73701774875792,81.9500740924077));
#38326=CARTESIAN_POINT('Ctrl Pts',(-89.7131477349571,7.73663955285474,78.8298975124876));
#38327=CARTESIAN_POINT('Ctrl Pts',(-89.8958101886172,8.00865749204959,76.8911873219261));
#38328=CARTESIAN_POINT('Ctrl Pts',(-90.1644704238476,8.58067298580855,74.599875320748));
#38329=CARTESIAN_POINT('Ctrl Pts',(-90.3257641012695,9.18498264446627,73.1097264041378));
#38330=CARTESIAN_POINT('Ctrl Pts',(-90.2991993003412,9.76000000001569,72.0441908016555));
#38331=CARTESIAN_POINT('Ctrl Pts',(-90.895972204776,9.63940333261201,88.0209003839118));
#38332=CARTESIAN_POINT('Ctrl Pts',(-90.9487639764366,9.2243376485348,87.2863405199713));
#38333=CARTESIAN_POINT('Ctrl Pts',(-90.8833386248301,8.15696353645985,85.0104469472155));
#38334=CARTESIAN_POINT('Ctrl Pts',(-90.5313266508363,7.47206531180379,81.9050471896105));
#38335=CARTESIAN_POINT('Ctrl Pts',(-90.5365149718603,7.47226163348177,78.8562489519795));
#38336=CARTESIAN_POINT('Ctrl Pts',(-90.6750800382882,7.75723042413783,76.9297385435099));
#38337=CARTESIAN_POINT('Ctrl Pts',(-90.8723012998031,8.36666124302361,74.6145362955887));
#38338=CARTESIAN_POINT('Ctrl Pts',(-90.9751598622677,9.01680480651077,73.080939411968));
#38339=CARTESIAN_POINT('Ctrl Pts',(-90.8959722047739,9.63940333262899,71.9790996160581));
#38340=CARTESIAN_POINT('Ctrl Pts',(-91.7377173103273,9.05076546339945,88.338613448658));
#38341=CARTESIAN_POINT('Ctrl Pts',(-91.8162525272141,8.53481991552815,87.5747433413596));
#38342=CARTESIAN_POINT('Ctrl Pts',(-91.7960385570055,7.18720898037985,85.2052170002644));
#38343=CARTESIAN_POINT('Ctrl Pts',(-91.4449131702562,6.25099366023525,81.9734225373038));
#38344=CARTESIAN_POINT('Ctrl Pts',(-91.4510308374062,6.25092309230086,78.8151638422316));
#38345=CARTESIAN_POINT('Ctrl Pts',(-91.587647686046,6.64111672717885,76.813793060011));
#38346=CARTESIAN_POINT('Ctrl Pts',(-91.7743660572492,7.44592541337458,74.4042344174921));
#38347=CARTESIAN_POINT('Ctrl Pts',(-91.8555201356577,8.2768471416109,72.8071917122573));
#38348=CARTESIAN_POINT('Ctrl Pts',(-91.7377173103241,9.05076546342056,71.6613865513108));
#38349=CARTESIAN_POINT('Ctrl Pts',(-92.,8.3949430764513,88.6925888746107));
#38350=CARTESIAN_POINT('Ctrl Pts',(-92.0421197771669,7.79643811210926,87.9182301283261));
#38351=CARTESIAN_POINT('Ctrl Pts',(-91.8800131297229,6.2289539284548,85.5139158134625));
#38352=CARTESIAN_POINT('Ctrl Pts',(-91.297671044354,5.1134253012412,82.1307014026271));
#38353=CARTESIAN_POINT('Ctrl Pts',(-91.3026286831461,5.11277842806216,78.7214477499932));
#38354=CARTESIAN_POINT('Ctrl Pts',(-91.5379503533126,5.57872018718012,76.6015467847076));
#38355=CARTESIAN_POINT('Ctrl Pts',(-91.8735935522416,6.52745583762372,74.0962088888192));
#38356=CARTESIAN_POINT('Ctrl Pts',(-92.0631796657526,7.49718562995966,72.4689492447835));
#38357=CARTESIAN_POINT('Ctrl Pts',(-91.9999999999983,8.39494307647579,71.3074111253576));
#38358=CARTESIAN_POINT('Ctrl Pts',(-92.,8.00000000000001,88.9057565652784));
#38359=CARTESIAN_POINT('Ctrl Pts',(-92.,7.36817111170808,88.1253492275899));
#38360=CARTESIAN_POINT('Ctrl Pts',(-91.6991668412039,5.72806963647306,85.7013212348271));
#38361=CARTESIAN_POINT('Ctrl Pts',(-90.942940568041,4.6025640632853,82.2271784882658));
#38362=CARTESIAN_POINT('Ctrl Pts',(-90.947934136765,4.60143957017688,78.6641302175159));
#38363=CARTESIAN_POINT('Ctrl Pts',(-91.255731456336,5.07242771945905,76.4722824902359));
#38364=CARTESIAN_POINT('Ctrl Pts',(-91.713227279185,6.04343085354599,73.9095997432177));
#38365=CARTESIAN_POINT('Ctrl Pts',(-92.0000000000041,7.05225666758454,72.2648544412212));
#38366=CARTESIAN_POINT('Ctrl Pts',(-92.,8.00000000002587,71.0942434346896));
#38367=CARTESIAN_POINT('',(-90.,9.7600000000154,72.0441908016561));
#38368=CARTESIAN_POINT('Origin',(-90.,8.00000000001724,71.0942434346896));
#38369=CARTESIAN_POINT('Ctrl Pts',(-90.,9.76,87.9558091983154));
#38370=CARTESIAN_POINT('Ctrl Pts',(-90.,9.38371079541722,87.2586453099802));
#38371=CARTESIAN_POINT('Ctrl Pts',(-89.7994445608026,8.40693925016618,85.0931803031121));
#38372=CARTESIAN_POINT('Ctrl Pts',(-89.2952937120273,7.73663815324546,81.9896127828507));
#38373=CARTESIAN_POINT('Ctrl Pts',(-89.2986227578434,7.73596845512756,78.8066229943142));
#38374=CARTESIAN_POINT('Ctrl Pts',(-89.5038209708906,8.01646806403338,76.8485723579441));
#38375=CARTESIAN_POINT('Ctrl Pts',(-89.8088181861233,8.59475437500072,74.5592424372745));
#38376=CARTESIAN_POINT('Ctrl Pts',(-90.0000000000027,9.19556619313921,73.0899366341577));
#38377=CARTESIAN_POINT('Ctrl Pts',(-90.,9.7600000000154,72.0441908016561));
#38378=CARTESIAN_POINT('Origin',(-90.,24.5,80.));
#38379=CARTESIAN_POINT('',(-90.,39.24,72.0441908016846));
#38380=CARTESIAN_POINT('',(-92.,41.,71.0942434347216));
#38381=CARTESIAN_POINT('Origin',(-90.,41.,71.0942434347216));
#38382=CARTESIAN_POINT('Origin',(-92.,24.5,80.));
#38383=CARTESIAN_POINT('Origin',(-90.,24.5,80.));
#38384=CARTESIAN_POINT('Ctrl Pts',(-90.,39.24,72.0441908016846));
#38385=CARTESIAN_POINT('Ctrl Pts',(-90.,39.9925784091641,73.4385185783522));
#38386=CARTESIAN_POINT('Ctrl Pts',(-89.6247663405693,40.8156274544243,75.6745310640996));
#38387=CARTESIAN_POINT('Ctrl Pts',(-89.2998530158664,41.2636159206061,78.8054319539897));
#38388=CARTESIAN_POINT('Ctrl Pts',(-89.2947826313159,41.2634913601276,81.9893852835302));
#38389=CARTESIAN_POINT('Ctrl Pts',(-89.7999750759925,40.5929907863548,85.0924696714116));
#38390=CARTESIAN_POINT('Ctrl Pts',(-90.,39.616289204582,87.2586453099816));
#38391=CARTESIAN_POINT('Ctrl Pts',(-90.,39.24,87.9558091983154));
#38392=CARTESIAN_POINT('Ctrl Pts',(-90.2991993003419,39.24,72.0441908016846));
#38393=CARTESIAN_POINT('Ctrl Pts',(-90.3346190349092,40.0066898073949,73.4649049383262));
#38394=CARTESIAN_POINT('Ctrl Pts',(-90.0027743158169,40.8288120390438,75.7289274878841));
#38395=CARTESIAN_POINT('Ctrl Pts',(-89.7146057062682,41.2627924802516,78.8286352385948));
#38396=CARTESIAN_POINT('Ctrl Pts',(-89.7085874510491,41.263157350253,81.9498952398471));
#38397=CARTESIAN_POINT('Ctrl Pts',(-90.1626027926716,40.6115887482669,85.0417658160337));
#38398=CARTESIAN_POINT('Ctrl Pts',(-90.3169091676255,39.6233449036974,87.2454521299946));
#38399=CARTESIAN_POINT('Ctrl Pts',(-90.2991993003419,39.24,87.9558091983154));
#38400=CARTESIAN_POINT('Ctrl Pts',(-90.8959652150227,39.3605997833875,71.9790979342498));
#38401=CARTESIAN_POINT('Ctrl Pts',(-91.0015487583436,40.1907311515403,73.4482176621281));
#38402=CARTESIAN_POINT('Ctrl Pts',(-90.7545425049403,41.0725721868551,75.7748385067781));
#38403=CARTESIAN_POINT('Ctrl Pts',(-90.5385195523907,41.527175389641,78.8549852150399));
#38404=CARTESIAN_POINT('Ctrl Pts',(-90.5305887720886,41.5281747157414,81.9048905937702));
#38405=CARTESIAN_POINT('Ctrl Pts',(-90.8842946702573,40.8429080328227,85.0096550200834));
#38406=CARTESIAN_POINT('Ctrl Pts',(-90.9487569866832,39.7756654674639,87.2863422018111));
#38407=CARTESIAN_POINT('Ctrl Pts',(-90.8959652150227,39.3605997833875,88.0209020657502));
#38408=CARTESIAN_POINT('Ctrl Pts',(-91.7377033118041,39.9492389941977,71.6613841453859));
#38409=CARTESIAN_POINT('Ctrl Pts',(-91.8947737455773,40.9811300899385,73.1891243599799));
#38410=CARTESIAN_POINT('Ctrl Pts',(-91.6657296933045,42.1250155322943,75.6137715678291));
#38411=CARTESIAN_POINT('Ctrl Pts',(-91.45298826703,42.7487257343322,78.813967875551));
#38412=CARTESIAN_POINT('Ctrl Pts',(-91.4440144391444,42.7491210606227,81.9732139614271));
#38413=CARTESIAN_POINT('Ctrl Pts',(-91.796936898282,41.8127986994424,85.204459390508));
#38414=CARTESIAN_POINT('Ctrl Pts',(-91.8162385286907,40.465184542068,87.5747457473173));
#38415=CARTESIAN_POINT('Ctrl Pts',(-91.7377033118041,39.9492389941978,88.3386158546141));
#38416=CARTESIAN_POINT('Ctrl Pts',(-92.,40.6050569235487,71.3074111253893));
#38417=CARTESIAN_POINT('Ctrl Pts',(-92.0842395543337,41.8020668522306,72.8561286179559));
#38418=CARTESIAN_POINT('Ctrl Pts',(-91.6753673714846,43.1416553165424,75.3304959650833));
#38419=CARTESIAN_POINT('Ctrl Pts',(-91.3049054835182,43.8870217698137,78.7201946019518));
#38420=CARTESIAN_POINT('Ctrl Pts',(-91.2970139150267,43.8867145802703,82.1304659587381));
#38421=CARTESIAN_POINT('Ctrl Pts',(-91.8811142330039,42.7711777978929,85.5131266922364));
#38422=CARTESIAN_POINT('Ctrl Pts',(-92.0421197771668,41.2035618878896,87.9182301283276));
#38423=CARTESIAN_POINT('Ctrl Pts',(-92.,40.6050569235487,88.6925888746107));
#38424=CARTESIAN_POINT('Ctrl Pts',(-92.,41.,71.0942434347216));
#38425=CARTESIAN_POINT('Ctrl Pts',(-92.,42.2636577765815,72.6550581100958));
#38426=CARTESIAN_POINT('Ctrl Pts',(-91.4371495108539,43.6456431137721,75.1580571613055));
#38427=CARTESIAN_POINT('Ctrl Pts',(-90.9497795237996,44.3978625532565,78.6627969634214));
#38428=CARTESIAN_POINT('Ctrl Pts',(-90.9421739469738,44.3976534031992,82.2269238248473));
#38429=CARTESIAN_POINT('Ctrl Pts',(-91.6999626139887,43.271812887536,85.7005257515802));
#38430=CARTESIAN_POINT('Ctrl Pts',(-92.,41.6318288882907,88.1253492275915));
#38431=CARTESIAN_POINT('Ctrl Pts',(-92.,41.,88.9057565652784));
#38432=CARTESIAN_POINT('Ctrl Pts',(-92.,41.,88.9057565652784));
#38433=CARTESIAN_POINT('Ctrl Pts',(-92.,41.6318288882907,88.1253492275915));
#38434=CARTESIAN_POINT('Ctrl Pts',(-91.6999626139887,43.271812887536,85.7005257515802));
#38435=CARTESIAN_POINT('Ctrl Pts',(-90.9421739469738,44.3976534031992,82.2269238248473));
#38436=CARTESIAN_POINT('Ctrl Pts',(-90.9497795237996,44.3978625532565,78.6627969634214));
#38437=CARTESIAN_POINT('Ctrl Pts',(-91.4371495108539,43.6456431137721,75.1580571613055));
#38438=CARTESIAN_POINT('Ctrl Pts',(-92.,42.2636577765815,72.6550581100958));
#38439=CARTESIAN_POINT('Ctrl Pts',(-92.,41.,71.0942434347216));
#38440=CARTESIAN_POINT('Ctrl Pts',(-90.,39.24,72.0441908016846));
#38441=CARTESIAN_POINT('Ctrl Pts',(-90.,39.9925784091641,73.4385185783522));
#38442=CARTESIAN_POINT('Ctrl Pts',(-89.6247663405693,40.8156274544243,75.6745310640996));
#38443=CARTESIAN_POINT('Ctrl Pts',(-89.2998530158664,41.2636159206061,78.8054319539897));
#38444=CARTESIAN_POINT('Ctrl Pts',(-89.2947826313159,41.2634913601276,81.9893852835302));
#38445=CARTESIAN_POINT('Ctrl Pts',(-89.7999750759925,40.5929907863548,85.0924696714116));
#38446=CARTESIAN_POINT('Ctrl Pts',(-90.,39.616289204582,87.2586453099816));
#38447=CARTESIAN_POINT('Ctrl Pts',(-90.,39.24,87.9558091983154));
#38448=CARTESIAN_POINT('Origin',(-86.,41.,50.));
#38449=CARTESIAN_POINT('',(-92.,41.,50.));
#38450=CARTESIAN_POINT('',(-86.,47.,50.));
#38451=CARTESIAN_POINT('Origin',(-92.,24.5,80.));
#38452=CARTESIAN_POINT('',(-70.,24.5,96.75));
#38453=CARTESIAN_POINT('',(-92.,24.5,96.75));
#38454=CARTESIAN_POINT('Origin',(-70.,24.5,80.));
#38455=CARTESIAN_POINT('Origin',(-60.,15.,-125.));
#38456=CARTESIAN_POINT('',(-67.,15.,-125.));
#38457=CARTESIAN_POINT('Origin',(60.,15.,-125.));
#38458=CARTESIAN_POINT('',(53.,15.,-125.));
#38459=CARTESIAN_POINT('Origin',(-45.,24.5,114.));
#38460=CARTESIAN_POINT('',(-51.9,24.5,102.));
#38461=CARTESIAN_POINT('',(-51.9,24.5,114.));
#38462=CARTESIAN_POINT('Origin',(-45.,24.5,102.));
#38463=CARTESIAN_POINT('Origin',(-45.,24.5,102.));
#38464=CARTESIAN_POINT('Origin',(45.,24.5,114.));
#38465=CARTESIAN_POINT('',(38.1,24.5,102.));
#38466=CARTESIAN_POINT('',(38.1,24.5,114.));
#38467=CARTESIAN_POINT('Origin',(45.,24.5,102.));
#38468=CARTESIAN_POINT('Origin',(45.,24.5,102.));
#38469=CARTESIAN_POINT('Origin',(0.,24.5,110.));
#38470=CARTESIAN_POINT('',(-16.75,24.5,88.));
#38471=CARTESIAN_POINT('',(-16.75,24.5,110.));
#38472=CARTESIAN_POINT('Origin',(0.,24.5,88.));
#38473=CARTESIAN_POINT('Origin',(0.,24.5,88.));
#38474=CARTESIAN_POINT('Origin',(-70.,24.5,80.));
#38475=CARTESIAN_POINT('Origin',(-92.,41.,50.));
#38476=CARTESIAN_POINT('Origin',(70.,24.5,80.));
#38477=CARTESIAN_POINT('Origin',(92.,8.,50.));
#38478=CARTESIAN_POINT('',(92.,41.,50.));
#38479=CARTESIAN_POINT('',(92.,8.,50.));
#38480=CARTESIAN_POINT('',(92.,41.,50.));
#38481=CARTESIAN_POINT('Origin',(-41.0121933088198,48.,-41.0121933088198));
#38482=CARTESIAN_POINT('',(-46.0621933088198,28.,-41.0121933088198));
#38483=CARTESIAN_POINT('',(-46.0621933088198,48.,-41.0121933088198));
#38484=CARTESIAN_POINT('Origin',(-41.0121933088198,28.,-41.0121933088198));
#38485=CARTESIAN_POINT('Origin',(-41.0121933088198,28.,-41.0121933088198));
#38486=CARTESIAN_POINT('Origin',(-41.0121933088198,48.,41.0121933088198));
#38487=CARTESIAN_POINT('',(-46.0621933088198,28.,41.0121933088198));
#38488=CARTESIAN_POINT('',(-46.0621933088198,48.,41.0121933088198));
#38489=CARTESIAN_POINT('Origin',(-41.0121933088198,28.,41.0121933088198));
#38490=CARTESIAN_POINT('Origin',(-41.0121933088198,28.,41.0121933088198));
#38491=CARTESIAN_POINT('Origin',(41.0121933088198,48.,41.0121933088198));
#38492=CARTESIAN_POINT('',(35.9621933088198,28.,41.0121933088198));
#38493=CARTESIAN_POINT('',(35.9621933088198,48.,41.0121933088198));
#38494=CARTESIAN_POINT('Origin',(41.0121933088198,28.,41.0121933088198));
#38495=CARTESIAN_POINT('Origin',(41.0121933088198,28.,41.0121933088198));
#38496=CARTESIAN_POINT('Origin',(41.0121933088197,48.,-41.0121933088198));
#38497=CARTESIAN_POINT('',(35.9621933088197,28.,-41.0121933088198));
#38498=CARTESIAN_POINT('',(35.9621933088197,48.,-41.0121933088198));
#38499=CARTESIAN_POINT('Origin',(41.0121933088197,28.,-41.0121933088198));
#38500=CARTESIAN_POINT('Origin',(41.0121933088197,28.,-41.0121933088198));
#38501=CARTESIAN_POINT('Origin',(31.3800414539374,0.,-75.7581216659255));
#38502=CARTESIAN_POINT('',(26.3300414539374,20.,-75.7581216659255));
#38503=CARTESIAN_POINT('',(26.3300414539374,0.,-75.7581216659255));
#38504=CARTESIAN_POINT('Origin',(31.3800414539374,20.,-75.7581216659255));
#38505=CARTESIAN_POINT('Origin',(31.3800414539374,20.,-75.7581216659255));
#38506=CARTESIAN_POINT('Origin',(-75.7581216659255,0.,-31.3800414539373));
#38507=CARTESIAN_POINT('',(-80.8081216659255,20.,-31.3800414539373));
#38508=CARTESIAN_POINT('',(-80.8081216659255,0.,-31.3800414539373));
#38509=CARTESIAN_POINT('Origin',(-75.7581216659255,20.,-31.3800414539373));
#38510=CARTESIAN_POINT('Origin',(-75.7581216659255,20.,-31.3800414539373));
#38511=CARTESIAN_POINT('Origin',(-75.7581216659255,0.,31.3800414539374));
#38512=CARTESIAN_POINT('',(-80.8081216659255,20.,31.3800414539374));
#38513=CARTESIAN_POINT('',(-80.8081216659255,0.,31.3800414539374));
#38514=CARTESIAN_POINT('Origin',(-75.7581216659255,20.,31.3800414539374));
#38515=CARTESIAN_POINT('Origin',(-75.7581216659255,20.,31.3800414539374));
#38516=CARTESIAN_POINT('Origin',(31.3800414539374,0.,75.7581216659255));
#38517=CARTESIAN_POINT('',(26.3300414539374,20.,75.7581216659255));
#38518=CARTESIAN_POINT('',(26.3300414539374,0.,75.7581216659255));
#38519=CARTESIAN_POINT('Origin',(31.3800414539374,20.,75.7581216659255));
#38520=CARTESIAN_POINT('Origin',(31.3800414539374,20.,75.7581216659255));
#38521=CARTESIAN_POINT('Origin',(-31.3800414539374,0.,75.7581216659255));
#38522=CARTESIAN_POINT('',(-36.4300414539374,20.,75.7581216659255));
#38523=CARTESIAN_POINT('',(-36.4300414539374,0.,75.7581216659255));
#38524=CARTESIAN_POINT('Origin',(-31.3800414539374,20.,75.7581216659255));
#38525=CARTESIAN_POINT('Origin',(-31.3800414539374,20.,75.7581216659255));
#38526=CARTESIAN_POINT('Origin',(75.7581216659255,0.,31.3800414539374));
#38527=CARTESIAN_POINT('',(70.7081216659255,20.,31.3800414539374));
#38528=CARTESIAN_POINT('',(70.7081216659255,0.,31.3800414539374));
#38529=CARTESIAN_POINT('Origin',(75.7581216659255,20.,31.3800414539374));
#38530=CARTESIAN_POINT('Origin',(75.7581216659255,20.,31.3800414539374));
#38531=CARTESIAN_POINT('Origin',(-31.3800414539373,0.,-75.7581216659255));
#38532=CARTESIAN_POINT('',(-36.4300414539373,20.,-75.7581216659255));
#38533=CARTESIAN_POINT('',(-36.4300414539373,0.,-75.7581216659255));
#38534=CARTESIAN_POINT('Origin',(-31.3800414539373,20.,-75.7581216659255));
#38535=CARTESIAN_POINT('Origin',(-31.3800414539373,20.,-75.7581216659255));
#38536=CARTESIAN_POINT('Origin',(75.7581216659255,0.,-31.3800414539373));
#38537=CARTESIAN_POINT('',(70.7081216659255,20.,-31.3800414539373));
#38538=CARTESIAN_POINT('',(70.7081216659255,0.,-31.3800414539373));
#38539=CARTESIAN_POINT('Origin',(75.7581216659255,20.,-31.3800414539373));
#38540=CARTESIAN_POINT('Origin',(75.7581216659255,20.,-31.3800414539373));
#38541=CARTESIAN_POINT('Origin',(1.77635683940025E-14,9.,-4.70250832716619));
#38542=CARTESIAN_POINT('Origin',(0.,30.,13.));
#38543=CARTESIAN_POINT('',(-1.59204083889156E-15,30.,-13.));
#38544=CARTESIAN_POINT('Origin',(0.,30.,0.));
#38545=CARTESIAN_POINT('Origin',(0.,39.05,0.));
#38546=CARTESIAN_POINT('',(-1.59204083889156E-15,39.05,-13.));
#38547=CARTESIAN_POINT('Origin',(39.,30.5,110.));
#38548=CARTESIAN_POINT('',(39.,33.5,110.));
#38549=CARTESIAN_POINT('Origin',(51.,33.5,110.));
#38550=CARTESIAN_POINT('',(51.,33.5,110.));
#38551=CARTESIAN_POINT('Origin',(51.,30.5,110.));
#38552=CARTESIAN_POINT('',(54.,30.5,110.));
#38553=CARTESIAN_POINT('Origin',(54.,18.5,110.));
#38554=CARTESIAN_POINT('Origin',(-51.,30.5,110.));
#38555=CARTESIAN_POINT('',(-51.,33.5,110.));
#38556=CARTESIAN_POINT('Origin',(-39.,33.5,110.));
#38557=CARTESIAN_POINT('',(-39.,33.5,110.));
#38558=CARTESIAN_POINT('Origin',(-39.,30.5,110.));
#38559=CARTESIAN_POINT('',(-36.,30.5,110.));
#38560=CARTESIAN_POINT('Origin',(-36.,18.5,110.));
#38561=CARTESIAN_POINT('Origin',(-71.,-11.,-140.));
#38562=CARTESIAN_POINT('Origin',(39.,8.00000000000001,-125.));
#38563=CARTESIAN_POINT('',(39.,2.,-125.));
#38564=CARTESIAN_POINT('',(45.,8.,-125.));
#38565=CARTESIAN_POINT('Origin',(-39.,2.,-125.));
#38566=CARTESIAN_POINT('',(-39.,2.,-125.));
#38567=CARTESIAN_POINT('Origin',(-39.,8.00000000000001,-125.));
#38568=CARTESIAN_POINT('',(-45.,8.,-125.));
#38569=CARTESIAN_POINT('Origin',(-45.,36.,-125.));
#38570=CARTESIAN_POINT('',(-45.,36.,-125.));
#38571=CARTESIAN_POINT('Origin',(-39.,36.,-125.));
#38572=CARTESIAN_POINT('',(-39.,42.,-125.));
#38573=CARTESIAN_POINT('Origin',(39.,42.,-125.));
#38574=CARTESIAN_POINT('',(39.,42.,-125.));
#38575=CARTESIAN_POINT('Origin',(39.,36.,-125.));
#38576=CARTESIAN_POINT('',(45.,36.,-125.));
#38577=CARTESIAN_POINT('Origin',(45.,8.,-125.));
#38578=CARTESIAN_POINT('Origin',(0.,24.5,50.));
#38579=CARTESIAN_POINT('',(86.,47.,50.));
#38580=CARTESIAN_POINT('',(43.,47.,50.));
#38581=CARTESIAN_POINT('Origin',(86.,41.,50.));
#38582=CARTESIAN_POINT('Origin',(86.,47.,50.));
#38583=CARTESIAN_POINT('',(86.,47.,50.));
#38584=CARTESIAN_POINT('Origin',(86.,41.,50.));
#38585=CARTESIAN_POINT('',(0.,0.,0.));
#38586=CARTESIAN_POINT('Ctrl Pts',(-3.57453458878627,-16.9981470538884,
-71.8682453580158));
#38587=CARTESIAN_POINT('Ctrl Pts',(-3.57038661518134,-16.9983534204838,
-71.8641633585059));
#38588=CARTESIAN_POINT('Ctrl Pts',(-3.53990786586211,-16.9997799301677,
-71.834280745957));
#38589=CARTESIAN_POINT('Ctrl Pts',(-3.50642976897921,-16.9999870327594,
-71.8016132291015));
#38590=CARTESIAN_POINT('Ctrl Pts',(-3.50104102377553,-17.,-71.7963365978802));
#38591=CARTESIAN_POINT('Ctrl Pts',(-3.50000000000001,-17.,-71.7953186364093));
#38592=CARTESIAN_POINT('Ctrl Pts',(-3.33910484519611,-16.9981470538884,
-72.1036751016059));
#38593=CARTESIAN_POINT('Ctrl Pts',(-3.33497886295621,-16.9983534204838,
-72.0995711107311));
#38594=CARTESIAN_POINT('Ctrl Pts',(-3.30473155320942,-16.9997799301677,
-72.0694570586097));
#38595=CARTESIAN_POINT('Ctrl Pts',(-3.27148136320786,-16.9999870327594,
-72.0365616348729));
#38596=CARTESIAN_POINT('Ctrl Pts',(-3.26613954847709,-17.,-72.0312380731786));
#38597=CARTESIAN_POINT('Ctrl Pts',(-3.26510621213643,-17.,-72.0302124242728));
#38598=CARTESIAN_POINT('Ctrl Pts',(-3.10367510160595,-16.9981470538884,
-72.3391048451961));
#38599=CARTESIAN_POINT('Ctrl Pts',(-3.09957111073108,-16.9983534204838,
-72.3349788629562));
#38600=CARTESIAN_POINT('Ctrl Pts',(-3.06945705860968,-17.0000242835561,
-72.3045547255514));
#38601=CARTESIAN_POINT('Ctrl Pts',(-3.03656163487292,-16.9998354184739,
-72.2714568031683));
#38602=CARTESIAN_POINT('Ctrl Pts',(-3.03123807317866,-17.,-72.2661395484771));
#38603=CARTESIAN_POINT('Ctrl Pts',(-3.03021242427286,-17.,-72.2651062121364));
#38604=CARTESIAN_POINT('Ctrl Pts',(-2.8682453580158,-16.9981470538884,-72.5745345887863));
#38605=CARTESIAN_POINT('Ctrl Pts',(-2.86416335850596,-16.9983534204838,
-72.5703866151813));
#38606=CARTESIAN_POINT('Ctrl Pts',(-2.834280745957,-16.9997799301677,-72.5399078658621));
#38607=CARTESIAN_POINT('Ctrl Pts',(-2.80161322910157,-16.9999870327594,
-72.5064297689792));
#38608=CARTESIAN_POINT('Ctrl Pts',(-2.79633659788023,-17.,-72.5010410237755));
#38609=CARTESIAN_POINT('Ctrl Pts',(-2.79531863640928,-17.,-72.5));
#38610=CARTESIAN_POINT('',(-3.50000000000001,-17.,-71.7953186364093));
#38611=CARTESIAN_POINT('',(-3.57453458878627,-16.9981470538884,-71.8682453580158));
#38612=CARTESIAN_POINT('Ctrl Pts',(-3.50000000000001,-17.,-71.7953186364093));
#38613=CARTESIAN_POINT('Ctrl Pts',(-3.50033136103369,-17.,-71.7956426566413));
#38614=CARTESIAN_POINT('Ctrl Pts',(-3.5006659910395,-16.9999999087783,-71.7959698710105));
#38615=CARTESIAN_POINT('Ctrl Pts',(-3.50107815475911,-16.9999996125274,
-71.7963728195339));
#38616=CARTESIAN_POINT('Ctrl Pts',(-3.50151072778698,-16.9999993016069,
-71.7967957210522));
#38617=CARTESIAN_POINT('Ctrl Pts',(-3.50202849537424,-16.999998768055,-71.7973018394014));
#38618=CARTESIAN_POINT('Ctrl Pts',(-3.50267576544797,-16.9999976134245,
-71.7979344421874));
#38619=CARTESIAN_POINT('Ctrl Pts',(-3.50336536547692,-16.9999963832839,
-71.7986084157221));
#38620=CARTESIAN_POINT('Ctrl Pts',(-3.50420167541479,-16.9999944448324,
-71.7994256794686));
#38621=CARTESIAN_POINT('Ctrl Pts',(-3.50519595537292,-16.9999910006556,
-71.8003972134395));
#38622=CARTESIAN_POINT('Ctrl Pts',(-3.50629355744884,-16.9999871985718,
-71.8014697058443));
#38623=CARTESIAN_POINT('Ctrl Pts',(-3.50758325228922,-16.9999815341953,
-71.8027297908791));
#38624=CARTESIAN_POINT('Ctrl Pts',(-3.50903534240292,-16.9999727872824,
-71.8041484437089));
#38625=CARTESIAN_POINT('Ctrl Pts',(-3.51085714423962,-16.9999618133477,
-71.8059282949086));
#38626=CARTESIAN_POINT('Ctrl Pts',(-3.51293366154212,-16.9999458718544,
-71.8079568545964));
#38627=CARTESIAN_POINT('Ctrl Pts',(-3.51514671247924,-16.9999235237508,
-71.8101187023244));
#38628=CARTESIAN_POINT('Ctrl Pts',(-3.51749449195537,-16.9998998151149,
-71.8124121613864));
#38629=CARTESIAN_POINT('Ctrl Pts',(-3.51999108761033,-16.9998688531822,
-71.8148508937686));
#38630=CARTESIAN_POINT('Ctrl Pts',(-3.52248486630919,-16.9998314674613,
-71.8172869062406));
#38631=CARTESIAN_POINT('Ctrl Pts',(-3.52437422457713,-16.9998031429668,
-71.8191324991581));
#38632=CARTESIAN_POINT('Ctrl Pts',(-3.52626114404881,-16.9997712320714,
-71.820975729331));
#38633=CARTESIAN_POINT('Ctrl Pts',(-3.52810370841093,-16.9997367040829,
-71.8227757579311));
#38634=CARTESIAN_POINT('Ctrl Pts',(-3.52976637007423,-16.9997055473083,
-71.8244000369021));
#38635=CARTESIAN_POINT('Ctrl Pts',(-3.53139250445814,-16.9996723091153,
-71.8259887368555));
#38636=CARTESIAN_POINT('Ctrl Pts',(-3.53298085050798,-16.9996373773349,
-71.8275407505539));
#38637=CARTESIAN_POINT('Ctrl Pts',(-3.53454774391493,-16.9996029173527,
-71.8290718023242));
#38638=CARTESIAN_POINT('Ctrl Pts',(-3.53607719242338,-16.9995668629652,
-71.8305664957214));
#38639=CARTESIAN_POINT('Ctrl Pts',(-3.53760652085725,-16.9995285090951,
-71.8320614739058));
#38640=CARTESIAN_POINT('Ctrl Pts',(-3.53909804395504,-16.9994911033411,
-71.8335194958999));
#38641=CARTESIAN_POINT('Ctrl Pts',(-3.54059613558281,-16.9994513364011,
-71.8349843334469));
#38642=CARTESIAN_POINT('Ctrl Pts',(-3.54213060631552,-16.9994082206029,
-71.8364852326097));
#38643=CARTESIAN_POINT('Ctrl Pts',(-3.54377985735808,-16.9993618796896,
-71.8380984008873));
#38644=CARTESIAN_POINT('Ctrl Pts',(-3.54547077478773,-16.9993116397098,
-71.8397528770164));
#38645=CARTESIAN_POINT('Ctrl Pts',(-3.54719744053076,-16.9992572833264,
-71.8414428847978));
#38646=CARTESIAN_POINT('Ctrl Pts',(-3.54917002631363,-16.9991951852455,
-71.8433735916159));
#38647=CARTESIAN_POINT('Ctrl Pts',(-3.5511887316105,-16.9991276636875,-71.8453501484939));
#38648=CARTESIAN_POINT('Ctrl Pts',(-3.55319701397691,-16.9990563957717,
-71.8473171286809));
#38649=CARTESIAN_POINT('Ctrl Pts',(-3.55597939118123,-16.9989576575524,
-71.8500422837315));
#38650=CARTESIAN_POINT('Ctrl Pts',(-3.55873880452009,-16.9988515979041,
-71.852746171332));
#38651=CARTESIAN_POINT('Ctrl Pts',(-3.56125854441703,-16.9987486082515,
-71.8552161386878));
#38652=CARTESIAN_POINT('Ctrl Pts',(-3.56314834933973,-16.9986713660121,
-71.8570686142047));
#38653=CARTESIAN_POINT('Ctrl Pts',(-3.56490064570704,-16.998596102758,-71.8587868623067));
#38654=CARTESIAN_POINT('Ctrl Pts',(-3.56643959313734,-16.9985278711001,
-71.8602963585416));
#38655=CARTESIAN_POINT('Ctrl Pts',(-3.5677289530966,-16.9984707052957,-71.861561043719));
#38656=CARTESIAN_POINT('Ctrl Pts',(-3.56886818435408,-16.9984185388897,
-71.8626788313976));
#38657=CARTESIAN_POINT('Ctrl Pts',(-3.569838986615,-16.998373289921,-71.8636316653217));
#38658=CARTESIAN_POINT('Ctrl Pts',(-3.5707517147712,-16.9983307477788,-71.8645275000202));
#38659=CARTESIAN_POINT('Ctrl Pts',(-3.57151514502306,-16.9982943574932,
-71.8652771155595));
#38660=CARTESIAN_POINT('Ctrl Pts',(-3.57214502087146,-16.9982640274543,
-71.8658958651527));
#38661=CARTESIAN_POINT('Ctrl Pts',(-3.57273209133855,-16.9982357585976,
-71.8664725654875));
#38662=CARTESIAN_POINT('Ctrl Pts',(-3.57320299278079,-16.9982127623775,
-71.8669354348749));
#38663=CARTESIAN_POINT('Ctrl Pts',(-3.57360188999631,-16.9981931657129,
-71.867327729259));
#38664=CARTESIAN_POINT('Ctrl Pts',(-3.57394979081279,-16.9981760743537,
-71.8676698713729));
#38665=CARTESIAN_POINT('Ctrl Pts',(-3.57424318974085,-16.9981615513357,
-71.8679585937126));
#38666=CARTESIAN_POINT('Ctrl Pts',(-3.57453458878627,-16.9981470538884,
-71.8682453580158));
#38667=CARTESIAN_POINT('',(-2.8682453580158,-16.9981470538884,-72.5745345887863));
#38668=CARTESIAN_POINT('Ctrl Pts',(-2.8682453580158,-16.9981470538884,-72.5745345887863));
#38669=CARTESIAN_POINT('Ctrl Pts',(-3.10367510160595,-16.9981470538884,
-72.3391048451961));
#38670=CARTESIAN_POINT('Ctrl Pts',(-3.33910484519611,-16.9981470538884,
-72.1036751016059));
#38671=CARTESIAN_POINT('Ctrl Pts',(-3.57453458878627,-16.9981470538884,
-71.8682453580158));
#38672=CARTESIAN_POINT('',(-2.79531863640928,-17.,-72.5));
#38673=CARTESIAN_POINT('Ctrl Pts',(-2.8682453580158,-16.9981470538884,-72.5745345887863));
#38674=CARTESIAN_POINT('Ctrl Pts',(-2.86792051198432,-16.9981634765679,
-72.5742044925281));
#38675=CARTESIAN_POINT('Ctrl Pts',(-2.86759246756108,-16.9981799708645,
-72.5738711310018));
#38676=CARTESIAN_POINT('Ctrl Pts',(-2.86718860352499,-16.9982001093812,
-72.57346041281));
#38677=CARTESIAN_POINT('Ctrl Pts',(-2.8667647393911,-16.9982212451946,-72.57302935509));
#38678=CARTESIAN_POINT('Ctrl Pts',(-2.86625756382415,-16.9982463879926,
-72.5725132968389));
#38679=CARTESIAN_POINT('Ctrl Pts',(-2.86562376912052,-16.9982773404549,
-72.5718680115171));
#38680=CARTESIAN_POINT('Ctrl Pts',(-2.86494852089772,-16.9983103173716,
-72.5711805211291));
#38681=CARTESIAN_POINT('Ctrl Pts',(-2.86412982782488,-16.9983498713227,
-72.5703466306137));
#38682=CARTESIAN_POINT('Ctrl Pts',(-2.86315671761944,-16.9983957676602,
-72.5693550535868));
#38683=CARTESIAN_POINT('Ctrl Pts',(-2.86208246075231,-16.9984464345378,
-72.5682604104266));
#38684=CARTESIAN_POINT('Ctrl Pts',(-2.86082042406595,-16.9985047829815,
-72.5669740091159));
#38685=CARTESIAN_POINT('Ctrl Pts',(-2.85939970674286,-16.9985681244217,
-72.565525387959));
#38686=CARTESIAN_POINT('Ctrl Pts',(-2.85761705827721,-16.9986476022457,
-72.5637077270911));
#38687=CARTESIAN_POINT('Ctrl Pts',(-2.85558546640714,-16.9987347812318,
-72.5616355608823));
#38688=CARTESIAN_POINT('Ctrl Pts',(-2.85342062894715,-16.9988223610841,
-72.5594266767905));
#38689=CARTESIAN_POINT('Ctrl Pts',(-2.85112488425853,-16.9989152368701,
-72.5570842219803));
#38690=CARTESIAN_POINT('Ctrl Pts',(-2.84868403352369,-16.9990082804756,
-72.5545928471897));
#38691=CARTESIAN_POINT('Ctrl Pts',(-2.84624625175194,-16.9990947989236,
-72.552103587594));
#38692=CARTESIAN_POINT('Ctrl Pts',(-2.84439897927723,-16.9991603598156,
-72.5502173068831));
#38693=CARTESIAN_POINT('Ctrl Pts',(-2.84255427195847,-16.9992222334679,
-72.5483330647398));
#38694=CARTESIAN_POINT('Ctrl Pts',(-2.84075306394265,-16.9992793054386,
-72.5464926261216));
#38695=CARTESIAN_POINT('Ctrl Pts',(-2.83912769582927,-16.9993308058541,
-72.5448318572274));
#38696=CARTESIAN_POINT('Ctrl Pts',(-2.83753815081148,-16.9993784253393,
-72.543207168852));
#38697=CARTESIAN_POINT('Ctrl Pts',(-2.83598557864455,-16.9994224873957,
-72.5416197584348));
#38698=CARTESIAN_POINT('Ctrl Pts',(-2.83445351746977,-16.9994659673493,
-72.540053319257));
#38699=CARTESIAN_POINT('Ctrl Pts',(-2.83295811821705,-16.9995060035546,
-72.5385238533706));
#38700=CARTESIAN_POINT('Ctrl Pts',(-2.83146270058428,-16.9995437460623,
-72.5369939676884));
#38701=CARTESIAN_POINT('Ctrl Pts',(-2.83000471420189,-16.9995805438512,
-72.5355023760136));
#38702=CARTESIAN_POINT('Ctrl Pts',(-2.82854016663104,-16.9996153196962,
-72.5340037037557));
#38703=CARTESIAN_POINT('Ctrl Pts',(-2.82703981578638,-16.9996485645807,
-72.5324681805947));
#38704=CARTESIAN_POINT('Ctrl Pts',(-2.82542721104073,-16.9996842967954,
-72.5308177719951));
#38705=CARTESIAN_POINT('Ctrl Pts',(-2.82377359513262,-16.9997182120423,
-72.529125149268));
#38706=CARTESIAN_POINT('Ctrl Pts',(-2.82208470500296,-16.9997497930326,
-72.5273963190708));
#38707=CARTESIAN_POINT('Ctrl Pts',(-2.82015515581749,-16.9997858741684,
-72.5254211385423));
#38708=CARTESIAN_POINT('Ctrl Pts',(-2.81818008615893,-16.9998188305302,
-72.5233992312896));
#38709=CARTESIAN_POINT('Ctrl Pts',(-2.81621482751817,-16.9998475191546,
-72.52138736276));
#38710=CARTESIAN_POINT('Ctrl Pts',(-2.81349256857323,-16.9998872583841,
-72.5186005402078));
#38711=CARTESIAN_POINT('Ctrl Pts',(-2.81079201806523,-16.9999185308537,
-72.5158359360068));
#38712=CARTESIAN_POINT('Ctrl Pts',(-2.80832539114039,-16.9999409383933,
-72.5133109478137));
#38713=CARTESIAN_POINT('Ctrl Pts',(-2.80647542094676,-16.9999577440481,
-72.5114172066689));
#38714=CARTESIAN_POINT('Ctrl Pts',(-2.80475967567115,-16.9999696816405,
-72.5096609508553));
#38715=CARTESIAN_POINT('Ctrl Pts',(-2.803252515256,-16.9999780308564,-72.508118309431));
#38716=CARTESIAN_POINT('Ctrl Pts',(-2.80198975715483,-16.999985026157,-72.5068258239488));
#38717=CARTESIAN_POINT('Ctrl Pts',(-2.80087378577512,-16.9999895478102,
-72.5056836631397));
#38718=CARTESIAN_POINT('Ctrl Pts',(-2.79992260032024,-16.9999926045357,
-72.5047102375997));
#38719=CARTESIAN_POINT('Ctrl Pts',(-2.7990283037671,-16.9999954784432,-72.5037950311059));
#38720=CARTESIAN_POINT('Ctrl Pts',(-2.79828008131995,-16.9999970739683,
-72.5030293988184));
#38721=CARTESIAN_POINT('Ctrl Pts',(-2.797662574869,-16.9999980838367,-72.5023976001144));
#38722=CARTESIAN_POINT('Ctrl Pts',(-2.79708702610117,-16.9999990250876,
-72.5018087302087));
#38723=CARTESIAN_POINT('Ctrl Pts',(-2.79662518068282,-16.9999994582021,
-72.5013362750362));
#38724=CARTESIAN_POINT('Ctrl Pts',(-2.79623381941523,-16.9999997079814,
-72.500935978419));
#38725=CARTESIAN_POINT('Ctrl Pts',(-2.79589255313754,-16.9999999257886,
-72.5005869205336));
#38726=CARTESIAN_POINT('Ctrl Pts',(-2.79560461778333,-17.,-72.5002924603909));
#38727=CARTESIAN_POINT('Ctrl Pts',(-2.79531863640928,-17.,-72.5));
#38728=CARTESIAN_POINT('',(-3.14765931820465,-17.,-72.1476593182046));
#38729=CARTESIAN_POINT('Ctrl Pts',(-2.8682453580158,-16.9981470538884,-72.5745345887863));
#38730=CARTESIAN_POINT('Ctrl Pts',(-3.24643975969904,-16.9790273330526,
-72.9588414442702));
#38731=CARTESIAN_POINT('Ctrl Pts',(-3.89283858086127,-16.6911512202391,
-73.5507380181503));
#38732=CARTESIAN_POINT('Ctrl Pts',(-4.4212646197358,-16.0144112572066,-73.9509340499422));
#38733=CARTESIAN_POINT('Ctrl Pts',(-4.50000000000001,-15.6672482052684,
-74.));
#38734=CARTESIAN_POINT('Ctrl Pts',(-4.50000000000001,-15.5,-74.));
#38735=CARTESIAN_POINT('Ctrl Pts',(-3.10367510160595,-16.9981470538884,
-72.3391048451961));
#38736=CARTESIAN_POINT('Ctrl Pts',(-3.48390698788944,-16.9790273330526,
-72.7213742160798));
#38737=CARTESIAN_POINT('Ctrl Pts',(-4.11213839329096,-16.6911512202391,
-73.3314382057206));
#38738=CARTESIAN_POINT('Ctrl Pts',(-4.59782109647127,-16.0144112572066,
-73.7743775732067));
#38739=CARTESIAN_POINT('Ctrl Pts',(-4.66666666666668,-15.6672482052684,
-73.8333333333333));
#38740=CARTESIAN_POINT('Ctrl Pts',(-4.66666666666668,-15.5,-73.8333333333333));
#38741=CARTESIAN_POINT('Ctrl Pts',(-3.33910484519611,-16.9981470538884,
-72.1036751016059));
#38742=CARTESIAN_POINT('Ctrl Pts',(-3.72137421607984,-16.9790273330526,
-72.4839069878894));
#38743=CARTESIAN_POINT('Ctrl Pts',(-4.33143820572064,-16.6911512202391,
-73.112138393291));
#38744=CARTESIAN_POINT('Ctrl Pts',(-4.77437757320675,-16.0144112572066,
-73.5978210964713));
#38745=CARTESIAN_POINT('Ctrl Pts',(-4.83333333333335,-15.6672482052684,
-73.6666666666667));
#38746=CARTESIAN_POINT('Ctrl Pts',(-4.83333333333335,-15.5,-73.6666666666667));
#38747=CARTESIAN_POINT('Ctrl Pts',(-3.57453458878627,-16.9981470538884,
-71.8682453580158));
#38748=CARTESIAN_POINT('Ctrl Pts',(-3.95884144427025,-16.9790273330526,
-72.246439759699));
#38749=CARTESIAN_POINT('Ctrl Pts',(-4.55073801815033,-16.6911512202391,
-72.8928385808613));
#38750=CARTESIAN_POINT('Ctrl Pts',(-4.95093404994221,-16.0144112572066,
-73.4212646197358));
#38751=CARTESIAN_POINT('Ctrl Pts',(-5.00000000000001,-15.6672482052684,
-73.5));
#38752=CARTESIAN_POINT('Ctrl Pts',(-5.00000000000001,-15.5,-73.5));
#38753=CARTESIAN_POINT('',(-5.00000000000001,-15.5,-73.5));
#38754=CARTESIAN_POINT('Ctrl Pts',(-3.57453458878627,-16.9981470538884,
-71.8682453580158));
#38755=CARTESIAN_POINT('Ctrl Pts',(-3.95884144427025,-16.9790273330526,
-72.246439759699));
#38756=CARTESIAN_POINT('Ctrl Pts',(-4.55073801815033,-16.6911512202391,
-72.8928385808613));
#38757=CARTESIAN_POINT('Ctrl Pts',(-4.95093404994221,-16.0144112572066,
-73.4212646197358));
#38758=CARTESIAN_POINT('Ctrl Pts',(-5.00000000000001,-15.6672482052684,
-73.5));
#38759=CARTESIAN_POINT('Ctrl Pts',(-5.00000000000001,-15.5,-73.5));
#38760=CARTESIAN_POINT('',(-4.50000000000001,-15.5,-74.));
#38761=CARTESIAN_POINT('',(-5.00000000000001,-15.5,-73.5));
#38762=CARTESIAN_POINT('Ctrl Pts',(-4.50000000000001,-15.5,-74.));
#38763=CARTESIAN_POINT('Ctrl Pts',(-4.50000000000001,-15.6672482052684,
-74.));
#38764=CARTESIAN_POINT('Ctrl Pts',(-4.4212646197358,-16.0144112572066,-73.9509340499422));
#38765=CARTESIAN_POINT('Ctrl Pts',(-3.89283858086127,-16.6911512202391,
-73.5507380181503));
#38766=CARTESIAN_POINT('Ctrl Pts',(-3.24643975969904,-16.9790273330526,
-72.9588414442702));
#38767=CARTESIAN_POINT('Ctrl Pts',(-2.8682453580158,-16.9981470538884,-72.5745345887863));
#38768=CARTESIAN_POINT('Origin',(-4.75000000000001,-14.,-73.75));
#38769=CARTESIAN_POINT('',(-5.00000000000001,-14.,-73.5));
#38770=CARTESIAN_POINT('',(-4.50000000000001,-14.,-74.));
#38771=CARTESIAN_POINT('',(-44.75,-14.,-33.7500000000002));
#38772=CARTESIAN_POINT('',(-4.50000000000001,-14.,-74.));
#38773=CARTESIAN_POINT('',(-5.00000000000001,-14.,-73.5));
#38774=CARTESIAN_POINT('Origin',(-1.11022302462516E-14,-17.,-62.));
#38775=CARTESIAN_POINT('',(2.79531863640925,-17.,-72.5));
#38776=CARTESIAN_POINT('',(-2.50000000000001,-17.,-72.5));
#38777=CARTESIAN_POINT('',(3.49999999999999,-17.,-71.7953186364093));
#38778=CARTESIAN_POINT('',(3.14765931820462,-17.,-72.1476593182046));
#38779=CARTESIAN_POINT('',(3.49999999999999,-17.,-56.3914887194867));
#38780=CARTESIAN_POINT('',(3.49999999999999,-17.,-68.));
#38781=CARTESIAN_POINT('',(-6.91925441518255E-15,-17.,-56.5));
#38782=CARTESIAN_POINT('Origin',(0.,-17.,0.));
#38783=CARTESIAN_POINT('',(-3.50000000000001,-17.,-56.3914887194867));
#38784=CARTESIAN_POINT('Origin',(0.,-17.,0.));
#38785=CARTESIAN_POINT('',(-3.50000000000001,-17.,-56.));
#38786=CARTESIAN_POINT('Origin',(-2.50000000000001,-15.5,-72.5));
#38787=CARTESIAN_POINT('',(4.49999999999999,-15.5,-74.));
#38788=CARTESIAN_POINT('',(-2.50000000000001,-15.5,-74.));
#38789=CARTESIAN_POINT('',(2.86824535801577,-16.9981470538884,-72.5745345887863));
#38790=CARTESIAN_POINT('Ctrl Pts',(2.86824535801577,-16.9981470538884,-72.5745345887863));
#38791=CARTESIAN_POINT('Ctrl Pts',(3.12037495913793,-16.9854005733312,-72.8307391591089));
#38792=CARTESIAN_POINT('Ctrl Pts',(3.63377877163942,-16.8268077199093,-73.3201733549766));
#38793=CARTESIAN_POINT('Ctrl Pts',(4.13541628736353,-16.3991227020429,-73.7358067305414));
#38794=CARTESIAN_POINT('Ctrl Pts',(4.43902863521563,-15.9274342791999,-73.9615602058987));
#38795=CARTESIAN_POINT('Ctrl Pts',(4.49999999999999,-15.6672482052684,-74.));
#38796=CARTESIAN_POINT('Ctrl Pts',(4.49999999999999,-15.5,-74.));
#38797=CARTESIAN_POINT('Ctrl Pts',(2.79531863640925,-17.,-72.5));
#38798=CARTESIAN_POINT('Ctrl Pts',(2.79564265664125,-17.,-72.5003313610337));
#38799=CARTESIAN_POINT('Ctrl Pts',(2.79596987101048,-16.9999999087783,-72.5006659910395));
#38800=CARTESIAN_POINT('Ctrl Pts',(2.79637281953385,-16.9999996125274,-72.5010781547591));
#38801=CARTESIAN_POINT('Ctrl Pts',(2.79679572105219,-16.9999993016069,-72.501510727787));
#38802=CARTESIAN_POINT('Ctrl Pts',(2.79730183940143,-16.999998768055,-72.5020284953742));
#38803=CARTESIAN_POINT('Ctrl Pts',(2.79793444218738,-16.9999976134245,-72.502675765448));
#38804=CARTESIAN_POINT('Ctrl Pts',(2.79860841572207,-16.9999963832839,-72.5033653654769));
#38805=CARTESIAN_POINT('Ctrl Pts',(2.79942567946863,-16.9999944448324,-72.5042016754148));
#38806=CARTESIAN_POINT('Ctrl Pts',(2.80039721343958,-16.9999910006556,-72.505195955373));
#38807=CARTESIAN_POINT('Ctrl Pts',(2.80146970584441,-16.9999871985718,-72.5062935574489));
#38808=CARTESIAN_POINT('Ctrl Pts',(2.80272979087922,-16.9999815341953,-72.5075832522893));
#38809=CARTESIAN_POINT('Ctrl Pts',(2.80414844370906,-16.9999727872824,-72.5090353424031));
#38810=CARTESIAN_POINT('Ctrl Pts',(2.80592829490883,-16.9999618133477,-72.5108571442398));
#38811=CARTESIAN_POINT('Ctrl Pts',(2.80795685459665,-16.9999458718544,-72.5129336615423));
#38812=CARTESIAN_POINT('Ctrl Pts',(2.81011870232471,-16.9999235237508,-72.5151467124795));
#38813=CARTESIAN_POINT('Ctrl Pts',(2.81241216138656,-16.9998998151149,-72.5174944919555));
#38814=CARTESIAN_POINT('Ctrl Pts',(2.81485089376864,-16.9998688531822,-72.5199910876103));
#38815=CARTESIAN_POINT('Ctrl Pts',(2.81728690624043,-16.9998314674613,-72.522484866309));
#38816=CARTESIAN_POINT('Ctrl Pts',(2.81913249915803,-16.9998031429668,-72.524374224577));
#38817=CARTESIAN_POINT('Ctrl Pts',(2.82097572933092,-16.9997712320714,-72.5262611440487));
#38818=CARTESIAN_POINT('Ctrl Pts',(2.82277575793103,-16.9997367040829,-72.5281037084108));
#38819=CARTESIAN_POINT('Ctrl Pts',(2.82440003690208,-16.9997055473083,-72.5297663700741));
#38820=CARTESIAN_POINT('Ctrl Pts',(2.82598873685543,-16.9996723091153,-72.531392504458));
#38821=CARTESIAN_POINT('Ctrl Pts',(2.82754075055383,-16.9996373773349,-72.5329808505079));
#38822=CARTESIAN_POINT('Ctrl Pts',(2.82907180232415,-16.9996029173527,-72.5345477439148));
#38823=CARTESIAN_POINT('Ctrl Pts',(2.83056649572128,-16.9995668629652,-72.5360771924232));
#38824=CARTESIAN_POINT('Ctrl Pts',(2.83206147390567,-16.9995285090951,-72.5376065208571));
#38825=CARTESIAN_POINT('Ctrl Pts',(2.83351949589972,-16.9994911033411,-72.5390980439549));
#38826=CARTESIAN_POINT('Ctrl Pts',(2.83498433344674,-16.9994513364011,-72.5405961355826));
#38827=CARTESIAN_POINT('Ctrl Pts',(2.83648523260946,-16.9994082206029,-72.5421306063153));
#38828=CARTESIAN_POINT('Ctrl Pts',(2.83809840088706,-16.9993618796896,-72.5437798573578));
#38829=CARTESIAN_POINT('Ctrl Pts',(2.83975287701612,-16.9993116397098,-72.5454707747875));
#38830=CARTESIAN_POINT('Ctrl Pts',(2.84144288479756,-16.9992572833264,-72.5471974405305));
#38831=CARTESIAN_POINT('Ctrl Pts',(2.84337359161558,-16.9991951852455,-72.5491700263133));
#38832=CARTESIAN_POINT('Ctrl Pts',(2.84535014849349,-16.9991276636876,-72.5511887316101));
#38833=CARTESIAN_POINT('Ctrl Pts',(2.84731712868045,-16.9990563957717,-72.5531970139764));
#38834=CARTESIAN_POINT('Ctrl Pts',(2.85004228373103,-16.9989576575525,-72.5559793911808));
#38835=CARTESIAN_POINT('Ctrl Pts',(2.85274617133159,-16.9988515979041,-72.5587388045197));
#38836=CARTESIAN_POINT('Ctrl Pts',(2.8552161386875,-16.9987486082515,-72.5612585444167));
#38837=CARTESIAN_POINT('Ctrl Pts',(2.85706861420443,-16.9986713660121,-72.5631483493394));
#38838=CARTESIAN_POINT('Ctrl Pts',(2.85878686230641,-16.998596102758,-72.5649006457068));
#38839=CARTESIAN_POINT('Ctrl Pts',(2.86029635854136,-16.9985278711001,-72.5664395931371));
#38840=CARTESIAN_POINT('Ctrl Pts',(2.86156104371881,-16.9984707052957,-72.5677289530964));
#38841=CARTESIAN_POINT('Ctrl Pts',(2.8626788313974,-16.9984185388897,-72.5688681843539));
#38842=CARTESIAN_POINT('Ctrl Pts',(2.86363166532155,-16.998373289921,-72.5698389866148));
#38843=CARTESIAN_POINT('Ctrl Pts',(2.8645275000201,-16.9983307477788,-72.5707517147711));
#38844=CARTESIAN_POINT('Ctrl Pts',(2.86527711555933,-16.9982943574932,-72.5715151450229));
#38845=CARTESIAN_POINT('Ctrl Pts',(2.86589586515254,-16.9982640274543,-72.5721450208714));
#38846=CARTESIAN_POINT('Ctrl Pts',(2.8664725654874,-16.9982357585976,-72.5727320913385));
#38847=CARTESIAN_POINT('Ctrl Pts',(2.86693543487485,-16.9982127623775,-72.5732029927807));
#38848=CARTESIAN_POINT('Ctrl Pts',(2.86732772925896,-16.9981931657129,-72.5736018899962));
#38849=CARTESIAN_POINT('Ctrl Pts',(2.86766987137285,-16.9981760743537,-72.5739497908127));
#38850=CARTESIAN_POINT('Ctrl Pts',(2.86795859371254,-16.9981615513357,-72.5742431897408));
#38851=CARTESIAN_POINT('Ctrl Pts',(2.86824535801577,-16.9981470538884,-72.5745345887863));
#38852=CARTESIAN_POINT('Origin',(-5.00000000000001,-14.,-74.));
#38853=CARTESIAN_POINT('',(4.49999999999999,-14.,-74.));
#38854=CARTESIAN_POINT('',(-2.50000000000001,-14.,-74.));
#38855=CARTESIAN_POINT('',(4.49999999999999,-14.,-74.));
#38856=CARTESIAN_POINT('Ctrl Pts',(2.86824535801577,-16.9981470538884,-72.5745345887863));
#38857=CARTESIAN_POINT('Ctrl Pts',(2.86416335850593,-16.9983534204838,-72.5703866151813));
#38858=CARTESIAN_POINT('Ctrl Pts',(2.83428074595699,-16.9997799301677,-72.5399078658621));
#38859=CARTESIAN_POINT('Ctrl Pts',(2.80161322910155,-16.9999870327594,-72.5064297689792));
#38860=CARTESIAN_POINT('Ctrl Pts',(2.79633659788021,-17.,-72.5010410237755));
#38861=CARTESIAN_POINT('Ctrl Pts',(2.79531863640925,-17.,-72.5));
#38862=CARTESIAN_POINT('Ctrl Pts',(3.10367510160593,-16.9981470538884,-72.3391048451961));
#38863=CARTESIAN_POINT('Ctrl Pts',(3.09957111073106,-16.9983534204838,-72.3349788629562));
#38864=CARTESIAN_POINT('Ctrl Pts',(3.06945705860967,-16.9997799301677,-72.3047315532094));
#38865=CARTESIAN_POINT('Ctrl Pts',(3.0365616348729,-16.9999870327594,-72.2714813632078));
#38866=CARTESIAN_POINT('Ctrl Pts',(3.03123807317864,-17.,-72.2661395484771));
#38867=CARTESIAN_POINT('Ctrl Pts',(3.03021242427283,-17.,-72.2651062121364));
#38868=CARTESIAN_POINT('Ctrl Pts',(3.33910484519608,-16.9981470538884,-72.1036751016059));
#38869=CARTESIAN_POINT('Ctrl Pts',(3.33497886295619,-16.9983534204838,-72.0995711107311));
#38870=CARTESIAN_POINT('Ctrl Pts',(3.30455472555143,-17.0000242835561,-72.0694570586097));
#38871=CARTESIAN_POINT('Ctrl Pts',(3.27145680316826,-16.9998354184739,-72.0365616348729));
#38872=CARTESIAN_POINT('Ctrl Pts',(3.26613954847707,-17.,-72.0312380731786));
#38873=CARTESIAN_POINT('Ctrl Pts',(3.26510621213641,-17.,-72.0302124242728));
#38874=CARTESIAN_POINT('Ctrl Pts',(3.57453458878624,-16.9981470538884,-71.8682453580158));
#38875=CARTESIAN_POINT('Ctrl Pts',(3.57038661518131,-16.9983534204838,-71.8641633585059));
#38876=CARTESIAN_POINT('Ctrl Pts',(3.53990786586207,-16.9997799301677,-71.834280745957));
#38877=CARTESIAN_POINT('Ctrl Pts',(3.50642976897918,-16.9999870327594,-71.8016132291015));
#38878=CARTESIAN_POINT('Ctrl Pts',(3.5010410237755,-17.,-71.7963365978802));
#38879=CARTESIAN_POINT('Ctrl Pts',(3.49999999999999,-17.,-71.7953186364093));
#38880=CARTESIAN_POINT('',(3.57453458878624,-16.9981470538884,-71.8682453580158));
#38881=CARTESIAN_POINT('Ctrl Pts',(3.57453458878624,-16.9981470538884,-71.8682453580158));
#38882=CARTESIAN_POINT('Ctrl Pts',(3.33910484519608,-16.9981470538884,-72.1036751016059));
#38883=CARTESIAN_POINT('Ctrl Pts',(3.10367510160593,-16.9981470538884,-72.3391048451961));
#38884=CARTESIAN_POINT('Ctrl Pts',(2.86824535801577,-16.9981470538884,-72.5745345887863));
#38885=CARTESIAN_POINT('Ctrl Pts',(3.57453458878624,-16.9981470538884,-71.8682453580158));
#38886=CARTESIAN_POINT('Ctrl Pts',(3.57420449252802,-16.9981634765679,-71.8679205119843));
#38887=CARTESIAN_POINT('Ctrl Pts',(3.57387113100173,-16.9981799708645,-71.8675924675611));
#38888=CARTESIAN_POINT('Ctrl Pts',(3.57346041281003,-16.9982001093812,-71.867188603525));
#38889=CARTESIAN_POINT('Ctrl Pts',(3.57302935508999,-16.9982212451946,-71.8667647393911));
#38890=CARTESIAN_POINT('Ctrl Pts',(3.57251329683893,-16.9982463879926,-71.8662575638241));
#38891=CARTESIAN_POINT('Ctrl Pts',(3.57186801151713,-16.9982773404549,-71.8656237691205));
#38892=CARTESIAN_POINT('Ctrl Pts',(3.57118052112906,-16.9983103173716,-71.8649485208977));
#38893=CARTESIAN_POINT('Ctrl Pts',(3.57034663061369,-16.9983498713227,-71.8641298278249));
#38894=CARTESIAN_POINT('Ctrl Pts',(3.56935505358675,-16.9983957676602,-71.8631567176194));
#38895=CARTESIAN_POINT('Ctrl Pts',(3.56826041042658,-16.9984464345378,-71.8620824607523));
#38896=CARTESIAN_POINT('Ctrl Pts',(3.56697400911584,-16.9985047829815,-71.8608204240659));
#38897=CARTESIAN_POINT('Ctrl Pts',(3.56552538795898,-16.9985681244217,-71.8593997067428));
#38898=CARTESIAN_POINT('Ctrl Pts',(3.56370772709103,-16.9986476022457,-71.8576170582772));
#38899=CARTESIAN_POINT('Ctrl Pts',(3.56163556088222,-16.9987347812318,-71.8555854664071));
#38900=CARTESIAN_POINT('Ctrl Pts',(3.55942667679046,-16.9988223610841,-71.8534206289471));
#38901=CARTESIAN_POINT('Ctrl Pts',(3.55708422198031,-16.9989152368701,-71.8511248842585));
#38902=CARTESIAN_POINT('Ctrl Pts',(3.5545928471897,-16.9990082804756,-71.8486840335237));
#38903=CARTESIAN_POINT('Ctrl Pts',(3.55210358759401,-16.9990947989236,-71.8462462517519));
#38904=CARTESIAN_POINT('Ctrl Pts',(3.55021730688307,-16.9991603598156,-71.8443989792772));
#38905=CARTESIAN_POINT('Ctrl Pts',(3.5483330647398,-16.9992222334679,-71.8425542719585));
#38906=CARTESIAN_POINT('Ctrl Pts',(3.54649262612161,-16.9992793054386,-71.8407530639426));
#38907=CARTESIAN_POINT('Ctrl Pts',(3.54483185722742,-16.9993308058541,-71.8391276958293));
#38908=CARTESIAN_POINT('Ctrl Pts',(3.54320716885198,-16.9993784253393,-71.8375381508115));
#38909=CARTESIAN_POINT('Ctrl Pts',(3.54161975843479,-16.9994224873957,-71.8359855786445));
#38910=CARTESIAN_POINT('Ctrl Pts',(3.54005331925701,-16.9994659673493,-71.8344535174698));
#38911=CARTESIAN_POINT('Ctrl Pts',(3.53852385337056,-16.9995060035546,-71.832958118217));
#38912=CARTESIAN_POINT('Ctrl Pts',(3.53699396768836,-16.9995437460623,-71.8314627005843));
#38913=CARTESIAN_POINT('Ctrl Pts',(3.53550237601364,-16.9995805438512,-71.8300047142019));
#38914=CARTESIAN_POINT('Ctrl Pts',(3.53400370375569,-16.9996153196962,-71.828540166631));
#38915=CARTESIAN_POINT('Ctrl Pts',(3.53246818059468,-16.9996485645807,-71.8270398157864));
#38916=CARTESIAN_POINT('Ctrl Pts',(3.53081777199505,-16.9996842967954,-71.8254272110407));
#38917=CARTESIAN_POINT('Ctrl Pts',(3.52912514926799,-16.9997182120423,-71.8237735951326));
#38918=CARTESIAN_POINT('Ctrl Pts',(3.5273963190708,-16.9997497930326,-71.822084705003));
#38919=CARTESIAN_POINT('Ctrl Pts',(3.52542113854233,-16.9997858741684,-71.8201551558175));
#38920=CARTESIAN_POINT('Ctrl Pts',(3.52339923128957,-16.9998188305302,-71.8181800861589));
#38921=CARTESIAN_POINT('Ctrl Pts',(3.52138736275993,-16.9998475191546,-71.8162148275182));
#38922=CARTESIAN_POINT('Ctrl Pts',(3.51860054020781,-16.9998872583841,-71.8134925685732));
#38923=CARTESIAN_POINT('Ctrl Pts',(3.51583593600675,-16.9999185308537,-71.8107920180652));
#38924=CARTESIAN_POINT('Ctrl Pts',(3.51331094781367,-16.9999409383933,-71.8083253911404));
#38925=CARTESIAN_POINT('Ctrl Pts',(3.51141720666886,-16.9999577440481,-71.8064754209467));
#38926=CARTESIAN_POINT('Ctrl Pts',(3.50966095085529,-16.9999696816405,-71.8047596756711));
#38927=CARTESIAN_POINT('Ctrl Pts',(3.50811830943094,-16.9999780308564,-71.803252515256));
#38928=CARTESIAN_POINT('Ctrl Pts',(3.50682582394882,-16.999985026157,-71.8019897571548));
#38929=CARTESIAN_POINT('Ctrl Pts',(3.50568366313965,-16.9999895478102,-71.8008737857751));
#38930=CARTESIAN_POINT('Ctrl Pts',(3.5047102375997,-16.9999926045357,-71.7999226003202));
#38931=CARTESIAN_POINT('Ctrl Pts',(3.50379503110591,-16.9999954784432,-71.7990283037671));
#38932=CARTESIAN_POINT('Ctrl Pts',(3.50302939881839,-16.9999970739683,-71.7982800813199));
#38933=CARTESIAN_POINT('Ctrl Pts',(3.50239760011444,-16.9999980838367,-71.797662574869));
#38934=CARTESIAN_POINT('Ctrl Pts',(3.50180873020868,-16.9999990250876,-71.7970870261012));
#38935=CARTESIAN_POINT('Ctrl Pts',(3.50133627503613,-16.9999994582021,-71.7966251806828));
#38936=CARTESIAN_POINT('Ctrl Pts',(3.50093597841901,-16.9999997079814,-71.7962338194152));
#38937=CARTESIAN_POINT('Ctrl Pts',(3.50058692053359,-16.9999999257886,-71.7958925531375));
#38938=CARTESIAN_POINT('Ctrl Pts',(3.50029246039091,-17.,-71.7956046177833));
#38939=CARTESIAN_POINT('Ctrl Pts',(3.49999999999999,-17.,-71.7953186364093));
#38940=CARTESIAN_POINT('Ctrl Pts',(3.57453458878624,-16.9981470538884,-71.8682453580158));
#38941=CARTESIAN_POINT('Ctrl Pts',(3.83073915910889,-16.9854005733312,-72.1203749591379));
#38942=CARTESIAN_POINT('Ctrl Pts',(4.32017335497657,-16.8268077199093,-72.6337787716394));
#38943=CARTESIAN_POINT('Ctrl Pts',(4.7358067305414,-16.3991227020429,-73.1354162873635));
#38944=CARTESIAN_POINT('Ctrl Pts',(4.96156020589869,-15.9274342791999,-73.4390286352156));
#38945=CARTESIAN_POINT('Ctrl Pts',(4.99999999999999,-15.6672482052684,-73.5));
#38946=CARTESIAN_POINT('Ctrl Pts',(4.99999999999999,-15.5,-73.5));
#38947=CARTESIAN_POINT('Ctrl Pts',(3.33910484519608,-16.9981470538884,-72.1036751016059));
#38948=CARTESIAN_POINT('Ctrl Pts',(3.59395109245191,-16.9854005733312,-72.3571630257949));
#38949=CARTESIAN_POINT('Ctrl Pts',(4.09137516053085,-16.8268077199093,-72.8625769660851));
#38950=CARTESIAN_POINT('Ctrl Pts',(4.53567658281545,-16.3991227020429,-73.3355464350895));
#38951=CARTESIAN_POINT('Ctrl Pts',(4.787383015671,-15.9274342791999,-73.6132058254433));
#38952=CARTESIAN_POINT('Ctrl Pts',(4.83333333333332,-15.6672482052684,-73.6666666666667));
#38953=CARTESIAN_POINT('Ctrl Pts',(4.83333333333332,-15.5,-73.6666666666667));
#38954=CARTESIAN_POINT('Ctrl Pts',(3.10367510160593,-16.9981470538884,-72.3391048451961));
#38955=CARTESIAN_POINT('Ctrl Pts',(3.35716302579492,-16.9854005733312,-72.5939510924519));
#38956=CARTESIAN_POINT('Ctrl Pts',(3.86257696608514,-16.8268077199093,-73.0913751605309));
#38957=CARTESIAN_POINT('Ctrl Pts',(4.33554643508949,-16.3991227020429,-73.5356765828154));
#38958=CARTESIAN_POINT('Ctrl Pts',(4.61320582544332,-15.9274342791999,-73.787383015671));
#38959=CARTESIAN_POINT('Ctrl Pts',(4.66666666666665,-15.6672482052684,-73.8333333333333));
#38960=CARTESIAN_POINT('Ctrl Pts',(4.66666666666665,-15.5,-73.8333333333333));
#38961=CARTESIAN_POINT('Ctrl Pts',(2.86824535801577,-16.9981470538884,-72.5745345887863));
#38962=CARTESIAN_POINT('Ctrl Pts',(3.12037495913793,-16.9854005733312,-72.8307391591089));
#38963=CARTESIAN_POINT('Ctrl Pts',(3.63377877163942,-16.8268077199093,-73.3201733549766));
#38964=CARTESIAN_POINT('Ctrl Pts',(4.13541628736353,-16.3991227020429,-73.7358067305414));
#38965=CARTESIAN_POINT('Ctrl Pts',(4.43902863521563,-15.9274342791999,-73.9615602058987));
#38966=CARTESIAN_POINT('Ctrl Pts',(4.49999999999999,-15.6672482052684,-74.));
#38967=CARTESIAN_POINT('Ctrl Pts',(4.49999999999999,-15.5,-74.));
#38968=CARTESIAN_POINT('',(4.99999999999999,-15.5,-73.5));
#38969=CARTESIAN_POINT('',(4.49999999999999,-15.5,-74.));
#38970=CARTESIAN_POINT('Ctrl Pts',(4.99999999999999,-15.5,-73.5));
#38971=CARTESIAN_POINT('Ctrl Pts',(4.99999999999999,-15.6672482052684,-73.5));
#38972=CARTESIAN_POINT('Ctrl Pts',(4.96156020589869,-15.9274342791999,-73.4390286352156));
#38973=CARTESIAN_POINT('Ctrl Pts',(4.7358067305414,-16.3991227020429,-73.1354162873635));
#38974=CARTESIAN_POINT('Ctrl Pts',(4.32017335497657,-16.8268077199093,-72.6337787716394));
#38975=CARTESIAN_POINT('Ctrl Pts',(3.83073915910889,-16.9854005733312,-72.1203749591379));
#38976=CARTESIAN_POINT('Ctrl Pts',(3.57453458878624,-16.9981470538884,-71.8682453580158));
#38977=CARTESIAN_POINT('Origin',(4.74999999999999,-14.,-73.75));
#38978=CARTESIAN_POINT('',(4.99999999999999,-14.,-73.5));
#38979=CARTESIAN_POINT('',(44.75,-14.,-33.7499999999994));
#38980=CARTESIAN_POINT('',(4.99999999999999,-14.,-73.5));
#38981=CARTESIAN_POINT('Origin',(3.49999999999999,-15.5,-68.));
#38982=CARTESIAN_POINT('',(4.99999999999999,-15.5,-56.2783262011229));
#38983=CARTESIAN_POINT('',(4.99999999999999,-15.5,-68.));
#38984=CARTESIAN_POINT('Ctrl Pts',(3.49999999999999,-17.,-56.3914887194867));
#38985=CARTESIAN_POINT('Ctrl Pts',(3.68849285843232,-17.,-56.379789702144));
#38986=CARTESIAN_POINT('Ctrl Pts',(3.88949595769793,-16.9623071985392,-56.366268079425));
#38987=CARTESIAN_POINT('Ctrl Pts',(4.25923828551907,-16.8090480003591,-56.3395353657988));
#38988=CARTESIAN_POINT('Ctrl Pts',(4.42798167302477,-16.6934822832211,-56.3263779287031));
#38989=CARTESIAN_POINT('Ctrl Pts',(4.69412389350912,-16.4270526075957,-56.3048219679644));
#38990=CARTESIAN_POINT('Ctrl Pts',(4.80941523738749,-16.2585410496607,-56.2949857165266));
#38991=CARTESIAN_POINT('Ctrl Pts',(4.96235566707567,-15.889189778178,-56.2817103328366));
#38992=CARTESIAN_POINT('Ctrl Pts',(4.99999999999999,-15.6883461217826,-56.2783262011229));
#38993=CARTESIAN_POINT('Ctrl Pts',(4.99999999999999,-15.5,-56.2783262011229));
#38994=CARTESIAN_POINT('Origin',(4.99999999999999,-14.,-74.));
#38995=CARTESIAN_POINT('',(4.99999999999999,-14.,-56.2783262011229));
#38996=CARTESIAN_POINT('',(5.,-14.,8.5));
#38997=CARTESIAN_POINT('',(4.99999999999999,-16.45,-56.2783262011229));
#38998=CARTESIAN_POINT('Ctrl Pts',(-71.8682453580158,-16.9981470538884,
3.57453458878626));
#38999=CARTESIAN_POINT('Ctrl Pts',(-71.8641633585059,-16.9983534204838,
3.57038661518134));
#39000=CARTESIAN_POINT('Ctrl Pts',(-71.834280745957,-16.9997799301677,3.5399078658621));
#39001=CARTESIAN_POINT('Ctrl Pts',(-71.8016132291015,-16.9999870327594,
3.50642976897921));
#39002=CARTESIAN_POINT('Ctrl Pts',(-71.7963365978802,-17.,3.50104102377552));
#39003=CARTESIAN_POINT('Ctrl Pts',(-71.7953186364093,-17.,3.50000000000001));
#39004=CARTESIAN_POINT('Ctrl Pts',(-72.1036751016059,-16.9981470538884,
3.33910484519611));
#39005=CARTESIAN_POINT('Ctrl Pts',(-72.0995711107311,-16.9983534204838,
3.33497886295621));
#39006=CARTESIAN_POINT('Ctrl Pts',(-72.0694570586097,-16.9997799301677,
3.30473155320942));
#39007=CARTESIAN_POINT('Ctrl Pts',(-72.0365616348729,-16.9999870327594,
3.27148136320786));
#39008=CARTESIAN_POINT('Ctrl Pts',(-72.0312380731786,-17.,3.26613954847709));
#39009=CARTESIAN_POINT('Ctrl Pts',(-72.0302124242728,-17.,3.26510621213643));
#39010=CARTESIAN_POINT('Ctrl Pts',(-72.3391048451961,-16.9981470538884,
3.10367510160595));
#39011=CARTESIAN_POINT('Ctrl Pts',(-72.3349788629562,-16.9983534204838,
3.09957111073108));
#39012=CARTESIAN_POINT('Ctrl Pts',(-72.3045547255514,-17.0000242835561,
3.06945705860968));
#39013=CARTESIAN_POINT('Ctrl Pts',(-72.2714568031683,-16.9998354184739,
3.03656163487291));
#39014=CARTESIAN_POINT('Ctrl Pts',(-72.2661395484771,-17.,3.03123807317866));
#39015=CARTESIAN_POINT('Ctrl Pts',(-72.2651062121364,-17.,3.03021242427285));
#39016=CARTESIAN_POINT('Ctrl Pts',(-72.5745345887863,-16.9981470538884,
2.86824535801579));
#39017=CARTESIAN_POINT('Ctrl Pts',(-72.5703866151813,-16.9983534204838,
2.86416335850595));
#39018=CARTESIAN_POINT('Ctrl Pts',(-72.5399078658621,-16.9997799301677,
2.834280745957));
#39019=CARTESIAN_POINT('Ctrl Pts',(-72.5064297689792,-16.9999870327594,
2.80161322910156));
#39020=CARTESIAN_POINT('Ctrl Pts',(-72.5010410237755,-17.,2.79633659788023));
#39021=CARTESIAN_POINT('Ctrl Pts',(-72.5,-17.,2.79531863640927));
#39022=CARTESIAN_POINT('',(-71.7953186364093,-17.,3.50000000000001));
#39023=CARTESIAN_POINT('',(-71.8682453580158,-16.9981470538884,3.57453458878626));
#39024=CARTESIAN_POINT('Ctrl Pts',(-71.7953186364093,-17.,3.50000000000001));
#39025=CARTESIAN_POINT('Ctrl Pts',(-71.7956426566413,-17.,3.50033136103369));
#39026=CARTESIAN_POINT('Ctrl Pts',(-71.7959698710105,-16.9999999087783,
3.5006659910395));
#39027=CARTESIAN_POINT('Ctrl Pts',(-71.7963728195339,-16.9999996125274,
3.50107815475912));
#39028=CARTESIAN_POINT('Ctrl Pts',(-71.7967957210522,-16.9999993016069,
3.501510727787));
#39029=CARTESIAN_POINT('Ctrl Pts',(-71.7973018394015,-16.999998768055,3.50202849537427));
#39030=CARTESIAN_POINT('Ctrl Pts',(-71.7979344421874,-16.9999976134245,
3.50267576544801));
#39031=CARTESIAN_POINT('Ctrl Pts',(-71.7986084157221,-16.9999963832839,
3.50336536547696));
#39032=CARTESIAN_POINT('Ctrl Pts',(-71.7994256794686,-16.9999944448324,
3.50420167541483));
#39033=CARTESIAN_POINT('Ctrl Pts',(-71.8003972134396,-16.9999910006556,
3.50519595537295));
#39034=CARTESIAN_POINT('Ctrl Pts',(-71.8014697058444,-16.9999871985718,
3.50629355744889));
#39035=CARTESIAN_POINT('Ctrl Pts',(-71.8027297908792,-16.9999815341953,
3.50758325228928));
#39036=CARTESIAN_POINT('Ctrl Pts',(-71.804148443709,-16.9999727872824,3.50903534240298));
#39037=CARTESIAN_POINT('Ctrl Pts',(-71.8059282949087,-16.9999618133477,
3.51085714423967));
#39038=CARTESIAN_POINT('Ctrl Pts',(-71.8079568545964,-16.9999458718544,
3.51293366154214));
#39039=CARTESIAN_POINT('Ctrl Pts',(-71.8101187023244,-16.9999235237508,
3.51514671247923));
#39040=CARTESIAN_POINT('Ctrl Pts',(-71.8124121613863,-16.9998998151149,
3.51749449195529));
#39041=CARTESIAN_POINT('Ctrl Pts',(-71.8148508937685,-16.9998688531822,
3.51999108761016));
#39042=CARTESIAN_POINT('Ctrl Pts',(-71.8172869062403,-16.9998314674613,
3.52248486630895));
#39043=CARTESIAN_POINT('Ctrl Pts',(-71.8191324991579,-16.9998031429668,
3.52437422457693));
#39044=CARTESIAN_POINT('Ctrl Pts',(-71.8209757293309,-16.9997712320714,
3.52626114404865));
#39045=CARTESIAN_POINT('Ctrl Pts',(-71.822775757931,-16.9997367040829,3.52810370841081));
#39046=CARTESIAN_POINT('Ctrl Pts',(-71.824400036902,-16.9997055473083,3.5297663700741));
#39047=CARTESIAN_POINT('Ctrl Pts',(-71.8259887368554,-16.9996723091153,
3.531392504458));
#39048=CARTESIAN_POINT('Ctrl Pts',(-71.8275407505538,-16.9996373773349,
3.53298085050784));
#39049=CARTESIAN_POINT('Ctrl Pts',(-71.8290718023241,-16.9996029173527,
3.53454774391476));
#39050=CARTESIAN_POINT('Ctrl Pts',(-71.8305664957212,-16.9995668629652,
3.53607719242319));
#39051=CARTESIAN_POINT('Ctrl Pts',(-71.8320614739056,-16.9995285090951,
3.53760652085704));
#39052=CARTESIAN_POINT('Ctrl Pts',(-71.8335194958997,-16.9994911033411,
3.53909804395481));
#39053=CARTESIAN_POINT('Ctrl Pts',(-71.8349843334467,-16.9994513364011,
3.54059613558254));
#39054=CARTESIAN_POINT('Ctrl Pts',(-71.8364852326094,-16.9994082206029,
3.54213060631522));
#39055=CARTESIAN_POINT('Ctrl Pts',(-71.838098400887,-16.9993618796896,3.54377985735778));
#39056=CARTESIAN_POINT('Ctrl Pts',(-71.8397528770161,-16.9993116397098,
3.54547077478745));
#39057=CARTESIAN_POINT('Ctrl Pts',(-71.8414428847976,-16.9992572833264,
3.54719744053049));
#39058=CARTESIAN_POINT('Ctrl Pts',(-71.8433735916156,-16.9991951852455,
3.54917002631327));
#39059=CARTESIAN_POINT('Ctrl Pts',(-71.8453501484935,-16.9991276636876,
3.55118873161006));
#39060=CARTESIAN_POINT('Ctrl Pts',(-71.8473171286804,-16.9990563957717,
3.5531970139764));
#39061=CARTESIAN_POINT('Ctrl Pts',(-71.850042283731,-16.9989576575525,3.55597939118077));
#39062=CARTESIAN_POINT('Ctrl Pts',(-71.8527461713316,-16.9988515979041,
3.55873880451969));
#39063=CARTESIAN_POINT('Ctrl Pts',(-71.8552161386875,-16.9987486082515,
3.56125854441668));
#39064=CARTESIAN_POINT('Ctrl Pts',(-71.8570686142045,-16.9986713660121,
3.56314834933943));
#39065=CARTESIAN_POINT('Ctrl Pts',(-71.8587868623064,-16.998596102758,3.56490064570679));
#39066=CARTESIAN_POINT('Ctrl Pts',(-71.8602963585414,-16.9985278711001,
3.56643959313713));
#39067=CARTESIAN_POINT('Ctrl Pts',(-71.8615610437188,-16.9984707052957,
3.56772895309641));
#39068=CARTESIAN_POINT('Ctrl Pts',(-71.8626788313974,-16.9984185388897,
3.56886818435391));
#39069=CARTESIAN_POINT('Ctrl Pts',(-71.8636316653216,-16.998373289921,3.56983898661485));
#39070=CARTESIAN_POINT('Ctrl Pts',(-71.8645275000201,-16.9983307477788,
3.57075171477107));
#39071=CARTESIAN_POINT('Ctrl Pts',(-71.8652771155594,-16.9982943574932,
3.57151514502294));
#39072=CARTESIAN_POINT('Ctrl Pts',(-71.8658958651526,-16.9982640274543,
3.57214502087136));
#39073=CARTESIAN_POINT('Ctrl Pts',(-71.8664725654874,-16.9982357585976,
3.57273209133846));
#39074=CARTESIAN_POINT('Ctrl Pts',(-71.8669354348749,-16.9982127623775,
3.57320299278071));
#39075=CARTESIAN_POINT('Ctrl Pts',(-71.867327729259,-16.9981931657129,3.57360188999624));
#39076=CARTESIAN_POINT('Ctrl Pts',(-71.8676698713729,-16.9981760743537,
3.57394979081275));
#39077=CARTESIAN_POINT('Ctrl Pts',(-71.8679585937125,-16.9981615513357,
3.57424318974083));
#39078=CARTESIAN_POINT('Ctrl Pts',(-71.8682453580158,-16.9981470538884,
3.57453458878627));
#39079=CARTESIAN_POINT('',(-72.5745345887863,-16.9981470538884,2.86824535801579));
#39080=CARTESIAN_POINT('Ctrl Pts',(-72.5745345887863,-16.9981470538884,
2.86824535801579));
#39081=CARTESIAN_POINT('Ctrl Pts',(-72.3391048451961,-16.9981470538884,
3.10367510160595));
#39082=CARTESIAN_POINT('Ctrl Pts',(-72.1036751016059,-16.9981470538884,
3.33910484519611));
#39083=CARTESIAN_POINT('Ctrl Pts',(-71.8682453580158,-16.9981470538884,
3.57453458878626));
#39084=CARTESIAN_POINT('',(-72.5,-17.,2.79531863640927));
#39085=CARTESIAN_POINT('Ctrl Pts',(-72.5745345887863,-16.9981470538884,
2.86824535801579));
#39086=CARTESIAN_POINT('Ctrl Pts',(-72.5742044925281,-16.9981634765679,
2.86792051198432));
#39087=CARTESIAN_POINT('Ctrl Pts',(-72.5738711310018,-16.9981799708645,
2.86759246756108));
#39088=CARTESIAN_POINT('Ctrl Pts',(-72.57346041281,-16.9982001093812,2.86718860352498));
#39089=CARTESIAN_POINT('Ctrl Pts',(-72.57302935509,-16.9982212451946,2.8667647393911));
#39090=CARTESIAN_POINT('Ctrl Pts',(-72.5725132968389,-16.9982463879926,
2.86625756382415));
#39091=CARTESIAN_POINT('Ctrl Pts',(-72.5718680115171,-16.9982773404549,
2.86562376912052));
#39092=CARTESIAN_POINT('Ctrl Pts',(-72.5711805211291,-16.9983103173716,
2.86494852089772));
#39093=CARTESIAN_POINT('Ctrl Pts',(-72.5703466306137,-16.9983498713227,
2.86412982782488));
#39094=CARTESIAN_POINT('Ctrl Pts',(-72.5693550535868,-16.9983957676602,
2.86315671761944));
#39095=CARTESIAN_POINT('Ctrl Pts',(-72.5682604104266,-16.9984464345378,
2.86208246075231));
#39096=CARTESIAN_POINT('Ctrl Pts',(-72.5669740091159,-16.9985047829815,
2.86082042406595));
#39097=CARTESIAN_POINT('Ctrl Pts',(-72.565525387959,-16.9985681244217,2.85939970674287));
#39098=CARTESIAN_POINT('Ctrl Pts',(-72.5637077270911,-16.9986476022457,
2.85761705827722));
#39099=CARTESIAN_POINT('Ctrl Pts',(-72.5616355608823,-16.9987347812318,
2.85558546640715));
#39100=CARTESIAN_POINT('Ctrl Pts',(-72.5594266767905,-16.9988223610841,
2.85342062894716));
#39101=CARTESIAN_POINT('Ctrl Pts',(-72.5570842219804,-16.9989152368701,
2.85112488425854));
#39102=CARTESIAN_POINT('Ctrl Pts',(-72.5545928471897,-16.9990082804756,
2.84868403352371));
#39103=CARTESIAN_POINT('Ctrl Pts',(-72.552103587594,-16.9990947989236,2.84624625175195));
#39104=CARTESIAN_POINT('Ctrl Pts',(-72.5502173068831,-16.9991603598156,
2.84439897927725));
#39105=CARTESIAN_POINT('Ctrl Pts',(-72.5483330647398,-16.9992222334679,
2.84255427195848));
#39106=CARTESIAN_POINT('Ctrl Pts',(-72.5464926261216,-16.9992793054386,
2.84075306394266));
#39107=CARTESIAN_POINT('Ctrl Pts',(-72.5448318572274,-16.9993308058541,
2.83912769582928));
#39108=CARTESIAN_POINT('Ctrl Pts',(-72.543207168852,-16.9993784253393,2.83753815081149));
#39109=CARTESIAN_POINT('Ctrl Pts',(-72.5416197584348,-16.9994224873957,
2.83598557864455));
#39110=CARTESIAN_POINT('Ctrl Pts',(-72.540053319257,-16.9994659673493,2.83445351746978));
#39111=CARTESIAN_POINT('Ctrl Pts',(-72.5385238533706,-16.9995060035546,
2.83295811821706));
#39112=CARTESIAN_POINT('Ctrl Pts',(-72.5369939676884,-16.9995437460623,
2.83146270058429));
#39113=CARTESIAN_POINT('Ctrl Pts',(-72.5355023760137,-16.9995805438512,
2.8300047142019));
#39114=CARTESIAN_POINT('Ctrl Pts',(-72.5340037037557,-16.9996153196962,
2.82854016663104));
#39115=CARTESIAN_POINT('Ctrl Pts',(-72.5324681805947,-16.9996485645807,
2.82703981578639));
#39116=CARTESIAN_POINT('Ctrl Pts',(-72.5308177719951,-16.9996842967954,
2.82542721104074));
#39117=CARTESIAN_POINT('Ctrl Pts',(-72.529125149268,-16.9997182120423,2.82377359513262));
#39118=CARTESIAN_POINT('Ctrl Pts',(-72.5273963190708,-16.9997497930326,
2.82208470500297));
#39119=CARTESIAN_POINT('Ctrl Pts',(-72.5254211385424,-16.9997858741684,
2.82015515581749));
#39120=CARTESIAN_POINT('Ctrl Pts',(-72.5233992312896,-16.9998188305302,
2.81818008615893));
#39121=CARTESIAN_POINT('Ctrl Pts',(-72.52138736276,-16.9998475191546,2.81621482751818));
#39122=CARTESIAN_POINT('Ctrl Pts',(-72.5186005402078,-16.9998872583841,
2.81349256857324));
#39123=CARTESIAN_POINT('Ctrl Pts',(-72.5158359360068,-16.9999185308537,
2.81079201806524));
#39124=CARTESIAN_POINT('Ctrl Pts',(-72.5133109478137,-16.9999409383933,
2.8083253911404));
#39125=CARTESIAN_POINT('Ctrl Pts',(-72.5114172066689,-16.9999577440481,
2.80647542094676));
#39126=CARTESIAN_POINT('Ctrl Pts',(-72.5096609508553,-16.9999696816405,
2.80475967567115));
#39127=CARTESIAN_POINT('Ctrl Pts',(-72.508118309431,-16.9999780308564,2.803252515256));
#39128=CARTESIAN_POINT('Ctrl Pts',(-72.5068258239488,-16.999985026157,2.80198975715482));
#39129=CARTESIAN_POINT('Ctrl Pts',(-72.5056836631397,-16.9999895478102,
2.80087378577512));
#39130=CARTESIAN_POINT('Ctrl Pts',(-72.5047102375997,-16.9999926045357,
2.79992260032024));
#39131=CARTESIAN_POINT('Ctrl Pts',(-72.5037950311059,-16.9999954784432,
2.7990283037671));
#39132=CARTESIAN_POINT('Ctrl Pts',(-72.5030293988184,-16.9999970739683,
2.79828008131995));
#39133=CARTESIAN_POINT('Ctrl Pts',(-72.5023976001144,-16.9999980838367,
2.797662574869));
#39134=CARTESIAN_POINT('Ctrl Pts',(-72.5018087302087,-16.9999990250876,
2.79708702610117));
#39135=CARTESIAN_POINT('Ctrl Pts',(-72.5013362750362,-16.9999994582021,
2.79662518068281));
#39136=CARTESIAN_POINT('Ctrl Pts',(-72.500935978419,-16.9999997079814,2.79623381941523));
#39137=CARTESIAN_POINT('Ctrl Pts',(-72.5005869205336,-16.9999999257886,
2.79589255313754));
#39138=CARTESIAN_POINT('Ctrl Pts',(-72.5002924603909,-17.,2.79560461778333));
#39139=CARTESIAN_POINT('Ctrl Pts',(-72.5,-17.,2.79531863640927));
#39140=CARTESIAN_POINT('',(-72.1476593182046,-17.,3.14765931820464));
#39141=CARTESIAN_POINT('Ctrl Pts',(-72.5745345887863,-16.9981470538884,
2.86824535801579));
#39142=CARTESIAN_POINT('Ctrl Pts',(-72.9588414442702,-16.9790273330526,
3.24643975969903));
#39143=CARTESIAN_POINT('Ctrl Pts',(-73.5507380181504,-16.6911512202391,
3.89283858086127));
#39144=CARTESIAN_POINT('Ctrl Pts',(-73.9509340499422,-16.0144112572066,
4.4212646197358));
#39145=CARTESIAN_POINT('Ctrl Pts',(-74.,-15.6672482052684,4.50000000000001));
#39146=CARTESIAN_POINT('Ctrl Pts',(-74.,-15.5,4.50000000000001));
#39147=CARTESIAN_POINT('Ctrl Pts',(-72.3391048451961,-16.9981470538884,
3.10367510160595));
#39148=CARTESIAN_POINT('Ctrl Pts',(-72.7213742160798,-16.9790273330526,
3.48390698788944));
#39149=CARTESIAN_POINT('Ctrl Pts',(-73.3314382057207,-16.6911512202391,
4.11213839329095));
#39150=CARTESIAN_POINT('Ctrl Pts',(-73.7743775732067,-16.0144112572066,
4.59782109647127));
#39151=CARTESIAN_POINT('Ctrl Pts',(-73.8333333333333,-15.6672482052684,
4.66666666666667));
#39152=CARTESIAN_POINT('Ctrl Pts',(-73.8333333333333,-15.5,4.66666666666667));
#39153=CARTESIAN_POINT('Ctrl Pts',(-72.1036751016059,-16.9981470538884,
3.33910484519611));
#39154=CARTESIAN_POINT('Ctrl Pts',(-72.4839069878894,-16.9790273330526,
3.72137421607984));
#39155=CARTESIAN_POINT('Ctrl Pts',(-73.112138393291,-16.6911512202391,4.33143820572064));
#39156=CARTESIAN_POINT('Ctrl Pts',(-73.5978210964713,-16.0144112572066,
4.77437757320674));
#39157=CARTESIAN_POINT('Ctrl Pts',(-73.6666666666667,-15.6672482052684,
4.83333333333334));
#39158=CARTESIAN_POINT('Ctrl Pts',(-73.6666666666667,-15.5,4.83333333333334));
#39159=CARTESIAN_POINT('Ctrl Pts',(-71.8682453580158,-16.9981470538884,
3.57453458878626));
#39160=CARTESIAN_POINT('Ctrl Pts',(-72.246439759699,-16.9790273330526,3.95884144427024));
#39161=CARTESIAN_POINT('Ctrl Pts',(-72.8928385808613,-16.6911512202391,
4.55073801815033));
#39162=CARTESIAN_POINT('Ctrl Pts',(-73.4212646197358,-16.0144112572066,
4.95093404994221));
#39163=CARTESIAN_POINT('Ctrl Pts',(-73.5,-15.6672482052684,5.00000000000001));
#39164=CARTESIAN_POINT('Ctrl Pts',(-73.5,-15.5,5.00000000000001));
#39165=CARTESIAN_POINT('',(-73.5,-15.5,5.00000000000001));
#39166=CARTESIAN_POINT('Ctrl Pts',(-71.8682453580158,-16.9981470538884,
3.57453458878626));
#39167=CARTESIAN_POINT('Ctrl Pts',(-72.246439759699,-16.9790273330526,3.95884144427024));
#39168=CARTESIAN_POINT('Ctrl Pts',(-72.8928385808613,-16.6911512202391,
4.55073801815033));
#39169=CARTESIAN_POINT('Ctrl Pts',(-73.4212646197358,-16.0144112572066,
4.95093404994221));
#39170=CARTESIAN_POINT('Ctrl Pts',(-73.5,-15.6672482052684,5.00000000000001));
#39171=CARTESIAN_POINT('Ctrl Pts',(-73.5,-15.5,5.00000000000001));
#39172=CARTESIAN_POINT('',(-74.,-15.5,4.50000000000001));
#39173=CARTESIAN_POINT('',(-73.5,-15.5,5.00000000000001));
#39174=CARTESIAN_POINT('Ctrl Pts',(-74.,-15.5,4.50000000000001));
#39175=CARTESIAN_POINT('Ctrl Pts',(-74.,-15.6672482052684,4.50000000000001));
#39176=CARTESIAN_POINT('Ctrl Pts',(-73.9509340499422,-16.0144112572066,
4.4212646197358));
#39177=CARTESIAN_POINT('Ctrl Pts',(-73.5507380181504,-16.6911512202391,
3.89283858086127));
#39178=CARTESIAN_POINT('Ctrl Pts',(-72.9588414442702,-16.9790273330526,
3.24643975969903));
#39179=CARTESIAN_POINT('Ctrl Pts',(-72.5745345887863,-16.9981470538884,
2.86824535801579));
#39180=CARTESIAN_POINT('Origin',(-73.75,-14.,4.75000000000001));
#39181=CARTESIAN_POINT('',(-73.5,-14.,5.));
#39182=CARTESIAN_POINT('',(-74.,-14.,4.50000000000001));
#39183=CARTESIAN_POINT('',(-33.7500000000001,-14.,44.7500000000001));
#39184=CARTESIAN_POINT('',(-74.,-14.,4.50000000000001));
#39185=CARTESIAN_POINT('',(-73.5,-14.,5.00000000000001));
#39186=CARTESIAN_POINT('Origin',(-62.,-17.,7.7715611723761E-15));
#39187=CARTESIAN_POINT('',(-72.5,-17.,-3.49999999999999));
#39188=CARTESIAN_POINT('',(-72.5,-17.,2.50000000000001));
#39189=CARTESIAN_POINT('',(-56.3914887194867,-17.,-3.49999999999999));
#39190=CARTESIAN_POINT('',(-68.,-17.,-3.49999999999999));
#39191=CARTESIAN_POINT('',(-56.3914887194867,-17.,3.50000000000001));
#39192=CARTESIAN_POINT('Origin',(0.,-17.,0.));
#39193=CARTESIAN_POINT('',(-56.,-17.,3.50000000000001));
#39194=CARTESIAN_POINT('Origin',(-72.5,-15.5,2.50000000000001));
#39195=CARTESIAN_POINT('',(-74.,-15.5,-3.49999999999999));
#39196=CARTESIAN_POINT('',(-74.,-15.5,2.50000000000001));
#39197=CARTESIAN_POINT('Origin',(-72.5,-15.5,-3.49999999999999));
#39198=CARTESIAN_POINT('Origin',(-74.,-14.,5.00000000000001));
#39199=CARTESIAN_POINT('',(-74.,-14.,-3.49999999999999));
#39200=CARTESIAN_POINT('',(-74.,-14.,48.));
#39201=CARTESIAN_POINT('',(-74.,-14.,-3.49999999999999));
#39202=CARTESIAN_POINT('Ctrl Pts',(3.57453458878626,-16.9981470538884,71.8682453580158));
#39203=CARTESIAN_POINT('Ctrl Pts',(3.57038661518133,-16.9983534204838,71.8641633585059));
#39204=CARTESIAN_POINT('Ctrl Pts',(3.5399078658621,-16.9997799301677,71.834280745957));
#39205=CARTESIAN_POINT('Ctrl Pts',(3.5064297689792,-16.9999870327594,71.8016132291015));
#39206=CARTESIAN_POINT('Ctrl Pts',(3.50104102377552,-17.,71.7963365978802));
#39207=CARTESIAN_POINT('Ctrl Pts',(3.5,-17.,71.7953186364093));
#39208=CARTESIAN_POINT('Ctrl Pts',(3.3391048451961,-16.9981470538884,72.1036751016059));
#39209=CARTESIAN_POINT('Ctrl Pts',(3.3349788629562,-16.9983534204838,72.0995711107311));
#39210=CARTESIAN_POINT('Ctrl Pts',(3.30473155320942,-16.9997799301677,72.0694570586097));
#39211=CARTESIAN_POINT('Ctrl Pts',(3.27148136320786,-16.9999870327594,72.0365616348729));
#39212=CARTESIAN_POINT('Ctrl Pts',(3.26613954847709,-17.,72.0312380731786));
#39213=CARTESIAN_POINT('Ctrl Pts',(3.26510621213643,-17.,72.0302124242728));
#39214=CARTESIAN_POINT('Ctrl Pts',(3.10367510160595,-16.9981470538884,72.3391048451961));
#39215=CARTESIAN_POINT('Ctrl Pts',(3.09957111073108,-16.9983534204838,72.3349788629562));
#39216=CARTESIAN_POINT('Ctrl Pts',(3.06945705860968,-17.0000242835561,72.3045547255514));
#39217=CARTESIAN_POINT('Ctrl Pts',(3.03656163487291,-16.9998354184739,72.2714568031683));
#39218=CARTESIAN_POINT('Ctrl Pts',(3.03123807317865,-17.,72.2661395484771));
#39219=CARTESIAN_POINT('Ctrl Pts',(3.03021242427285,-17.,72.2651062121364));
#39220=CARTESIAN_POINT('Ctrl Pts',(2.86824535801579,-16.9981470538884,72.5745345887863));
#39221=CARTESIAN_POINT('Ctrl Pts',(2.86416335850595,-16.9983534204838,72.5703866151813));
#39222=CARTESIAN_POINT('Ctrl Pts',(2.83428074595699,-16.9997799301677,72.5399078658621));
#39223=CARTESIAN_POINT('Ctrl Pts',(2.80161322910156,-16.9999870327594,72.5064297689792));
#39224=CARTESIAN_POINT('Ctrl Pts',(2.79633659788022,-17.,72.5010410237755));
#39225=CARTESIAN_POINT('Ctrl Pts',(2.79531863640927,-17.,72.5));
#39226=CARTESIAN_POINT('',(3.5,-17.,71.7953186364093));
#39227=CARTESIAN_POINT('',(3.57453458878626,-16.9981470538884,71.8682453580158));
#39228=CARTESIAN_POINT('Ctrl Pts',(3.50000000000001,-17.,71.7953186364093));
#39229=CARTESIAN_POINT('Ctrl Pts',(3.50033136103368,-17.,71.7956426566413));
#39230=CARTESIAN_POINT('Ctrl Pts',(3.5006659910395,-16.9999999087783,71.7959698710105));
#39231=CARTESIAN_POINT('Ctrl Pts',(3.50107815475912,-16.9999996125274,71.7963728195339));
#39232=CARTESIAN_POINT('Ctrl Pts',(3.50151072778699,-16.9999993016069,71.7967957210522));
#39233=CARTESIAN_POINT('Ctrl Pts',(3.50202849537426,-16.999998768055,71.7973018394015));
#39234=CARTESIAN_POINT('Ctrl Pts',(3.50267576544801,-16.9999976134245,71.7979344421874));
#39235=CARTESIAN_POINT('Ctrl Pts',(3.50336536547695,-16.9999963832839,71.7986084157221));
#39236=CARTESIAN_POINT('Ctrl Pts',(3.50420167541483,-16.9999944448324,71.7994256794686));
#39237=CARTESIAN_POINT('Ctrl Pts',(3.50519595537295,-16.9999910006556,71.8003972134396));
#39238=CARTESIAN_POINT('Ctrl Pts',(3.50629355744888,-16.9999871985718,71.8014697058444));
#39239=CARTESIAN_POINT('Ctrl Pts',(3.50758325228927,-16.9999815341953,71.8027297908792));
#39240=CARTESIAN_POINT('Ctrl Pts',(3.50903534240298,-16.9999727872824,71.804148443709));
#39241=CARTESIAN_POINT('Ctrl Pts',(3.51085714423966,-16.9999618133477,71.8059282949087));
#39242=CARTESIAN_POINT('Ctrl Pts',(3.51293366154214,-16.9999458718544,71.8079568545964));
#39243=CARTESIAN_POINT('Ctrl Pts',(3.51514671247922,-16.9999235237508,71.8101187023244));
#39244=CARTESIAN_POINT('Ctrl Pts',(3.51749449195528,-16.9998998151149,71.8124121613863));
#39245=CARTESIAN_POINT('Ctrl Pts',(3.51999108761016,-16.9998688531822,71.8148508937685));
#39246=CARTESIAN_POINT('Ctrl Pts',(3.52248486630895,-16.9998314674613,71.8172869062403));
#39247=CARTESIAN_POINT('Ctrl Pts',(3.52437422457692,-16.9998031429668,71.8191324991579));
#39248=CARTESIAN_POINT('Ctrl Pts',(3.52626114404864,-16.9997712320714,71.8209757293309));
#39249=CARTESIAN_POINT('Ctrl Pts',(3.5281037084108,-16.9997367040829,71.822775757931));
#39250=CARTESIAN_POINT('Ctrl Pts',(3.52976637007409,-16.9997055473083,71.824400036902));
#39251=CARTESIAN_POINT('Ctrl Pts',(3.531392504458,-16.9996723091153,71.8259887368554));
#39252=CARTESIAN_POINT('Ctrl Pts',(3.53298085050783,-16.9996373773349,71.8275407505538));
#39253=CARTESIAN_POINT('Ctrl Pts',(3.53454774391476,-16.9996029173527,71.8290718023241));
#39254=CARTESIAN_POINT('Ctrl Pts',(3.53607719242319,-16.9995668629652,71.8305664957212));
#39255=CARTESIAN_POINT('Ctrl Pts',(3.53760652085704,-16.9995285090951,71.8320614739056));
#39256=CARTESIAN_POINT('Ctrl Pts',(3.5390980439548,-16.9994911033411,71.8335194958997));
#39257=CARTESIAN_POINT('Ctrl Pts',(3.54059613558254,-16.9994513364011,71.8349843334467));
#39258=CARTESIAN_POINT('Ctrl Pts',(3.54213060631522,-16.9994082206029,71.8364852326094));
#39259=CARTESIAN_POINT('Ctrl Pts',(3.54377985735778,-16.9993618796896,71.838098400887));
#39260=CARTESIAN_POINT('Ctrl Pts',(3.54547077478744,-16.9993116397098,71.8397528770161));
#39261=CARTESIAN_POINT('Ctrl Pts',(3.54719744053048,-16.9992572833264,71.8414428847976));
#39262=CARTESIAN_POINT('Ctrl Pts',(3.54917002631327,-16.9991951852455,71.8433735916156));
#39263=CARTESIAN_POINT('Ctrl Pts',(3.55118873161006,-16.9991276636876,71.8453501484935));
#39264=CARTESIAN_POINT('Ctrl Pts',(3.5531970139764,-16.9990563957717,71.8473171286804));
#39265=CARTESIAN_POINT('Ctrl Pts',(3.55597939118076,-16.9989576575525,71.850042283731));
#39266=CARTESIAN_POINT('Ctrl Pts',(3.55873880451969,-16.9988515979041,71.8527461713316));
#39267=CARTESIAN_POINT('Ctrl Pts',(3.56125854441668,-16.9987486082515,71.8552161386875));
#39268=CARTESIAN_POINT('Ctrl Pts',(3.56314834933942,-16.9986713660121,71.8570686142045));
#39269=CARTESIAN_POINT('Ctrl Pts',(3.56490064570679,-16.998596102758,71.8587868623064));
#39270=CARTESIAN_POINT('Ctrl Pts',(3.56643959313712,-16.9985278711001,71.8602963585414));
#39271=CARTESIAN_POINT('Ctrl Pts',(3.5677289530964,-16.9984707052957,71.8615610437188));
#39272=CARTESIAN_POINT('Ctrl Pts',(3.5688681843539,-16.9984185388897,71.8626788313974));
#39273=CARTESIAN_POINT('Ctrl Pts',(3.56983898661485,-16.998373289921,71.8636316653216));
#39274=CARTESIAN_POINT('Ctrl Pts',(3.57075171477106,-16.9983307477788,71.8645275000201));
#39275=CARTESIAN_POINT('Ctrl Pts',(3.57151514502293,-16.9982943574932,71.8652771155594));
#39276=CARTESIAN_POINT('Ctrl Pts',(3.57214502087136,-16.9982640274543,71.8658958651526));
#39277=CARTESIAN_POINT('Ctrl Pts',(3.57273209133846,-16.9982357585976,71.8664725654874));
#39278=CARTESIAN_POINT('Ctrl Pts',(3.57320299278071,-16.9982127623775,71.8669354348749));
#39279=CARTESIAN_POINT('Ctrl Pts',(3.57360188999624,-16.9981931657129,71.867327729259));
#39280=CARTESIAN_POINT('Ctrl Pts',(3.57394979081275,-16.9981760743537,71.8676698713729));
#39281=CARTESIAN_POINT('Ctrl Pts',(3.57424318974082,-16.9981615513357,71.8679585937125));
#39282=CARTESIAN_POINT('Ctrl Pts',(3.57453458878626,-16.9981470538884,71.8682453580158));
#39283=CARTESIAN_POINT('',(2.86824535801579,-16.9981470538884,72.5745345887863));
#39284=CARTESIAN_POINT('Ctrl Pts',(2.86824535801579,-16.9981470538884,72.5745345887863));
#39285=CARTESIAN_POINT('Ctrl Pts',(3.10367510160595,-16.9981470538884,72.3391048451961));
#39286=CARTESIAN_POINT('Ctrl Pts',(3.3391048451961,-16.9981470538884,72.1036751016059));
#39287=CARTESIAN_POINT('Ctrl Pts',(3.57453458878626,-16.9981470538884,71.8682453580158));
#39288=CARTESIAN_POINT('',(2.79531863640927,-17.,72.5));
#39289=CARTESIAN_POINT('Ctrl Pts',(2.86824535801579,-16.9981470538884,72.5745345887863));
#39290=CARTESIAN_POINT('Ctrl Pts',(2.86792051198431,-16.9981634765679,72.5742044925281));
#39291=CARTESIAN_POINT('Ctrl Pts',(2.86759246756107,-16.9981799708645,72.5738711310018));
#39292=CARTESIAN_POINT('Ctrl Pts',(2.86718860352498,-16.9982001093812,72.57346041281));
#39293=CARTESIAN_POINT('Ctrl Pts',(2.86676473939109,-16.9982212451946,72.57302935509));
#39294=CARTESIAN_POINT('Ctrl Pts',(2.86625756382415,-16.9982463879926,72.5725132968389));
#39295=CARTESIAN_POINT('Ctrl Pts',(2.86562376912052,-16.9982773404549,72.5718680115171));
#39296=CARTESIAN_POINT('Ctrl Pts',(2.86494852089771,-16.9983103173716,72.5711805211291));
#39297=CARTESIAN_POINT('Ctrl Pts',(2.86412982782487,-16.9983498713227,72.5703466306137));
#39298=CARTESIAN_POINT('Ctrl Pts',(2.86315671761944,-16.9983957676602,72.5693550535868));
#39299=CARTESIAN_POINT('Ctrl Pts',(2.86208246075231,-16.9984464345378,72.5682604104266));
#39300=CARTESIAN_POINT('Ctrl Pts',(2.86082042406595,-16.9985047829815,72.5669740091159));
#39301=CARTESIAN_POINT('Ctrl Pts',(2.85939970674287,-16.9985681244217,72.565525387959));
#39302=CARTESIAN_POINT('Ctrl Pts',(2.85761705827722,-16.9986476022457,72.5637077270911));
#39303=CARTESIAN_POINT('Ctrl Pts',(2.85558546640715,-16.9987347812318,72.5616355608823));
#39304=CARTESIAN_POINT('Ctrl Pts',(2.85342062894716,-16.9988223610841,72.5594266767905));
#39305=CARTESIAN_POINT('Ctrl Pts',(2.85112488425854,-16.9989152368701,72.5570842219804));
#39306=CARTESIAN_POINT('Ctrl Pts',(2.84868403352371,-16.9990082804756,72.5545928471897));
#39307=CARTESIAN_POINT('Ctrl Pts',(2.84624625175195,-16.9990947989236,72.552103587594));
#39308=CARTESIAN_POINT('Ctrl Pts',(2.84439897927724,-16.9991603598156,72.5502173068831));
#39309=CARTESIAN_POINT('Ctrl Pts',(2.84255427195848,-16.9992222334679,72.5483330647398));
#39310=CARTESIAN_POINT('Ctrl Pts',(2.84075306394266,-16.9992793054386,72.5464926261216));
#39311=CARTESIAN_POINT('Ctrl Pts',(2.83912769582928,-16.9993308058541,72.5448318572274));
#39312=CARTESIAN_POINT('Ctrl Pts',(2.83753815081149,-16.9993784253393,72.543207168852));
#39313=CARTESIAN_POINT('Ctrl Pts',(2.83598557864455,-16.9994224873957,72.5416197584348));
#39314=CARTESIAN_POINT('Ctrl Pts',(2.83445351746977,-16.9994659673493,72.540053319257));
#39315=CARTESIAN_POINT('Ctrl Pts',(2.83295811821705,-16.9995060035546,72.5385238533706));
#39316=CARTESIAN_POINT('Ctrl Pts',(2.83146270058428,-16.9995437460623,72.5369939676884));
#39317=CARTESIAN_POINT('Ctrl Pts',(2.83000471420189,-16.9995805438512,72.5355023760137));
#39318=CARTESIAN_POINT('Ctrl Pts',(2.82854016663104,-16.9996153196962,72.5340037037557));
#39319=CARTESIAN_POINT('Ctrl Pts',(2.82703981578638,-16.9996485645807,72.5324681805947));
#39320=CARTESIAN_POINT('Ctrl Pts',(2.82542721104074,-16.9996842967954,72.5308177719951));
#39321=CARTESIAN_POINT('Ctrl Pts',(2.82377359513262,-16.9997182120423,72.529125149268));
#39322=CARTESIAN_POINT('Ctrl Pts',(2.82208470500296,-16.9997497930326,72.5273963190708));
#39323=CARTESIAN_POINT('Ctrl Pts',(2.82015515581749,-16.9997858741684,72.5254211385424));
#39324=CARTESIAN_POINT('Ctrl Pts',(2.81818008615893,-16.9998188305302,72.5233992312896));
#39325=CARTESIAN_POINT('Ctrl Pts',(2.81621482751817,-16.9998475191546,72.52138736276));
#39326=CARTESIAN_POINT('Ctrl Pts',(2.81349256857323,-16.9998872583841,72.5186005402078));
#39327=CARTESIAN_POINT('Ctrl Pts',(2.81079201806523,-16.9999185308537,72.5158359360068));
#39328=CARTESIAN_POINT('Ctrl Pts',(2.80832539114039,-16.9999409383933,72.5133109478137));
#39329=CARTESIAN_POINT('Ctrl Pts',(2.80647542094676,-16.9999577440481,72.5114172066689));
#39330=CARTESIAN_POINT('Ctrl Pts',(2.80475967567115,-16.9999696816405,72.5096609508553));
#39331=CARTESIAN_POINT('Ctrl Pts',(2.80325251525599,-16.9999780308564,72.508118309431));
#39332=CARTESIAN_POINT('Ctrl Pts',(2.80198975715482,-16.999985026157,72.5068258239488));
#39333=CARTESIAN_POINT('Ctrl Pts',(2.80087378577512,-16.9999895478102,72.5056836631397));
#39334=CARTESIAN_POINT('Ctrl Pts',(2.79992260032023,-16.9999926045357,72.5047102375997));
#39335=CARTESIAN_POINT('Ctrl Pts',(2.79902830376709,-16.9999954784432,72.5037950311059));
#39336=CARTESIAN_POINT('Ctrl Pts',(2.79828008131994,-16.9999970739683,72.5030293988184));
#39337=CARTESIAN_POINT('Ctrl Pts',(2.79766257486899,-16.9999980838367,72.5023976001144));
#39338=CARTESIAN_POINT('Ctrl Pts',(2.79708702610116,-16.9999990250876,72.5018087302087));
#39339=CARTESIAN_POINT('Ctrl Pts',(2.79662518068281,-16.9999994582021,72.5013362750362));
#39340=CARTESIAN_POINT('Ctrl Pts',(2.79623381941522,-16.9999997079814,72.500935978419));
#39341=CARTESIAN_POINT('Ctrl Pts',(2.79589255313753,-16.9999999257886,72.5005869205336));
#39342=CARTESIAN_POINT('Ctrl Pts',(2.79560461778332,-17.,72.5002924603909));
#39343=CARTESIAN_POINT('Ctrl Pts',(2.79531863640927,-17.,72.5));
#39344=CARTESIAN_POINT('',(3.14765931820464,-17.,72.1476593182046));
#39345=CARTESIAN_POINT('Ctrl Pts',(2.86824535801579,-16.9981470538884,72.5745345887863));
#39346=CARTESIAN_POINT('Ctrl Pts',(3.24643975969903,-16.9790273330526,72.9588414442702));
#39347=CARTESIAN_POINT('Ctrl Pts',(3.89283858086126,-16.6911512202391,73.5507380181503));
#39348=CARTESIAN_POINT('Ctrl Pts',(4.42126461973579,-16.0144112572066,73.9509340499422));
#39349=CARTESIAN_POINT('Ctrl Pts',(4.5,-15.6672482052684,74.));
#39350=CARTESIAN_POINT('Ctrl Pts',(4.5,-15.5,74.));
#39351=CARTESIAN_POINT('Ctrl Pts',(3.10367510160595,-16.9981470538884,72.3391048451961));
#39352=CARTESIAN_POINT('Ctrl Pts',(3.48390698788943,-16.9790273330526,72.7213742160798));
#39353=CARTESIAN_POINT('Ctrl Pts',(4.11213839329095,-16.6911512202391,73.3314382057206));
#39354=CARTESIAN_POINT('Ctrl Pts',(4.59782109647126,-16.0144112572066,73.7743775732067));
#39355=CARTESIAN_POINT('Ctrl Pts',(4.66666666666667,-15.6672482052684,73.8333333333333));
#39356=CARTESIAN_POINT('Ctrl Pts',(4.66666666666667,-15.5,73.8333333333333));
#39357=CARTESIAN_POINT('Ctrl Pts',(3.3391048451961,-16.9981470538884,72.1036751016059));
#39358=CARTESIAN_POINT('Ctrl Pts',(3.72137421607983,-16.9790273330526,72.4839069878894));
#39359=CARTESIAN_POINT('Ctrl Pts',(4.33143820572063,-16.6911512202391,73.112138393291));
#39360=CARTESIAN_POINT('Ctrl Pts',(4.77437757320674,-16.0144112572066,73.5978210964713));
#39361=CARTESIAN_POINT('Ctrl Pts',(4.83333333333334,-15.6672482052684,73.6666666666667));
#39362=CARTESIAN_POINT('Ctrl Pts',(4.83333333333334,-15.5,73.6666666666667));
#39363=CARTESIAN_POINT('Ctrl Pts',(3.57453458878626,-16.9981470538884,71.8682453580158));
#39364=CARTESIAN_POINT('Ctrl Pts',(3.95884144427024,-16.9790273330526,72.246439759699));
#39365=CARTESIAN_POINT('Ctrl Pts',(4.55073801815032,-16.6911512202391,72.8928385808613));
#39366=CARTESIAN_POINT('Ctrl Pts',(4.95093404994221,-16.0144112572066,73.4212646197358));
#39367=CARTESIAN_POINT('Ctrl Pts',(5.,-15.6672482052684,73.5));
#39368=CARTESIAN_POINT('Ctrl Pts',(5.,-15.5,73.5));
#39369=CARTESIAN_POINT('',(5.,-15.5,73.5));
#39370=CARTESIAN_POINT('Ctrl Pts',(3.57453458878626,-16.9981470538884,71.8682453580158));
#39371=CARTESIAN_POINT('Ctrl Pts',(3.95884144427024,-16.9790273330526,72.246439759699));
#39372=CARTESIAN_POINT('Ctrl Pts',(4.55073801815032,-16.6911512202391,72.8928385808613));
#39373=CARTESIAN_POINT('Ctrl Pts',(4.95093404994221,-16.0144112572066,73.4212646197358));
#39374=CARTESIAN_POINT('Ctrl Pts',(5.,-15.6672482052684,73.5));
#39375=CARTESIAN_POINT('Ctrl Pts',(5.,-15.5,73.5));
#39376=CARTESIAN_POINT('',(4.5,-15.5,74.));
#39377=CARTESIAN_POINT('',(5.,-15.5,73.5));
#39378=CARTESIAN_POINT('Ctrl Pts',(4.5,-15.5,74.));
#39379=CARTESIAN_POINT('Ctrl Pts',(4.5,-15.6672482052684,74.));
#39380=CARTESIAN_POINT('Ctrl Pts',(4.42126461973579,-16.0144112572066,73.9509340499422));
#39381=CARTESIAN_POINT('Ctrl Pts',(3.89283858086126,-16.6911512202391,73.5507380181503));
#39382=CARTESIAN_POINT('Ctrl Pts',(3.24643975969903,-16.9790273330526,72.9588414442702));
#39383=CARTESIAN_POINT('Ctrl Pts',(2.86824535801579,-16.9981470538884,72.5745345887863));
#39384=CARTESIAN_POINT('Origin',(4.75,-14.,73.75));
#39385=CARTESIAN_POINT('',(5.,-14.,73.5));
#39386=CARTESIAN_POINT('',(4.5,-14.,74.));
#39387=CARTESIAN_POINT('',(-0.750000000000002,-14.,79.25));
#39388=CARTESIAN_POINT('',(4.5,-14.,74.));
#39389=CARTESIAN_POINT('',(5.,-14.,73.5));
#39390=CARTESIAN_POINT('Origin',(3.33066907387547E-15,-17.,62.));
#39391=CARTESIAN_POINT('',(-2.79531863640926,-17.,72.5));
#39392=CARTESIAN_POINT('',(2.5,-17.,72.5));
#39393=CARTESIAN_POINT('',(-3.5,-17.,71.7953186364093));
#39394=CARTESIAN_POINT('',(-3.14765931820463,-17.,72.1476593182046));
#39395=CARTESIAN_POINT('',(-3.5,-17.,56.3914887194867));
#39396=CARTESIAN_POINT('',(-3.5,-17.,68.));
#39397=CARTESIAN_POINT('',(3.5,-17.,56.3914887194867));
#39398=CARTESIAN_POINT('Origin',(0.,-17.,0.));
#39399=CARTESIAN_POINT('',(3.5,-17.,56.));
#39400=CARTESIAN_POINT('Origin',(2.5,-15.5,72.5));
#39401=CARTESIAN_POINT('',(-4.5,-15.5,74.));
#39402=CARTESIAN_POINT('',(2.5,-15.5,74.));
#39403=CARTESIAN_POINT('',(-2.86824535801578,-16.9981470538884,72.5745345887862));
#39404=CARTESIAN_POINT('Ctrl Pts',(-2.86824535801578,-16.9981470538884,
72.5745345887862));
#39405=CARTESIAN_POINT('Ctrl Pts',(-3.24643975969902,-16.9790273330526,
72.9588414442702));
#39406=CARTESIAN_POINT('Ctrl Pts',(-3.89283858086125,-16.6911512202391,
73.5507380181503));
#39407=CARTESIAN_POINT('Ctrl Pts',(-4.42126461973579,-16.0144112572066,
73.9509340499422));
#39408=CARTESIAN_POINT('Ctrl Pts',(-4.5,-15.6672482052684,74.));
#39409=CARTESIAN_POINT('Ctrl Pts',(-4.5,-15.5,74.));
#39410=CARTESIAN_POINT('Ctrl Pts',(-2.79531863640926,-17.,72.5));
#39411=CARTESIAN_POINT('Ctrl Pts',(-2.79564265664126,-17.,72.5003313610337));
#39412=CARTESIAN_POINT('Ctrl Pts',(-2.79596987101048,-16.9999999087783,
72.5006659910395));
#39413=CARTESIAN_POINT('Ctrl Pts',(-2.79637281953386,-16.9999996125274,
72.5010781547591));
#39414=CARTESIAN_POINT('Ctrl Pts',(-2.7967957210522,-16.9999993016069,72.501510727787));
#39415=CARTESIAN_POINT('Ctrl Pts',(-2.79730183940143,-16.999998768055,72.5020284953742));
#39416=CARTESIAN_POINT('Ctrl Pts',(-2.79793444218738,-16.9999976134245,
72.502675765448));
#39417=CARTESIAN_POINT('Ctrl Pts',(-2.79860841572207,-16.9999963832839,
72.5033653654769));
#39418=CARTESIAN_POINT('Ctrl Pts',(-2.79942567946863,-16.9999944448324,
72.5042016754148));
#39419=CARTESIAN_POINT('Ctrl Pts',(-2.80039721343957,-16.9999910006556,
72.5051959553729));
#39420=CARTESIAN_POINT('Ctrl Pts',(-2.8014697058444,-16.9999871985718,72.5062935574489));
#39421=CARTESIAN_POINT('Ctrl Pts',(-2.80272979087921,-16.9999815341953,
72.5075832522893));
#39422=CARTESIAN_POINT('Ctrl Pts',(-2.80414844370905,-16.9999727872824,
72.509035342403));
#39423=CARTESIAN_POINT('Ctrl Pts',(-2.80592829490881,-16.9999618133477,
72.5108571442398));
#39424=CARTESIAN_POINT('Ctrl Pts',(-2.80795685459662,-16.9999458718544,
72.5129336615423));
#39425=CARTESIAN_POINT('Ctrl Pts',(-2.81011870232467,-16.9999235237508,
72.5151467124795));
#39426=CARTESIAN_POINT('Ctrl Pts',(-2.81241216138654,-16.9998998151149,
72.5174944919555));
#39427=CARTESIAN_POINT('Ctrl Pts',(-2.81485089376864,-16.9998688531822,
72.5199910876103));
#39428=CARTESIAN_POINT('Ctrl Pts',(-2.81728690624045,-16.9998314674613,
72.522484866309));
#39429=CARTESIAN_POINT('Ctrl Pts',(-2.81913249915804,-16.9998031429668,
72.524374224577));
#39430=CARTESIAN_POINT('Ctrl Pts',(-2.82097572933093,-16.9997712320714,
72.5262611440487));
#39431=CARTESIAN_POINT('Ctrl Pts',(-2.82277575793103,-16.9997367040829,
72.5281037084108));
#39432=CARTESIAN_POINT('Ctrl Pts',(-2.82440003690208,-16.9997055473083,
72.5297663700741));
#39433=CARTESIAN_POINT('Ctrl Pts',(-2.82598873685543,-16.9996723091153,
72.531392504458));
#39434=CARTESIAN_POINT('Ctrl Pts',(-2.82754075055383,-16.9996373773349,
72.5329808505079));
#39435=CARTESIAN_POINT('Ctrl Pts',(-2.82907180232415,-16.9996029173527,
72.5345477439148));
#39436=CARTESIAN_POINT('Ctrl Pts',(-2.83056649572128,-16.9995668629652,
72.5360771924232));
#39437=CARTESIAN_POINT('Ctrl Pts',(-2.83206147390568,-16.9995285090951,
72.5376065208571));
#39438=CARTESIAN_POINT('Ctrl Pts',(-2.83351949589972,-16.9994911033411,
72.5390980439549));
#39439=CARTESIAN_POINT('Ctrl Pts',(-2.83498433344674,-16.9994513364011,
72.5405961355826));
#39440=CARTESIAN_POINT('Ctrl Pts',(-2.83648523260947,-16.9994082206029,
72.5421306063153));
#39441=CARTESIAN_POINT('Ctrl Pts',(-2.83809840088706,-16.9993618796896,
72.5437798573578));
#39442=CARTESIAN_POINT('Ctrl Pts',(-2.83975287701613,-16.9993116397098,
72.5454707747875));
#39443=CARTESIAN_POINT('Ctrl Pts',(-2.84144288479758,-16.9992572833264,
72.5471974405305));
#39444=CARTESIAN_POINT('Ctrl Pts',(-2.84337359161561,-16.9991951852455,
72.5491700263133));
#39445=CARTESIAN_POINT('Ctrl Pts',(-2.84535014849355,-16.9991276636876,
72.5511887316101));
#39446=CARTESIAN_POINT('Ctrl Pts',(-2.84731712868052,-16.9990563957717,
72.5531970139765));
#39447=CARTESIAN_POINT('Ctrl Pts',(-2.85004228373109,-16.9989576575525,
72.5559793911808));
#39448=CARTESIAN_POINT('Ctrl Pts',(-2.85274617133165,-16.9988515979041,
72.5587388045197));
#39449=CARTESIAN_POINT('Ctrl Pts',(-2.85521613868755,-16.9987486082515,
72.5612585444167));
#39450=CARTESIAN_POINT('Ctrl Pts',(-2.85706861420448,-16.9986713660121,
72.5631483493395));
#39451=CARTESIAN_POINT('Ctrl Pts',(-2.85878686230645,-16.998596102758,72.5649006457068));
#39452=CARTESIAN_POINT('Ctrl Pts',(-2.86029635854139,-16.9985278711001,
72.5664395931371));
#39453=CARTESIAN_POINT('Ctrl Pts',(-2.86156104371884,-16.9984707052957,
72.5677289530964));
#39454=CARTESIAN_POINT('Ctrl Pts',(-2.86267883139743,-16.9984185388897,
72.5688681843539));
#39455=CARTESIAN_POINT('Ctrl Pts',(-2.86363166532158,-16.998373289921,72.5698389866149));
#39456=CARTESIAN_POINT('Ctrl Pts',(-2.86452750002013,-16.9983307477788,
72.5707517147711));
#39457=CARTESIAN_POINT('Ctrl Pts',(-2.86527711555935,-16.9982943574932,
72.5715151450229));
#39458=CARTESIAN_POINT('Ctrl Pts',(-2.86589586515256,-16.9982640274543,
72.5721450208714));
#39459=CARTESIAN_POINT('Ctrl Pts',(-2.86647256548742,-16.9982357585976,
72.5727320913385));
#39460=CARTESIAN_POINT('Ctrl Pts',(-2.86693543487487,-16.9982127623775,
72.5732029927807));
#39461=CARTESIAN_POINT('Ctrl Pts',(-2.86732772925898,-16.9981931657129,
72.5736018899962));
#39462=CARTESIAN_POINT('Ctrl Pts',(-2.86766987137286,-16.9981760743537,
72.5739497908127));
#39463=CARTESIAN_POINT('Ctrl Pts',(-2.86795859371255,-16.9981615513357,
72.5742431897408));
#39464=CARTESIAN_POINT('Ctrl Pts',(-2.86824535801578,-16.9981470538884,
72.5745345887862));
#39465=CARTESIAN_POINT('Origin',(5.,-14.,74.));
#39466=CARTESIAN_POINT('',(-4.49999999999999,-14.,74.));
#39467=CARTESIAN_POINT('',(2.5,-14.,74.));
#39468=CARTESIAN_POINT('',(-4.49999999999999,-14.,74.));
#39469=CARTESIAN_POINT('Ctrl Pts',(-2.86824535801578,-16.9981470538884,
72.5745345887862));
#39470=CARTESIAN_POINT('Ctrl Pts',(-2.86416335850594,-16.9983534204838,
72.5703866151813));
#39471=CARTESIAN_POINT('Ctrl Pts',(-2.834280745957,-16.9997799301677,72.5399078658621));
#39472=CARTESIAN_POINT('Ctrl Pts',(-2.80161322910155,-16.9999870327594,
72.5064297689792));
#39473=CARTESIAN_POINT('Ctrl Pts',(-2.79633659788021,-17.,72.5010410237755));
#39474=CARTESIAN_POINT('Ctrl Pts',(-2.79531863640926,-17.,72.5));
#39475=CARTESIAN_POINT('Ctrl Pts',(-3.10367510160593,-16.9981470538884,
72.3391048451961));
#39476=CARTESIAN_POINT('Ctrl Pts',(-3.09957111073106,-16.9983534204838,
72.3349788629562));
#39477=CARTESIAN_POINT('Ctrl Pts',(-3.06945705860968,-16.9997799301677,
72.3047315532094));
#39478=CARTESIAN_POINT('Ctrl Pts',(-3.0365616348729,-16.9999870327594,72.2714813632078));
#39479=CARTESIAN_POINT('Ctrl Pts',(-3.03123807317865,-17.,72.2661395484771));
#39480=CARTESIAN_POINT('Ctrl Pts',(-3.03021242427284,-17.,72.2651062121364));
#39481=CARTESIAN_POINT('Ctrl Pts',(-3.33910484519609,-16.9981470538884,
72.1036751016059));
#39482=CARTESIAN_POINT('Ctrl Pts',(-3.33497886295619,-16.9983534204838,
72.0995711107311));
#39483=CARTESIAN_POINT('Ctrl Pts',(-3.30455472555143,-17.0000242835561,
72.0694570586097));
#39484=CARTESIAN_POINT('Ctrl Pts',(-3.27145680316828,-16.9998354184739,
72.0365616348729));
#39485=CARTESIAN_POINT('Ctrl Pts',(-3.26613954847708,-17.,72.0312380731786));
#39486=CARTESIAN_POINT('Ctrl Pts',(-3.26510621213642,-17.,72.0302124242728));
#39487=CARTESIAN_POINT('Ctrl Pts',(-3.57453458878625,-16.9981470538884,
71.8682453580158));
#39488=CARTESIAN_POINT('Ctrl Pts',(-3.57038661518132,-16.9983534204838,
71.8641633585059));
#39489=CARTESIAN_POINT('Ctrl Pts',(-3.53990786586207,-16.9997799301677,
71.834280745957));
#39490=CARTESIAN_POINT('Ctrl Pts',(-3.5064297689792,-16.9999870327594,71.8016132291015));
#39491=CARTESIAN_POINT('Ctrl Pts',(-3.50104102377551,-17.,71.7963365978802));
#39492=CARTESIAN_POINT('Ctrl Pts',(-3.5,-17.,71.7953186364093));
#39493=CARTESIAN_POINT('',(-3.57453458878625,-16.9981470538884,71.8682453580158));
#39494=CARTESIAN_POINT('Ctrl Pts',(-3.57453458878625,-16.9981470538884,
71.8682453580158));
#39495=CARTESIAN_POINT('Ctrl Pts',(-3.33910484519609,-16.9981470538884,
72.1036751016059));
#39496=CARTESIAN_POINT('Ctrl Pts',(-3.10367510160593,-16.9981470538884,
72.3391048451961));
#39497=CARTESIAN_POINT('Ctrl Pts',(-2.86824535801578,-16.9981470538884,
72.5745345887862));
#39498=CARTESIAN_POINT('Ctrl Pts',(-3.57453458878625,-16.9981470538884,
71.8682453580158));
#39499=CARTESIAN_POINT('Ctrl Pts',(-3.57420449252803,-16.9981634765679,
71.8679205119843));
#39500=CARTESIAN_POINT('Ctrl Pts',(-3.57387113100174,-16.9981799708645,
71.8675924675611));
#39501=CARTESIAN_POINT('Ctrl Pts',(-3.57346041281003,-16.9982001093812,
71.867188603525));
#39502=CARTESIAN_POINT('Ctrl Pts',(-3.57302935509,-16.9982212451947,71.8667647393911));
#39503=CARTESIAN_POINT('Ctrl Pts',(-3.57251329683894,-16.9982463879926,
71.8662575638241));
#39504=CARTESIAN_POINT('Ctrl Pts',(-3.57186801151713,-16.9982773404549,
71.8656237691205));
#39505=CARTESIAN_POINT('Ctrl Pts',(-3.57118052112907,-16.9983103173716,
71.8649485208977));
#39506=CARTESIAN_POINT('Ctrl Pts',(-3.57034663061369,-16.9983498713227,
71.8641298278249));
#39507=CARTESIAN_POINT('Ctrl Pts',(-3.56935505358675,-16.9983957676602,
71.8631567176194));
#39508=CARTESIAN_POINT('Ctrl Pts',(-3.56826041042659,-16.9984464345378,
71.8620824607523));
#39509=CARTESIAN_POINT('Ctrl Pts',(-3.56697400911585,-16.9985047829815,
71.8608204240659));
#39510=CARTESIAN_POINT('Ctrl Pts',(-3.56552538795899,-16.9985681244217,
71.8593997067428));
#39511=CARTESIAN_POINT('Ctrl Pts',(-3.56370772709106,-16.9986476022457,
71.8576170582772));
#39512=CARTESIAN_POINT('Ctrl Pts',(-3.56163556088227,-16.9987347812318,
71.8555854664071));
#39513=CARTESIAN_POINT('Ctrl Pts',(-3.55942667679054,-16.9988223610841,
71.8534206289472));
#39514=CARTESIAN_POINT('Ctrl Pts',(-3.55708422198037,-16.9989152368701,
71.8511248842585));
#39515=CARTESIAN_POINT('Ctrl Pts',(-3.55459284718975,-16.9990082804756,
71.8486840335237));
#39516=CARTESIAN_POINT('Ctrl Pts',(-3.55210358759403,-16.9990947989236,
71.8462462517519));
#39517=CARTESIAN_POINT('Ctrl Pts',(-3.55021730688309,-16.9991603598156,
71.8443989792772));
#39518=CARTESIAN_POINT('Ctrl Pts',(-3.54833306473982,-16.9992222334679,
71.8425542719585));
#39519=CARTESIAN_POINT('Ctrl Pts',(-3.54649262612163,-16.9992793054386,
71.8407530639427));
#39520=CARTESIAN_POINT('Ctrl Pts',(-3.54483185722744,-16.9993308058541,
71.8391276958293));
#39521=CARTESIAN_POINT('Ctrl Pts',(-3.543207168852,-16.9993784253393,71.8375381508115));
#39522=CARTESIAN_POINT('Ctrl Pts',(-3.5416197584348,-16.9994224873957,71.8359855786445));
#39523=CARTESIAN_POINT('Ctrl Pts',(-3.54005331925703,-16.9994659673493,
71.8344535174698));
#39524=CARTESIAN_POINT('Ctrl Pts',(-3.53852385337057,-16.9995060035546,
71.8329581182171));
#39525=CARTESIAN_POINT('Ctrl Pts',(-3.53699396768837,-16.9995437460623,
71.8314627005843));
#39526=CARTESIAN_POINT('Ctrl Pts',(-3.53550237601366,-16.9995805438512,
71.8300047142019));
#39527=CARTESIAN_POINT('Ctrl Pts',(-3.53400370375571,-16.9996153196962,
71.828540166631));
#39528=CARTESIAN_POINT('Ctrl Pts',(-3.5324681805947,-16.9996485645807,71.8270398157864));
#39529=CARTESIAN_POINT('Ctrl Pts',(-3.53081777199506,-16.9996842967954,
71.8254272110407));
#39530=CARTESIAN_POINT('Ctrl Pts',(-3.529125149268,-16.9997182120423,71.8237735951326));
#39531=CARTESIAN_POINT('Ctrl Pts',(-3.52739631907081,-16.9997497930326,
71.8220847050029));
#39532=CARTESIAN_POINT('Ctrl Pts',(-3.52542113854234,-16.9997858741684,
71.8201551558175));
#39533=CARTESIAN_POINT('Ctrl Pts',(-3.52339923128959,-16.9998188305302,
71.8181800861589));
#39534=CARTESIAN_POINT('Ctrl Pts',(-3.52138736275996,-16.9998475191546,
71.8162148275182));
#39535=CARTESIAN_POINT('Ctrl Pts',(-3.51860054020783,-16.9998872583841,
71.8134925685732));
#39536=CARTESIAN_POINT('Ctrl Pts',(-3.51583593600677,-16.9999185308537,
71.8107920180652));
#39537=CARTESIAN_POINT('Ctrl Pts',(-3.51331094781369,-16.9999409383933,
71.8083253911404));
#39538=CARTESIAN_POINT('Ctrl Pts',(-3.51141720666888,-16.9999577440481,
71.8064754209467));
#39539=CARTESIAN_POINT('Ctrl Pts',(-3.50966095085531,-16.9999696816405,
71.8047596756711));
#39540=CARTESIAN_POINT('Ctrl Pts',(-3.50811830943095,-16.9999780308564,
71.803252515256));
#39541=CARTESIAN_POINT('Ctrl Pts',(-3.50682582394883,-16.999985026157,71.8019897571548));
#39542=CARTESIAN_POINT('Ctrl Pts',(-3.50568366313966,-16.9999895478102,
71.8008737857751));
#39543=CARTESIAN_POINT('Ctrl Pts',(-3.50471023759971,-16.9999926045357,
71.7999226003202));
#39544=CARTESIAN_POINT('Ctrl Pts',(-3.50379503110591,-16.9999954784432,
71.7990283037671));
#39545=CARTESIAN_POINT('Ctrl Pts',(-3.50302939881839,-16.9999970739683,
71.7982800813199));
#39546=CARTESIAN_POINT('Ctrl Pts',(-3.50239760011444,-16.9999980838367,
71.797662574869));
#39547=CARTESIAN_POINT('Ctrl Pts',(-3.50180873020869,-16.9999990250876,
71.7970870261012));
#39548=CARTESIAN_POINT('Ctrl Pts',(-3.50133627503614,-16.9999994582021,
71.7966251806828));
#39549=CARTESIAN_POINT('Ctrl Pts',(-3.50093597841901,-16.9999997079814,
71.7962338194152));
#39550=CARTESIAN_POINT('Ctrl Pts',(-3.5005869205336,-16.9999999257886,71.7958925531375));
#39551=CARTESIAN_POINT('Ctrl Pts',(-3.50029246039092,-17.,71.7956046177833));
#39552=CARTESIAN_POINT('Ctrl Pts',(-3.5,-17.,71.7953186364093));
#39553=CARTESIAN_POINT('Ctrl Pts',(-3.57453458878625,-16.9981470538884,
71.8682453580158));
#39554=CARTESIAN_POINT('Ctrl Pts',(-3.95884144427023,-16.9790273330526,
72.246439759699));
#39555=CARTESIAN_POINT('Ctrl Pts',(-4.55073801815031,-16.6911512202391,
72.8928385808613));
#39556=CARTESIAN_POINT('Ctrl Pts',(-4.95093404994219,-16.0144112572066,
73.4212646197358));
#39557=CARTESIAN_POINT('Ctrl Pts',(-4.99999999999999,-15.6672482052684,
73.5));
#39558=CARTESIAN_POINT('Ctrl Pts',(-4.99999999999999,-15.5,73.5));
#39559=CARTESIAN_POINT('Ctrl Pts',(-3.33910484519609,-16.9981470538884,
72.1036751016059));
#39560=CARTESIAN_POINT('Ctrl Pts',(-3.72137421607982,-16.9790273330526,
72.4839069878894));
#39561=CARTESIAN_POINT('Ctrl Pts',(-4.33143820572062,-16.6911512202391,
73.1121383932909));
#39562=CARTESIAN_POINT('Ctrl Pts',(-4.77437757320673,-16.0144112572066,
73.5978210964712));
#39563=CARTESIAN_POINT('Ctrl Pts',(-4.83333333333333,-15.6672482052684,
73.6666666666667));
#39564=CARTESIAN_POINT('Ctrl Pts',(-4.83333333333333,-15.5,73.6666666666667));
#39565=CARTESIAN_POINT('Ctrl Pts',(-3.10367510160593,-16.9981470538884,
72.3391048451961));
#39566=CARTESIAN_POINT('Ctrl Pts',(-3.48390698788942,-16.9790273330526,
72.7213742160798));
#39567=CARTESIAN_POINT('Ctrl Pts',(-4.11213839329094,-16.6911512202391,
73.3314382057206));
#39568=CARTESIAN_POINT('Ctrl Pts',(-4.59782109647126,-16.0144112572066,
73.7743775732067));
#39569=CARTESIAN_POINT('Ctrl Pts',(-4.66666666666666,-15.6672482052684,
73.8333333333333));
#39570=CARTESIAN_POINT('Ctrl Pts',(-4.66666666666666,-15.5,73.8333333333333));
#39571=CARTESIAN_POINT('Ctrl Pts',(-2.86824535801578,-16.9981470538884,
72.5745345887862));
#39572=CARTESIAN_POINT('Ctrl Pts',(-3.24643975969902,-16.9790273330526,
72.9588414442702));
#39573=CARTESIAN_POINT('Ctrl Pts',(-3.89283858086125,-16.6911512202391,
73.5507380181503));
#39574=CARTESIAN_POINT('Ctrl Pts',(-4.42126461973579,-16.0144112572066,
73.9509340499422));
#39575=CARTESIAN_POINT('Ctrl Pts',(-4.5,-15.6672482052684,74.));
#39576=CARTESIAN_POINT('Ctrl Pts',(-4.5,-15.5,74.));
#39577=CARTESIAN_POINT('',(-4.99999999999999,-15.5,73.5));
#39578=CARTESIAN_POINT('',(-4.5,-15.5,74.));
#39579=CARTESIAN_POINT('Ctrl Pts',(-4.99999999999999,-15.5,73.5));
#39580=CARTESIAN_POINT('Ctrl Pts',(-4.99999999999999,-15.6672482052684,
73.5));
#39581=CARTESIAN_POINT('Ctrl Pts',(-4.95093404994219,-16.0144112572066,
73.4212646197358));
#39582=CARTESIAN_POINT('Ctrl Pts',(-4.55073801815031,-16.6911512202391,
72.8928385808613));
#39583=CARTESIAN_POINT('Ctrl Pts',(-3.95884144427023,-16.9790273330526,
72.246439759699));
#39584=CARTESIAN_POINT('Ctrl Pts',(-3.57453458878625,-16.9981470538884,
71.8682453580158));
#39585=CARTESIAN_POINT('Origin',(-4.75,-14.,73.75));
#39586=CARTESIAN_POINT('',(-5.,-14.,73.5));
#39587=CARTESIAN_POINT('',(0.749999999999987,-14.,79.2500000000001));
#39588=CARTESIAN_POINT('',(-5.,-14.,73.5));
#39589=CARTESIAN_POINT('Origin',(-3.5,-15.5,68.));
#39590=CARTESIAN_POINT('',(-5.,-15.5,56.2783262011229));
#39591=CARTESIAN_POINT('',(-5.,-15.5,68.));
#39592=CARTESIAN_POINT('Ctrl Pts',(-3.49999999999999,-17.,56.3914887194867));
#39593=CARTESIAN_POINT('Ctrl Pts',(-3.68849285843232,-17.,56.379789702144));
#39594=CARTESIAN_POINT('Ctrl Pts',(-3.88949595769794,-16.9623071985392,
56.366268079425));
#39595=CARTESIAN_POINT('Ctrl Pts',(-4.25923828551908,-16.8090480003591,
56.3395353657988));
#39596=CARTESIAN_POINT('Ctrl Pts',(-4.42798167302478,-16.6934822832211,
56.3263779287031));
#39597=CARTESIAN_POINT('Ctrl Pts',(-4.69412389350913,-16.4270526075957,
56.3048219679644));
#39598=CARTESIAN_POINT('Ctrl Pts',(-4.80941523738749,-16.2585410496607,
56.2949857165266));
#39599=CARTESIAN_POINT('Ctrl Pts',(-4.96235566707568,-15.889189778178,56.2817103328366));
#39600=CARTESIAN_POINT('Ctrl Pts',(-5.,-15.6883461217826,56.2783262011229));
#39601=CARTESIAN_POINT('Ctrl Pts',(-5.,-15.5,56.2783262011229));
#39602=CARTESIAN_POINT('Origin',(-5.,-14.,74.));
#39603=CARTESIAN_POINT('',(-5.,-14.,56.2783262011229));
#39604=CARTESIAN_POINT('',(-4.99999999999999,-14.,82.5));
#39605=CARTESIAN_POINT('',(-5.,-16.45,56.2783262011229));
#39606=CARTESIAN_POINT('Ctrl Pts',(71.8682453580158,-16.9981470538884,-3.57453458878626));
#39607=CARTESIAN_POINT('Ctrl Pts',(71.864163358506,-16.9983534204838,-3.57038661518133));
#39608=CARTESIAN_POINT('Ctrl Pts',(71.834280745957,-16.9997799301677,-3.5399078658621));
#39609=CARTESIAN_POINT('Ctrl Pts',(71.8016132291015,-16.9999870327594,-3.5064297689792));
#39610=CARTESIAN_POINT('Ctrl Pts',(71.7963365978802,-17.,-3.50104102377551));
#39611=CARTESIAN_POINT('Ctrl Pts',(71.7953186364093,-17.,-3.5));
#39612=CARTESIAN_POINT('Ctrl Pts',(72.103675101606,-16.9981470538884,-3.3391048451961));
#39613=CARTESIAN_POINT('Ctrl Pts',(72.0995711107311,-16.9983534204838,-3.33497886295621));
#39614=CARTESIAN_POINT('Ctrl Pts',(72.0694570586096,-16.9997799301677,-3.30473155320941));
#39615=CARTESIAN_POINT('Ctrl Pts',(72.0365616348729,-16.9999870327594,-3.27148136320785));
#39616=CARTESIAN_POINT('Ctrl Pts',(72.0312380731786,-17.,-3.26613954847708));
#39617=CARTESIAN_POINT('Ctrl Pts',(72.0302124242728,-17.,-3.26510621213642));
#39618=CARTESIAN_POINT('Ctrl Pts',(72.3391048451961,-16.9981470538884,-3.10367510160595));
#39619=CARTESIAN_POINT('Ctrl Pts',(72.3349788629562,-16.9983534204838,-3.09957111073108));
#39620=CARTESIAN_POINT('Ctrl Pts',(72.3045547255514,-17.0000242835561,-3.06945705860968));
#39621=CARTESIAN_POINT('Ctrl Pts',(72.2714568031683,-16.9998354184739,-3.03656163487291));
#39622=CARTESIAN_POINT('Ctrl Pts',(72.2661395484771,-17.,-3.03123807317865));
#39623=CARTESIAN_POINT('Ctrl Pts',(72.2651062121364,-17.,-3.03021242427284));
#39624=CARTESIAN_POINT('Ctrl Pts',(72.5745345887863,-16.9981470538884,-2.86824535801579));
#39625=CARTESIAN_POINT('Ctrl Pts',(72.5703866151813,-16.9983534204838,-2.86416335850595));
#39626=CARTESIAN_POINT('Ctrl Pts',(72.5399078658621,-16.9997799301677,-2.83428074595699));
#39627=CARTESIAN_POINT('Ctrl Pts',(72.5064297689792,-16.9999870327594,-2.80161322910156));
#39628=CARTESIAN_POINT('Ctrl Pts',(72.5010410237755,-17.,-2.79633659788022));
#39629=CARTESIAN_POINT('Ctrl Pts',(72.5,-17.,-2.79531863640926));
#39630=CARTESIAN_POINT('',(71.7953186364093,-17.,-3.5));
#39631=CARTESIAN_POINT('',(71.8682453580158,-16.9981470538884,-3.57453458878626));
#39632=CARTESIAN_POINT('Ctrl Pts',(71.7953186364093,-17.,-3.5));
#39633=CARTESIAN_POINT('Ctrl Pts',(71.7956426566413,-17.,-3.50033136103367));
#39634=CARTESIAN_POINT('Ctrl Pts',(71.7959698710105,-16.9999999087783,-3.50066599103948));
#39635=CARTESIAN_POINT('Ctrl Pts',(71.7963728195339,-16.9999996125274,-3.5010781547591));
#39636=CARTESIAN_POINT('Ctrl Pts',(71.7967957210522,-16.9999993016069,-3.50151072778697));
#39637=CARTESIAN_POINT('Ctrl Pts',(71.7973018394014,-16.999998768055,-3.50202849537422));
#39638=CARTESIAN_POINT('Ctrl Pts',(71.7979344421874,-16.9999976134245,-3.50267576544796));
#39639=CARTESIAN_POINT('Ctrl Pts',(71.798608415722,-16.9999963832839,-3.5033653654769));
#39640=CARTESIAN_POINT('Ctrl Pts',(71.7994256794686,-16.9999944448324,-3.50420167541479));
#39641=CARTESIAN_POINT('Ctrl Pts',(71.8003972134396,-16.9999910006556,-3.50519595537292));
#39642=CARTESIAN_POINT('Ctrl Pts',(71.8014697058444,-16.9999871985718,-3.50629355744886));
#39643=CARTESIAN_POINT('Ctrl Pts',(71.8027297908792,-16.9999815341953,-3.50758325228926));
#39644=CARTESIAN_POINT('Ctrl Pts',(71.804148443709,-16.9999727872824,-3.50903534240297));
#39645=CARTESIAN_POINT('Ctrl Pts',(71.8059282949088,-16.9999618133477,-3.51085714423971));
#39646=CARTESIAN_POINT('Ctrl Pts',(71.8079568545965,-16.9999458718544,-3.51293366154225));
#39647=CARTESIAN_POINT('Ctrl Pts',(71.8101187023246,-16.9999235237508,-3.51514671247941));
#39648=CARTESIAN_POINT('Ctrl Pts',(71.8124121613865,-16.9998998151149,-3.51749449195541));
#39649=CARTESIAN_POINT('Ctrl Pts',(71.8148508937686,-16.9998688531822,-3.51999108761023));
#39650=CARTESIAN_POINT('Ctrl Pts',(71.8172869062403,-16.9998314674613,-3.52248486630896));
#39651=CARTESIAN_POINT('Ctrl Pts',(71.8191324991579,-16.9998031429668,-3.52437422457692));
#39652=CARTESIAN_POINT('Ctrl Pts',(71.8209757293308,-16.9997712320714,-3.52626114404862));
#39653=CARTESIAN_POINT('Ctrl Pts',(71.822775757931,-16.9997367040829,-3.52810370841076));
#39654=CARTESIAN_POINT('Ctrl Pts',(71.824400036902,-16.9997055473083,-3.52976637007407));
#39655=CARTESIAN_POINT('Ctrl Pts',(71.8259887368554,-16.9996723091153,-3.53139250445799));
#39656=CARTESIAN_POINT('Ctrl Pts',(71.8275407505538,-16.9996373773349,-3.53298085050784));
#39657=CARTESIAN_POINT('Ctrl Pts',(71.8290718023242,-16.9996029173527,-3.53454774391483));
#39658=CARTESIAN_POINT('Ctrl Pts',(71.8305664957214,-16.9995668629652,-3.53607719242333));
#39659=CARTESIAN_POINT('Ctrl Pts',(71.8320614739058,-16.9995285090951,-3.53760652085725));
#39660=CARTESIAN_POINT('Ctrl Pts',(71.8335194958998,-16.9994911033411,-3.53909804395501));
#39661=CARTESIAN_POINT('Ctrl Pts',(71.8349843334469,-16.9994513364011,-3.54059613558274));
#39662=CARTESIAN_POINT('Ctrl Pts',(71.8364852326096,-16.9994082206029,-3.54213060631543));
#39663=CARTESIAN_POINT('Ctrl Pts',(71.8380984008872,-16.9993618796896,-3.543779857358));
#39664=CARTESIAN_POINT('Ctrl Pts',(71.8397528770163,-16.9993116397098,-3.54547077478768));
#39665=CARTESIAN_POINT('Ctrl Pts',(71.8414428847978,-16.9992572833264,-3.54719744053074));
#39666=CARTESIAN_POINT('Ctrl Pts',(71.8433735916158,-16.9991951852455,-3.54917002631353));
#39667=CARTESIAN_POINT('Ctrl Pts',(71.8453501484938,-16.9991276636876,-3.55118873161033));
#39668=CARTESIAN_POINT('Ctrl Pts',(71.8473171286807,-16.9990563957717,-3.55319701397667));
#39669=CARTESIAN_POINT('Ctrl Pts',(71.8500422837313,-16.9989576575525,-3.55597939118101));
#39670=CARTESIAN_POINT('Ctrl Pts',(71.8527461713318,-16.9988515979041,-3.5587388045199));
#39671=CARTESIAN_POINT('Ctrl Pts',(71.8552161386877,-16.9987486082515,-3.56125854441687));
#39672=CARTESIAN_POINT('Ctrl Pts',(71.8570686142046,-16.9986713660121,-3.56314834933959));
#39673=CARTESIAN_POINT('Ctrl Pts',(71.8587868623066,-16.998596102758,-3.56490064570692));
#39674=CARTESIAN_POINT('Ctrl Pts',(71.8602963585415,-16.9985278711001,-3.56643959313724));
#39675=CARTESIAN_POINT('Ctrl Pts',(71.8615610437189,-16.9984707052957,-3.5677289530965));
#39676=CARTESIAN_POINT('Ctrl Pts',(71.8626788313975,-16.9984185388897,-3.56886818435398));
#39677=CARTESIAN_POINT('Ctrl Pts',(71.8636316653216,-16.998373289921,-3.56983898661491));
#39678=CARTESIAN_POINT('Ctrl Pts',(71.8645275000202,-16.9983307477788,-3.57075171477112));
#39679=CARTESIAN_POINT('Ctrl Pts',(71.8652771155594,-16.9982943574932,-3.57151514502298));
#39680=CARTESIAN_POINT('Ctrl Pts',(71.8658958651526,-16.9982640274543,-3.5721450208714));
#39681=CARTESIAN_POINT('Ctrl Pts',(71.8664725654875,-16.9982357585976,-3.5727320913385));
#39682=CARTESIAN_POINT('Ctrl Pts',(71.8669354348749,-16.9982127623775,-3.57320299278075));
#39683=CARTESIAN_POINT('Ctrl Pts',(71.867327729259,-16.9981931657129,-3.57360188999627));
#39684=CARTESIAN_POINT('Ctrl Pts',(71.8676698713729,-16.9981760743537,-3.57394979081276));
#39685=CARTESIAN_POINT('Ctrl Pts',(71.8679585937126,-16.9981615513357,-3.57424318974083));
#39686=CARTESIAN_POINT('Ctrl Pts',(71.8682453580158,-16.9981470538884,-3.57453458878626));
#39687=CARTESIAN_POINT('',(72.5745345887863,-16.9981470538884,-2.86824535801579));
#39688=CARTESIAN_POINT('Ctrl Pts',(72.5745345887863,-16.9981470538884,-2.86824535801579));
#39689=CARTESIAN_POINT('Ctrl Pts',(72.3391048451961,-16.9981470538884,-3.10367510160595));
#39690=CARTESIAN_POINT('Ctrl Pts',(72.103675101606,-16.9981470538884,-3.3391048451961));
#39691=CARTESIAN_POINT('Ctrl Pts',(71.8682453580158,-16.9981470538884,-3.57453458878626));
#39692=CARTESIAN_POINT('',(72.5,-17.,-2.79531863640926));
#39693=CARTESIAN_POINT('Ctrl Pts',(72.5745345887863,-16.9981470538884,-2.86824535801579));
#39694=CARTESIAN_POINT('Ctrl Pts',(72.5742044925281,-16.9981634765679,-2.86792051198431));
#39695=CARTESIAN_POINT('Ctrl Pts',(72.5738711310018,-16.9981799708645,-2.86759246756107));
#39696=CARTESIAN_POINT('Ctrl Pts',(72.5734604128101,-16.9982001093812,-2.86718860352498));
#39697=CARTESIAN_POINT('Ctrl Pts',(72.57302935509,-16.9982212451946,-2.86676473939109));
#39698=CARTESIAN_POINT('Ctrl Pts',(72.572513296839,-16.9982463879926,-2.86625756382415));
#39699=CARTESIAN_POINT('Ctrl Pts',(72.5718680115172,-16.9982773404549,-2.86562376912052));
#39700=CARTESIAN_POINT('Ctrl Pts',(72.5711805211291,-16.9983103173716,-2.86494852089771));
#39701=CARTESIAN_POINT('Ctrl Pts',(72.5703466306137,-16.9983498713227,-2.86412982782487));
#39702=CARTESIAN_POINT('Ctrl Pts',(72.5693550535868,-16.9983957676602,-2.86315671761943));
#39703=CARTESIAN_POINT('Ctrl Pts',(72.5682604104266,-16.9984464345378,-2.8620824607523));
#39704=CARTESIAN_POINT('Ctrl Pts',(72.5669740091159,-16.9985047829815,-2.86082042406594));
#39705=CARTESIAN_POINT('Ctrl Pts',(72.565525387959,-16.9985681244217,-2.85939970674285));
#39706=CARTESIAN_POINT('Ctrl Pts',(72.5637077270911,-16.9986476022457,-2.8576170582772));
#39707=CARTESIAN_POINT('Ctrl Pts',(72.5616355608823,-16.9987347812318,-2.85558546640713));
#39708=CARTESIAN_POINT('Ctrl Pts',(72.5594266767905,-16.9988223610841,-2.85342062894714));
#39709=CARTESIAN_POINT('Ctrl Pts',(72.5570842219804,-16.9989152368701,-2.85112488425853));
#39710=CARTESIAN_POINT('Ctrl Pts',(72.5545928471898,-16.9990082804756,-2.8486840335237));
#39711=CARTESIAN_POINT('Ctrl Pts',(72.552103587594,-16.9990947989236,-2.84624625175195));
#39712=CARTESIAN_POINT('Ctrl Pts',(72.5502173068831,-16.9991603598156,-2.84439897927724));
#39713=CARTESIAN_POINT('Ctrl Pts',(72.5483330647398,-16.9992222334679,-2.84255427195848));
#39714=CARTESIAN_POINT('Ctrl Pts',(72.5464926261216,-16.9992793054386,-2.84075306394266));
#39715=CARTESIAN_POINT('Ctrl Pts',(72.5448318572274,-16.9993308058541,-2.83912769582928));
#39716=CARTESIAN_POINT('Ctrl Pts',(72.543207168852,-16.9993784253393,-2.83753815081149));
#39717=CARTESIAN_POINT('Ctrl Pts',(72.5416197584348,-16.9994224873957,-2.83598557864455));
#39718=CARTESIAN_POINT('Ctrl Pts',(72.540053319257,-16.9994659673493,-2.83445351746977));
#39719=CARTESIAN_POINT('Ctrl Pts',(72.5385238533706,-16.9995060035546,-2.83295811821705));
#39720=CARTESIAN_POINT('Ctrl Pts',(72.5369939676884,-16.9995437460623,-2.83146270058428));
#39721=CARTESIAN_POINT('Ctrl Pts',(72.5355023760137,-16.9995805438512,-2.83000471420189));
#39722=CARTESIAN_POINT('Ctrl Pts',(72.5340037037557,-16.9996153196962,-2.82854016663104));
#39723=CARTESIAN_POINT('Ctrl Pts',(72.5324681805947,-16.9996485645807,-2.82703981578639));
#39724=CARTESIAN_POINT('Ctrl Pts',(72.5308177719951,-16.9996842967954,-2.82542721104074));
#39725=CARTESIAN_POINT('Ctrl Pts',(72.529125149268,-16.9997182120423,-2.82377359513262));
#39726=CARTESIAN_POINT('Ctrl Pts',(72.5273963190708,-16.9997497930326,-2.82208470500297));
#39727=CARTESIAN_POINT('Ctrl Pts',(72.5254211385424,-16.9997858741684,-2.8201551558175));
#39728=CARTESIAN_POINT('Ctrl Pts',(72.5233992312896,-16.9998188305302,-2.81818008615894));
#39729=CARTESIAN_POINT('Ctrl Pts',(72.52138736276,-16.9998475191546,-2.81621482751819));
#39730=CARTESIAN_POINT('Ctrl Pts',(72.5186005402079,-16.9998872583841,-2.81349256857325));
#39731=CARTESIAN_POINT('Ctrl Pts',(72.5158359360068,-16.9999185308537,-2.81079201806525));
#39732=CARTESIAN_POINT('Ctrl Pts',(72.5133109478137,-16.9999409383933,-2.8083253911404));
#39733=CARTESIAN_POINT('Ctrl Pts',(72.5114172066689,-16.9999577440481,-2.80647542094677));
#39734=CARTESIAN_POINT('Ctrl Pts',(72.5096609508553,-16.9999696816405,-2.80475967567116));
#39735=CARTESIAN_POINT('Ctrl Pts',(72.508118309431,-16.9999780308564,-2.803252515256));
#39736=CARTESIAN_POINT('Ctrl Pts',(72.5068258239489,-16.999985026157,-2.80198975715482));
#39737=CARTESIAN_POINT('Ctrl Pts',(72.5056836631397,-16.9999895478102,-2.80087378577512));
#39738=CARTESIAN_POINT('Ctrl Pts',(72.5047102375997,-16.9999926045357,-2.79992260032024));
#39739=CARTESIAN_POINT('Ctrl Pts',(72.5037950311059,-16.9999954784432,-2.79902830376709));
#39740=CARTESIAN_POINT('Ctrl Pts',(72.5030293988184,-16.9999970739683,-2.79828008131994));
#39741=CARTESIAN_POINT('Ctrl Pts',(72.5023976001144,-16.9999980838367,-2.79766257486899));
#39742=CARTESIAN_POINT('Ctrl Pts',(72.5018087302087,-16.9999990250876,-2.79708702610116));
#39743=CARTESIAN_POINT('Ctrl Pts',(72.5013362750362,-16.9999994582021,-2.79662518068281));
#39744=CARTESIAN_POINT('Ctrl Pts',(72.500935978419,-16.9999997079814,-2.79623381941522));
#39745=CARTESIAN_POINT('Ctrl Pts',(72.5005869205336,-16.9999999257886,-2.79589255313753));
#39746=CARTESIAN_POINT('Ctrl Pts',(72.5002924603909,-17.,-2.79560461778332));
#39747=CARTESIAN_POINT('Ctrl Pts',(72.5,-17.,-2.79531863640926));
#39748=CARTESIAN_POINT('',(72.1476593182046,-17.,-3.14765931820463));
#39749=CARTESIAN_POINT('Ctrl Pts',(72.5745345887863,-16.9981470538884,-2.86824535801579));
#39750=CARTESIAN_POINT('Ctrl Pts',(72.8307391591089,-16.9854005733312,-3.12037495913795));
#39751=CARTESIAN_POINT('Ctrl Pts',(73.3201733549766,-16.8268077199093,-3.63377877163944));
#39752=CARTESIAN_POINT('Ctrl Pts',(73.7358067305414,-16.3991227020429,-4.13541628736354));
#39753=CARTESIAN_POINT('Ctrl Pts',(73.9615602058987,-15.9274342791999,-4.43902863521564));
#39754=CARTESIAN_POINT('Ctrl Pts',(74.,-15.6672482052684,-4.5));
#39755=CARTESIAN_POINT('Ctrl Pts',(74.,-15.5,-4.5));
#39756=CARTESIAN_POINT('Ctrl Pts',(72.3391048451961,-16.9981470538884,-3.10367510160595));
#39757=CARTESIAN_POINT('Ctrl Pts',(72.5939510924519,-16.9854005733312,-3.35716302579494));
#39758=CARTESIAN_POINT('Ctrl Pts',(73.0913751605309,-16.8268077199093,-3.86257696608515));
#39759=CARTESIAN_POINT('Ctrl Pts',(73.5356765828155,-16.3991227020429,-4.3355464350895));
#39760=CARTESIAN_POINT('Ctrl Pts',(73.7873830156711,-15.9274342791999,-4.61320582544333));
#39761=CARTESIAN_POINT('Ctrl Pts',(73.8333333333333,-15.6672482052684,-4.66666666666667));
#39762=CARTESIAN_POINT('Ctrl Pts',(73.8333333333333,-15.5,-4.66666666666667));
#39763=CARTESIAN_POINT('Ctrl Pts',(72.103675101606,-16.9981470538884,-3.3391048451961));
#39764=CARTESIAN_POINT('Ctrl Pts',(72.3571630257949,-16.9854005733312,-3.59395109245193));
#39765=CARTESIAN_POINT('Ctrl Pts',(72.8625769660852,-16.8268077199093,-4.09137516053087));
#39766=CARTESIAN_POINT('Ctrl Pts',(73.3355464350895,-16.3991227020429,-4.53567658281546));
#39767=CARTESIAN_POINT('Ctrl Pts',(73.6132058254434,-15.9274342791999,-4.78738301567102));
#39768=CARTESIAN_POINT('Ctrl Pts',(73.6666666666667,-15.6672482052684,-4.83333333333333));
#39769=CARTESIAN_POINT('Ctrl Pts',(73.6666666666667,-15.5,-4.83333333333333));
#39770=CARTESIAN_POINT('Ctrl Pts',(71.8682453580158,-16.9981470538884,-3.57453458878626));
#39771=CARTESIAN_POINT('Ctrl Pts',(72.120374959138,-16.9854005733312,-3.83073915910891));
#39772=CARTESIAN_POINT('Ctrl Pts',(72.6337787716395,-16.8268077199093,-4.32017335497659));
#39773=CARTESIAN_POINT('Ctrl Pts',(73.1354162873635,-16.3991227020429,-4.73580673054142));
#39774=CARTESIAN_POINT('Ctrl Pts',(73.4390286352157,-15.9274342791999,-4.9615602058987));
#39775=CARTESIAN_POINT('Ctrl Pts',(73.5,-15.6672482052684,-5.));
#39776=CARTESIAN_POINT('Ctrl Pts',(73.5,-15.5,-5.));
#39777=CARTESIAN_POINT('',(73.5,-15.5,-5.));
#39778=CARTESIAN_POINT('Ctrl Pts',(71.8682453580158,-16.9981470538884,-3.57453458878626));
#39779=CARTESIAN_POINT('Ctrl Pts',(72.120374959138,-16.9854005733312,-3.83073915910891));
#39780=CARTESIAN_POINT('Ctrl Pts',(72.6337787716395,-16.8268077199093,-4.32017335497659));
#39781=CARTESIAN_POINT('Ctrl Pts',(73.1354162873635,-16.3991227020429,-4.73580673054142));
#39782=CARTESIAN_POINT('Ctrl Pts',(73.4390286352157,-15.9274342791999,-4.9615602058987));
#39783=CARTESIAN_POINT('Ctrl Pts',(73.5,-15.6672482052684,-5.));
#39784=CARTESIAN_POINT('Ctrl Pts',(73.5,-15.5,-5.));
#39785=CARTESIAN_POINT('',(74.,-15.5,-4.5));
#39786=CARTESIAN_POINT('',(73.5,-15.5,-5.));
#39787=CARTESIAN_POINT('Ctrl Pts',(74.,-15.5,-4.5));
#39788=CARTESIAN_POINT('Ctrl Pts',(74.,-15.6672482052684,-4.5));
#39789=CARTESIAN_POINT('Ctrl Pts',(73.9615602058987,-15.9274342791999,-4.43902863521564));
#39790=CARTESIAN_POINT('Ctrl Pts',(73.7358067305414,-16.3991227020429,-4.13541628736354));
#39791=CARTESIAN_POINT('Ctrl Pts',(73.3201733549766,-16.8268077199093,-3.63377877163944));
#39792=CARTESIAN_POINT('Ctrl Pts',(72.8307391591089,-16.9854005733312,-3.12037495913795));
#39793=CARTESIAN_POINT('Ctrl Pts',(72.5745345887863,-16.9981470538884,-2.86824535801579));
#39794=CARTESIAN_POINT('Origin',(73.75,-14.,-4.75));
#39795=CARTESIAN_POINT('',(73.5,-14.,-5.));
#39796=CARTESIAN_POINT('',(74.,-14.,-4.5));
#39797=CARTESIAN_POINT('',(79.2500000000001,-14.,0.750000000000108));
#39798=CARTESIAN_POINT('',(74.,-14.,-4.5));
#39799=CARTESIAN_POINT('',(73.5,-14.,-5.));
#39800=CARTESIAN_POINT('Origin',(62.,-17.,0.));
#39801=CARTESIAN_POINT('',(72.5,-17.,2.79531863640926));
#39802=CARTESIAN_POINT('',(72.5,-17.,-2.5));
#39803=CARTESIAN_POINT('',(71.7953186364093,-17.,3.5));
#39804=CARTESIAN_POINT('',(72.1476593182046,-17.,3.14765931820463));
#39805=CARTESIAN_POINT('',(56.3914887194867,-17.,3.5));
#39806=CARTESIAN_POINT('',(68.,-17.,3.5));
#39807=CARTESIAN_POINT('',(56.3914887194867,-17.,-3.5));
#39808=CARTESIAN_POINT('Origin',(0.,-17.,0.));
#39809=CARTESIAN_POINT('',(56.,-17.,-3.5));
#39810=CARTESIAN_POINT('Origin',(72.5,-15.5,-2.5));
#39811=CARTESIAN_POINT('',(74.,-15.5,4.5));
#39812=CARTESIAN_POINT('',(74.,-15.5,-2.5));
#39813=CARTESIAN_POINT('',(72.5745345887863,-16.9981470538884,2.86824535801578));
#39814=CARTESIAN_POINT('Ctrl Pts',(72.5745345887863,-16.9981470538884,2.86824535801578));
#39815=CARTESIAN_POINT('Ctrl Pts',(72.8307391591089,-16.9854005733312,3.12037495913794));
#39816=CARTESIAN_POINT('Ctrl Pts',(73.3201733549766,-16.8268077199093,3.63377877163943));
#39817=CARTESIAN_POINT('Ctrl Pts',(73.7358067305414,-16.3991227020429,4.13541628736354));
#39818=CARTESIAN_POINT('Ctrl Pts',(73.9615602058987,-15.9274342791999,4.43902863521564));
#39819=CARTESIAN_POINT('Ctrl Pts',(74.,-15.6672482052684,4.5));
#39820=CARTESIAN_POINT('Ctrl Pts',(74.,-15.5,4.5));
#39821=CARTESIAN_POINT('Ctrl Pts',(72.5,-17.,2.79531863640926));
#39822=CARTESIAN_POINT('Ctrl Pts',(72.5003313610337,-17.,2.79564265664126));
#39823=CARTESIAN_POINT('Ctrl Pts',(72.5006659910395,-16.9999999087783,2.79596987101049));
#39824=CARTESIAN_POINT('Ctrl Pts',(72.5010781547591,-16.9999996125274,2.79637281953386));
#39825=CARTESIAN_POINT('Ctrl Pts',(72.501510727787,-16.9999993016069,2.79679572105221));
#39826=CARTESIAN_POINT('Ctrl Pts',(72.5020284953742,-16.999998768055,2.79730183940144));
#39827=CARTESIAN_POINT('Ctrl Pts',(72.502675765448,-16.9999976134245,2.79793444218739));
#39828=CARTESIAN_POINT('Ctrl Pts',(72.5033653654769,-16.9999963832839,2.79860841572208));
#39829=CARTESIAN_POINT('Ctrl Pts',(72.5042016754148,-16.9999944448324,2.79942567946861));
#39830=CARTESIAN_POINT('Ctrl Pts',(72.5051959553729,-16.9999910006556,2.80039721343955));
#39831=CARTESIAN_POINT('Ctrl Pts',(72.5062935574489,-16.9999871985718,2.80146970584437));
#39832=CARTESIAN_POINT('Ctrl Pts',(72.5075832522893,-16.9999815341953,2.80272979087918));
#39833=CARTESIAN_POINT('Ctrl Pts',(72.509035342403,-16.9999727872824,2.80414844370901));
#39834=CARTESIAN_POINT('Ctrl Pts',(72.5108571442397,-16.9999618133477,2.80592829490876));
#39835=CARTESIAN_POINT('Ctrl Pts',(72.5129336615422,-16.9999458718544,2.80795685459655));
#39836=CARTESIAN_POINT('Ctrl Pts',(72.5151467124794,-16.9999235237508,2.81011870232459));
#39837=CARTESIAN_POINT('Ctrl Pts',(72.5174944919554,-16.9998998151149,2.81241216138644));
#39838=CARTESIAN_POINT('Ctrl Pts',(72.5199910876102,-16.9998688531822,2.81485089376853));
#39839=CARTESIAN_POINT('Ctrl Pts',(72.5224848663089,-16.9998314674613,2.81728690624033));
#39840=CARTESIAN_POINT('Ctrl Pts',(72.5243742245769,-16.9998031429668,2.81913249915794));
#39841=CARTESIAN_POINT('Ctrl Pts',(72.5262611440486,-16.9997712320714,2.82097572933083));
#39842=CARTESIAN_POINT('Ctrl Pts',(72.5281037084107,-16.9997367040829,2.82277575793095));
#39843=CARTESIAN_POINT('Ctrl Pts',(72.529766370074,-16.9997055473083,2.824400036902));
#39844=CARTESIAN_POINT('Ctrl Pts',(72.5313925044579,-16.9996723091153,2.82598873685535));
#39845=CARTESIAN_POINT('Ctrl Pts',(72.5329808505078,-16.9996373773349,2.82754075055375));
#39846=CARTESIAN_POINT('Ctrl Pts',(72.5345477439147,-16.9996029173527,2.82907180232405));
#39847=CARTESIAN_POINT('Ctrl Pts',(72.5360771924231,-16.9995668629652,2.83056649572116));
#39848=CARTESIAN_POINT('Ctrl Pts',(72.5376065208569,-16.9995285090951,2.83206147390553));
#39849=CARTESIAN_POINT('Ctrl Pts',(72.5390980439547,-16.9994911033411,2.83351949589957));
#39850=CARTESIAN_POINT('Ctrl Pts',(72.5405961355824,-16.9994513364011,2.83498433344659));
#39851=CARTESIAN_POINT('Ctrl Pts',(72.5421306063151,-16.9994082206029,2.8364852326093));
#39852=CARTESIAN_POINT('Ctrl Pts',(72.5437798573576,-16.9993618796896,2.83809840088688));
#39853=CARTESIAN_POINT('Ctrl Pts',(72.5454707747873,-16.9993116397099,2.83975287701592));
#39854=CARTESIAN_POINT('Ctrl Pts',(72.5471974405303,-16.9992572833264,2.84144288479735));
#39855=CARTESIAN_POINT('Ctrl Pts',(72.549170026313,-16.9991951852455,2.84337359161536));
#39856=CARTESIAN_POINT('Ctrl Pts',(72.5511887316098,-16.9991276636876,2.84535014849327));
#39857=CARTESIAN_POINT('Ctrl Pts',(72.5531970139762,-16.9990563957717,2.84731712868022));
#39858=CARTESIAN_POINT('Ctrl Pts',(72.5559793911805,-16.9989576575525,2.85004228373082));
#39859=CARTESIAN_POINT('Ctrl Pts',(72.5587388045195,-16.9988515979041,2.85274617133141));
#39860=CARTESIAN_POINT('Ctrl Pts',(72.5612585444165,-16.9987486082516,2.85521613868735));
#39861=CARTESIAN_POINT('Ctrl Pts',(72.5631483493393,-16.9986713660122,2.8570686142043));
#39862=CARTESIAN_POINT('Ctrl Pts',(72.5649006457067,-16.998596102758,2.8587868623063));
#39863=CARTESIAN_POINT('Ctrl Pts',(72.566439593137,-16.9985278711001,2.86029635854127));
#39864=CARTESIAN_POINT('Ctrl Pts',(72.5677289530963,-16.9984707052957,2.86156104371873));
#39865=CARTESIAN_POINT('Ctrl Pts',(72.5688681843538,-16.9984185388897,2.86267883139733));
#39866=CARTESIAN_POINT('Ctrl Pts',(72.5698389866148,-16.998373289921,2.8636316653215));
#39867=CARTESIAN_POINT('Ctrl Pts',(72.570751714771,-16.9983307477788,2.86452750002005));
#39868=CARTESIAN_POINT('Ctrl Pts',(72.5715151450229,-16.9982943574932,2.86527711555929));
#39869=CARTESIAN_POINT('Ctrl Pts',(72.5721450208713,-16.9982640274543,2.86589586515251));
#39870=CARTESIAN_POINT('Ctrl Pts',(72.5727320913384,-16.9982357585976,2.86647256548738));
#39871=CARTESIAN_POINT('Ctrl Pts',(72.5732029927807,-16.9982127623775,2.86693543487483));
#39872=CARTESIAN_POINT('Ctrl Pts',(72.5736018899962,-16.9981931657129,2.86732772925895));
#39873=CARTESIAN_POINT('Ctrl Pts',(72.5739497908127,-16.9981760743537,2.86766987137284));
#39874=CARTESIAN_POINT('Ctrl Pts',(72.5742431897408,-16.9981615513357,2.86795859371254));
#39875=CARTESIAN_POINT('Ctrl Pts',(72.5745345887863,-16.9981470538884,2.86824535801578));
#39876=CARTESIAN_POINT('Origin',(74.,-14.,-5.));
#39877=CARTESIAN_POINT('',(74.,-14.,4.5));
#39878=CARTESIAN_POINT('',(74.,-14.,43.));
#39879=CARTESIAN_POINT('',(74.,-14.,4.5));
#39880=CARTESIAN_POINT('Ctrl Pts',(72.5745345887863,-16.9981470538884,2.86824535801578));
#39881=CARTESIAN_POINT('Ctrl Pts',(72.5703866151813,-16.9983534204838,2.86416335850594));
#39882=CARTESIAN_POINT('Ctrl Pts',(72.5399078658621,-16.9997799301677,2.83428074595701));
#39883=CARTESIAN_POINT('Ctrl Pts',(72.5064297689792,-16.9999870327594,2.80161322910156));
#39884=CARTESIAN_POINT('Ctrl Pts',(72.5010410237755,-17.,2.79633659788022));
#39885=CARTESIAN_POINT('Ctrl Pts',(72.5,-17.,2.79531863640926));
#39886=CARTESIAN_POINT('Ctrl Pts',(72.3391048451961,-16.9981470538884,3.10367510160594));
#39887=CARTESIAN_POINT('Ctrl Pts',(72.3349788629562,-16.9983534204838,3.09957111073107));
#39888=CARTESIAN_POINT('Ctrl Pts',(72.3047315532094,-16.9997799301677,3.06945705860969));
#39889=CARTESIAN_POINT('Ctrl Pts',(72.2714813632079,-16.9999870327594,3.03656163487291));
#39890=CARTESIAN_POINT('Ctrl Pts',(72.2661395484771,-17.,3.03123807317865));
#39891=CARTESIAN_POINT('Ctrl Pts',(72.2651062121364,-17.,3.03021242427284));
#39892=CARTESIAN_POINT('Ctrl Pts',(72.1036751016059,-16.9981470538884,3.3391048451961));
#39893=CARTESIAN_POINT('Ctrl Pts',(72.0995711107311,-16.9983534204838,3.3349788629562));
#39894=CARTESIAN_POINT('Ctrl Pts',(72.0694570586097,-17.0000242835561,3.30455472555144));
#39895=CARTESIAN_POINT('Ctrl Pts',(72.0365616348729,-16.9998354184739,3.27145680316828));
#39896=CARTESIAN_POINT('Ctrl Pts',(72.0312380731786,-17.,3.26613954847708));
#39897=CARTESIAN_POINT('Ctrl Pts',(72.0302124242728,-17.,3.26510621213642));
#39898=CARTESIAN_POINT('Ctrl Pts',(71.8682453580158,-16.9981470538884,3.57453458878625));
#39899=CARTESIAN_POINT('Ctrl Pts',(71.8641633585059,-16.9983534204838,3.57038661518133));
#39900=CARTESIAN_POINT('Ctrl Pts',(71.834280745957,-16.9997799301677,3.53990786586208));
#39901=CARTESIAN_POINT('Ctrl Pts',(71.8016132291015,-16.9999870327594,3.50642976897919));
#39902=CARTESIAN_POINT('Ctrl Pts',(71.7963365978802,-17.,3.50104102377551));
#39903=CARTESIAN_POINT('Ctrl Pts',(71.7953186364093,-17.,3.5));
#39904=CARTESIAN_POINT('',(71.8682453580158,-16.9981470538884,3.57453458878625));
#39905=CARTESIAN_POINT('Ctrl Pts',(71.8682453580158,-16.9981470538884,3.57453458878625));
#39906=CARTESIAN_POINT('Ctrl Pts',(72.1036751016059,-16.9981470538884,3.3391048451961));
#39907=CARTESIAN_POINT('Ctrl Pts',(72.3391048451961,-16.9981470538884,3.10367510160594));
#39908=CARTESIAN_POINT('Ctrl Pts',(72.5745345887863,-16.9981470538884,2.86824535801578));
#39909=CARTESIAN_POINT('Ctrl Pts',(71.8682453580158,-16.9981470538884,3.57453458878625));
#39910=CARTESIAN_POINT('Ctrl Pts',(71.8679205119843,-16.9981634765679,3.57420449252804));
#39911=CARTESIAN_POINT('Ctrl Pts',(71.8675924675611,-16.9981799708645,3.57387113100175));
#39912=CARTESIAN_POINT('Ctrl Pts',(71.867188603525,-16.9982001093812,3.57346041281004));
#39913=CARTESIAN_POINT('Ctrl Pts',(71.8667647393911,-16.9982212451946,3.57302935509001));
#39914=CARTESIAN_POINT('Ctrl Pts',(71.8662575638241,-16.9982463879926,3.57251329683895));
#39915=CARTESIAN_POINT('Ctrl Pts',(71.8656237691205,-16.9982773404549,3.57186801151715));
#39916=CARTESIAN_POINT('Ctrl Pts',(71.8649485208977,-16.9983103173716,3.57118052112908));
#39917=CARTESIAN_POINT('Ctrl Pts',(71.8641298278249,-16.9983498713227,3.57034663061371));
#39918=CARTESIAN_POINT('Ctrl Pts',(71.8631567176194,-16.9983957676602,3.56935505358678));
#39919=CARTESIAN_POINT('Ctrl Pts',(71.8620824607523,-16.9984464345378,3.56826041042662));
#39920=CARTESIAN_POINT('Ctrl Pts',(71.8608204240659,-16.9985047829815,3.56697400911588));
#39921=CARTESIAN_POINT('Ctrl Pts',(71.8593997067429,-16.9985681244217,3.56552538795904));
#39922=CARTESIAN_POINT('Ctrl Pts',(71.8576170582772,-16.9986476022456,3.56370772709111));
#39923=CARTESIAN_POINT('Ctrl Pts',(71.8555854664071,-16.9987347812318,3.5616355608823));
#39924=CARTESIAN_POINT('Ctrl Pts',(71.8534206289472,-16.9988223610841,3.55942667679056));
#39925=CARTESIAN_POINT('Ctrl Pts',(71.8511248842585,-16.9989152368701,3.55708422198038));
#39926=CARTESIAN_POINT('Ctrl Pts',(71.8486840335237,-16.9990082804756,3.55459284718975));
#39927=CARTESIAN_POINT('Ctrl Pts',(71.8462462517519,-16.9990947989236,3.55210358759403));
#39928=CARTESIAN_POINT('Ctrl Pts',(71.8443989792772,-16.9991603598156,3.55021730688309));
#39929=CARTESIAN_POINT('Ctrl Pts',(71.8425542719585,-16.9992222334679,3.54833306473982));
#39930=CARTESIAN_POINT('Ctrl Pts',(71.8407530639426,-16.9992793054386,3.54649262612162));
#39931=CARTESIAN_POINT('Ctrl Pts',(71.8391276958293,-16.9993308058541,3.54483185722743));
#39932=CARTESIAN_POINT('Ctrl Pts',(71.8375381508115,-16.9993784253393,3.543207168852));
#39933=CARTESIAN_POINT('Ctrl Pts',(71.8359855786445,-16.9994224873957,3.54161975843481));
#39934=CARTESIAN_POINT('Ctrl Pts',(71.8344535174697,-16.9994659673493,3.54005331925702));
#39935=CARTESIAN_POINT('Ctrl Pts',(71.832958118217,-16.9995060035546,3.53852385337056));
#39936=CARTESIAN_POINT('Ctrl Pts',(71.8314627005842,-16.9995437460623,3.53699396768834));
#39937=CARTESIAN_POINT('Ctrl Pts',(71.8300047142018,-16.9995805438512,3.53550237601363));
#39938=CARTESIAN_POINT('Ctrl Pts',(71.828540166631,-16.9996153196962,3.53400370375568));
#39939=CARTESIAN_POINT('Ctrl Pts',(71.8270398157863,-16.9996485645807,3.53246818059467));
#39940=CARTESIAN_POINT('Ctrl Pts',(71.8254272110407,-16.9996842967954,3.53081777199503));
#39941=CARTESIAN_POINT('Ctrl Pts',(71.8237735951326,-16.9997182120423,3.52912514926797));
#39942=CARTESIAN_POINT('Ctrl Pts',(71.8220847050029,-16.9997497930326,3.52739631907077));
#39943=CARTESIAN_POINT('Ctrl Pts',(71.8201551558174,-16.9997858741684,3.52542113854231));
#39944=CARTESIAN_POINT('Ctrl Pts',(71.8181800861589,-16.9998188305302,3.52339923128955));
#39945=CARTESIAN_POINT('Ctrl Pts',(71.8162148275181,-16.9998475191546,3.52138736275992));
#39946=CARTESIAN_POINT('Ctrl Pts',(71.8134925685732,-16.9998872583841,3.51860054020779));
#39947=CARTESIAN_POINT('Ctrl Pts',(71.8107920180652,-16.9999185308537,3.51583593600674));
#39948=CARTESIAN_POINT('Ctrl Pts',(71.8083253911404,-16.9999409383933,3.51331094781366));
#39949=CARTESIAN_POINT('Ctrl Pts',(71.8064754209467,-16.9999577440481,3.51141720666885));
#39950=CARTESIAN_POINT('Ctrl Pts',(71.8047596756711,-16.9999696816405,3.50966095085529));
#39951=CARTESIAN_POINT('Ctrl Pts',(71.803252515256,-16.9999780308564,3.50811830943094));
#39952=CARTESIAN_POINT('Ctrl Pts',(71.8019897571548,-16.999985026157,3.50682582394882));
#39953=CARTESIAN_POINT('Ctrl Pts',(71.8008737857751,-16.9999895478102,3.50568366313965));
#39954=CARTESIAN_POINT('Ctrl Pts',(71.7999226003202,-16.9999926045357,3.50471023759971));
#39955=CARTESIAN_POINT('Ctrl Pts',(71.7990283037671,-16.9999954784432,3.50379503110591));
#39956=CARTESIAN_POINT('Ctrl Pts',(71.7982800813199,-16.9999970739683,3.50302939881839));
#39957=CARTESIAN_POINT('Ctrl Pts',(71.797662574869,-16.9999980838367,3.50239760011444));
#39958=CARTESIAN_POINT('Ctrl Pts',(71.7970870261012,-16.9999990250876,3.50180873020869));
#39959=CARTESIAN_POINT('Ctrl Pts',(71.7966251806828,-16.9999994582021,3.50133627503614));
#39960=CARTESIAN_POINT('Ctrl Pts',(71.7962338194152,-16.9999997079814,3.50093597841902));
#39961=CARTESIAN_POINT('Ctrl Pts',(71.7958925531375,-16.9999999257886,3.5005869205336));
#39962=CARTESIAN_POINT('Ctrl Pts',(71.7956046177833,-17.,3.50029246039093));
#39963=CARTESIAN_POINT('Ctrl Pts',(71.7953186364093,-17.,3.5));
#39964=CARTESIAN_POINT('Ctrl Pts',(71.8682453580158,-16.9981470538884,3.57453458878625));
#39965=CARTESIAN_POINT('Ctrl Pts',(72.1203749591379,-16.9854005733312,3.83073915910891));
#39966=CARTESIAN_POINT('Ctrl Pts',(72.6337787716394,-16.8268077199093,4.32017335497658));
#39967=CARTESIAN_POINT('Ctrl Pts',(73.1354162873635,-16.3991227020429,4.73580673054142));
#39968=CARTESIAN_POINT('Ctrl Pts',(73.4390286352156,-15.9274342791999,4.9615602058987));
#39969=CARTESIAN_POINT('Ctrl Pts',(73.5,-15.6672482052684,5.));
#39970=CARTESIAN_POINT('Ctrl Pts',(73.5,-15.5,5.));
#39971=CARTESIAN_POINT('Ctrl Pts',(72.1036751016059,-16.9981470538884,3.3391048451961));
#39972=CARTESIAN_POINT('Ctrl Pts',(72.3571630257949,-16.9854005733312,3.59395109245192));
#39973=CARTESIAN_POINT('Ctrl Pts',(72.8625769660851,-16.8268077199093,4.09137516053087));
#39974=CARTESIAN_POINT('Ctrl Pts',(73.3355464350895,-16.3991227020429,4.53567658281546));
#39975=CARTESIAN_POINT('Ctrl Pts',(73.6132058254433,-15.9274342791999,4.78738301567102));
#39976=CARTESIAN_POINT('Ctrl Pts',(73.6666666666667,-15.6672482052684,4.83333333333333));
#39977=CARTESIAN_POINT('Ctrl Pts',(73.6666666666667,-15.5,4.83333333333333));
#39978=CARTESIAN_POINT('Ctrl Pts',(72.3391048451961,-16.9981470538884,3.10367510160594));
#39979=CARTESIAN_POINT('Ctrl Pts',(72.5939510924519,-16.9854005733312,3.35716302579493));
#39980=CARTESIAN_POINT('Ctrl Pts',(73.0913751605309,-16.8268077199093,3.86257696608515));
#39981=CARTESIAN_POINT('Ctrl Pts',(73.5356765828154,-16.3991227020429,4.3355464350895));
#39982=CARTESIAN_POINT('Ctrl Pts',(73.787383015671,-15.9274342791999,4.61320582544333));
#39983=CARTESIAN_POINT('Ctrl Pts',(73.8333333333333,-15.6672482052684,4.66666666666667));
#39984=CARTESIAN_POINT('Ctrl Pts',(73.8333333333333,-15.5,4.66666666666667));
#39985=CARTESIAN_POINT('Ctrl Pts',(72.5745345887863,-16.9981470538884,2.86824535801578));
#39986=CARTESIAN_POINT('Ctrl Pts',(72.8307391591089,-16.9854005733312,3.12037495913794));
#39987=CARTESIAN_POINT('Ctrl Pts',(73.3201733549766,-16.8268077199093,3.63377877163943));
#39988=CARTESIAN_POINT('Ctrl Pts',(73.7358067305414,-16.3991227020429,4.13541628736354));
#39989=CARTESIAN_POINT('Ctrl Pts',(73.9615602058987,-15.9274342791999,4.43902863521564));
#39990=CARTESIAN_POINT('Ctrl Pts',(74.,-15.6672482052684,4.5));
#39991=CARTESIAN_POINT('Ctrl Pts',(74.,-15.5,4.5));
#39992=CARTESIAN_POINT('',(73.5,-15.5,5.));
#39993=CARTESIAN_POINT('',(74.,-15.5,4.5));
#39994=CARTESIAN_POINT('Ctrl Pts',(73.5,-15.5,5.));
#39995=CARTESIAN_POINT('Ctrl Pts',(73.5,-15.6672482052684,5.));
#39996=CARTESIAN_POINT('Ctrl Pts',(73.4390286352156,-15.9274342791999,4.9615602058987));
#39997=CARTESIAN_POINT('Ctrl Pts',(73.1354162873635,-16.3991227020429,4.73580673054142));
#39998=CARTESIAN_POINT('Ctrl Pts',(72.6337787716394,-16.8268077199093,4.32017335497658));
#39999=CARTESIAN_POINT('Ctrl Pts',(72.1203749591379,-16.9854005733312,3.83073915910891));
#40000=CARTESIAN_POINT('Ctrl Pts',(71.8682453580158,-16.9981470538884,3.57453458878625));
#40001=CARTESIAN_POINT('Origin',(73.75,-14.,4.75));
#40002=CARTESIAN_POINT('',(73.5,-14.,5.));
#40003=CARTESIAN_POINT('',(33.7499999999998,-14.,44.7499999999997));
#40004=CARTESIAN_POINT('',(73.5,-14.,5.));
#40005=CARTESIAN_POINT('Origin',(68.,-15.5,3.5));
#40006=CARTESIAN_POINT('',(56.2783262011229,-15.5,5.));
#40007=CARTESIAN_POINT('',(68.,-15.5,5.));
#40008=CARTESIAN_POINT('Ctrl Pts',(56.3914887194867,-17.,3.5));
#40009=CARTESIAN_POINT('Ctrl Pts',(56.379789702144,-17.,3.68849285843233));
#40010=CARTESIAN_POINT('Ctrl Pts',(56.366268079425,-16.9623071985392,3.88949595769794));
#40011=CARTESIAN_POINT('Ctrl Pts',(56.3395353657988,-16.8090480003591,4.25923828551908));
#40012=CARTESIAN_POINT('Ctrl Pts',(56.3263779287031,-16.6934822832211,4.42798167302478));
#40013=CARTESIAN_POINT('Ctrl Pts',(56.3048219679644,-16.4270526075957,4.69412389350913));
#40014=CARTESIAN_POINT('Ctrl Pts',(56.2949857165266,-16.2585410496607,4.8094152373875));
#40015=CARTESIAN_POINT('Ctrl Pts',(56.2817103328366,-15.889189778178,4.96235566707568));
#40016=CARTESIAN_POINT('Ctrl Pts',(56.2783262011229,-15.6883461217826,5.));
#40017=CARTESIAN_POINT('Ctrl Pts',(56.2783262011229,-15.5,5.));
#40018=CARTESIAN_POINT('Origin',(74.,-14.,5.));
#40019=CARTESIAN_POINT('',(56.2783262011229,-14.,5.));
#40020=CARTESIAN_POINT('',(37.,-14.,5.));
#40021=CARTESIAN_POINT('',(56.2783262011229,-16.45,5.));
#40022=CARTESIAN_POINT('Origin',(0.,-12.3786796564404,0.));
#40023=CARTESIAN_POINT('',(-1.12667505521556E-14,-12.3786796564404,-92.));
#40024=CARTESIAN_POINT('Origin',(0.,-12.3786796564404,0.));
#40025=CARTESIAN_POINT('',(-1.12129469407189E-14,-13.4393398282202,-91.5606601717798));
#40026=CARTESIAN_POINT('Origin',(-1.10830535322835E-14,-12.3786796564404,
-90.5));
#40027=CARTESIAN_POINT('Origin',(-8.40971020553915E-15,-13.4393398282202,
0.));
#40028=CARTESIAN_POINT('Origin',(0.,-13.5,0.));
#40029=CARTESIAN_POINT('',(-1.11980894836777E-14,-13.5606601717798,-91.4393398282202));
#40030=CARTESIAN_POINT('',(-1.12055182121983E-14,-13.5,-91.5));
#40031=CARTESIAN_POINT('Origin',(-8.39856711275827E-15,-13.5606601717798,
0.));
#40032=CARTESIAN_POINT('Origin',(0.,-6.5,0.));
#40033=CARTESIAN_POINT('',(-1.12667505521556E-14,-1.5,-92.));
#40034=CARTESIAN_POINT('Origin',(0.,-1.5,0.));
#40035=CARTESIAN_POINT('',(-1.12667505521556E-14,-6.5,-92.));
#40036=CARTESIAN_POINT('Origin',(0.,-12.5,0.));
#40037=CARTESIAN_POINT('',(-1.10681960752424E-14,-14.,-90.3786796564403));
#40038=CARTESIAN_POINT('Origin',(-1.10681960752424E-14,-12.5,-90.3786796564403));
#40039=CARTESIAN_POINT('Origin',(0.,-14.,0.));
#40040=CARTESIAN_POINT('Origin',(0.,-14.,91.));
#40041=CARTESIAN_POINT('',(25.8800414539374,-14.,-75.7581216659255));
#40042=CARTESIAN_POINT('Origin',(31.3800414539374,-14.,-75.7581216659255));
#40043=CARTESIAN_POINT('',(-81.2581216659255,-14.,-31.3800414539373));
#40044=CARTESIAN_POINT('Origin',(-75.7581216659255,-14.,-31.3800414539373));
#40045=CARTESIAN_POINT('',(-81.2581216659255,-14.,31.3800414539374));
#40046=CARTESIAN_POINT('Origin',(-75.7581216659255,-14.,31.3800414539374));
#40047=CARTESIAN_POINT('',(25.8800414539374,-14.,75.7581216659255));
#40048=CARTESIAN_POINT('Origin',(31.3800414539374,-14.,75.7581216659255));
#40049=CARTESIAN_POINT('',(-36.8800414539374,-14.,75.7581216659255));
#40050=CARTESIAN_POINT('Origin',(-31.3800414539374,-14.,75.7581216659255));
#40051=CARTESIAN_POINT('',(70.2581216659255,-14.,31.3800414539374));
#40052=CARTESIAN_POINT('Origin',(75.7581216659255,-14.,31.3800414539374));
#40053=CARTESIAN_POINT('',(-36.8800414539373,-14.,-75.7581216659255));
#40054=CARTESIAN_POINT('Origin',(-31.3800414539373,-14.,-75.7581216659255));
#40055=CARTESIAN_POINT('',(70.2581216659255,-14.,-31.3800414539373));
#40056=CARTESIAN_POINT('Origin',(75.7581216659255,-14.,-31.3800414539373));
#40057=CARTESIAN_POINT('',(-5.00000000000001,-14.,-56.2783262011229));
#40058=CARTESIAN_POINT('',(-5.,-14.,20.5));
#40059=CARTESIAN_POINT('',(-56.2783262011229,-14.,-4.99999999999999));
#40060=CARTESIAN_POINT('Origin',(0.,-14.,0.));
#40061=CARTESIAN_POINT('',(-72.5,-14.,-4.99999999999998));
#40062=CARTESIAN_POINT('',(-37.,-14.,-4.99999999999998));
#40063=CARTESIAN_POINT('Origin',(-72.5,-14.,-3.49999999999999));
#40064=CARTESIAN_POINT('',(-56.2783262011229,-14.,5.00000000000001));
#40065=CARTESIAN_POINT('',(-25.,-14.,5.));
#40066=CARTESIAN_POINT('Origin',(0.,-14.,0.));
#40067=CARTESIAN_POINT('',(5.,-14.,56.2783262011229));
#40068=CARTESIAN_POINT('',(5.,-14.,70.5));
#40069=CARTESIAN_POINT('Origin',(0.,-14.,0.));
#40070=CARTESIAN_POINT('',(56.2783262011229,-14.,-5.));
#40071=CARTESIAN_POINT('',(25.,-14.,-5.));
#40072=CARTESIAN_POINT('Origin',(0.,-14.,0.));
#40073=CARTESIAN_POINT('Origin',(56.,-15.5,-3.5));
#40074=CARTESIAN_POINT('',(56.2783262011229,-15.5,-5.));
#40075=CARTESIAN_POINT('Ctrl Pts',(56.2783262011229,-15.5,-5.));
#40076=CARTESIAN_POINT('Ctrl Pts',(56.2783262011229,-15.6883461217826,-5.));
#40077=CARTESIAN_POINT('Ctrl Pts',(56.2817103328366,-15.889189778178,-4.96235566707568));
#40078=CARTESIAN_POINT('Ctrl Pts',(56.2949857165266,-16.2585410496607,-4.8094152373875));
#40079=CARTESIAN_POINT('Ctrl Pts',(56.3048219679644,-16.4270526075957,-4.69412389350913));
#40080=CARTESIAN_POINT('Ctrl Pts',(56.3263779287031,-16.6934822832211,-4.42798167302478));
#40081=CARTESIAN_POINT('Ctrl Pts',(56.3395353657988,-16.8090480003591,-4.25923828551909));
#40082=CARTESIAN_POINT('Ctrl Pts',(56.366268079425,-16.9623071985392,-3.88949595769795));
#40083=CARTESIAN_POINT('Ctrl Pts',(56.379789702144,-17.,-3.68849285843233));
#40084=CARTESIAN_POINT('Ctrl Pts',(56.3914887194867,-17.,-3.5));
#40085=CARTESIAN_POINT('',(56.,-15.5,-5.));
#40086=CARTESIAN_POINT('Origin',(50.,-14.,-5.));
#40087=CARTESIAN_POINT('',(56.2783262011229,-16.45,-5.));
#40088=CARTESIAN_POINT('Origin',(3.5,-15.5,56.));
#40089=CARTESIAN_POINT('',(5.,-15.5,56.2783262011229));
#40090=CARTESIAN_POINT('Ctrl Pts',(5.,-15.5,56.2783262011229));
#40091=CARTESIAN_POINT('Ctrl Pts',(5.,-15.6883461217826,56.2783262011229));
#40092=CARTESIAN_POINT('Ctrl Pts',(4.96235566707569,-15.889189778178,56.2817103328366));
#40093=CARTESIAN_POINT('Ctrl Pts',(4.8094152373875,-16.2585410496607,56.2949857165266));
#40094=CARTESIAN_POINT('Ctrl Pts',(4.69412389350913,-16.4270526075957,56.3048219679644));
#40095=CARTESIAN_POINT('Ctrl Pts',(4.42798167302478,-16.6934822832211,56.3263779287031));
#40096=CARTESIAN_POINT('Ctrl Pts',(4.25923828551909,-16.8090480003591,56.3395353657988));
#40097=CARTESIAN_POINT('Ctrl Pts',(3.88949595769795,-16.9623071985392,56.366268079425));
#40098=CARTESIAN_POINT('Ctrl Pts',(3.68849285843233,-17.,56.379789702144));
#40099=CARTESIAN_POINT('Ctrl Pts',(3.5,-17.,56.3914887194867));
#40100=CARTESIAN_POINT('',(5.,-15.5,56.));
#40101=CARTESIAN_POINT('Origin',(5.,-14.,50.));
#40102=CARTESIAN_POINT('',(5.,-16.45,56.2783262011229));
#40103=CARTESIAN_POINT('Origin',(0.,-1.5,0.));
#40104=CARTESIAN_POINT('',(-1.10830535322835E-14,0.,-90.5));
#40105=CARTESIAN_POINT('Origin',(0.,0.,0.));
#40106=CARTESIAN_POINT('Origin',(-1.10830535322835E-14,-1.5,-90.5));
#40107=CARTESIAN_POINT('Origin',(0.,0.,0.));
#40108=CARTESIAN_POINT('',(-70.9934791577936,0.,-28.6326460019314));
#40109=CARTESIAN_POINT('',(-70.9934791577936,0.,28.6326460019316));
#40110=CARTESIAN_POINT('Origin',(0.,0.,0.));
#40111=CARTESIAN_POINT('',(-81.2581216659255,0.,-31.3800414539373));
#40112=CARTESIAN_POINT('Origin',(-75.7581216659255,0.,-31.3800414539373));
#40113=CARTESIAN_POINT('',(-70.4463086837813,0.,-29.9536323812221));
#40114=CARTESIAN_POINT('Origin',(-75.7581216659255,0.,-31.3800414539373));
#40115=CARTESIAN_POINT('',(-29.9536323812221,0.,-70.4463086837813));
#40116=CARTESIAN_POINT('Origin',(0.,0.,0.));
#40117=CARTESIAN_POINT('',(-36.8800414539373,0.,-75.7581216659255));
#40118=CARTESIAN_POINT('Origin',(-31.3800414539373,0.,-75.7581216659255));
#40119=CARTESIAN_POINT('',(-28.6326460019314,0.,-70.9934791577936));
#40120=CARTESIAN_POINT('Origin',(-31.3800414539373,0.,-75.7581216659255));
#40121=CARTESIAN_POINT('',(28.6326460019314,0.,-70.9934791577936));
#40122=CARTESIAN_POINT('Origin',(0.,0.,0.));
#40123=CARTESIAN_POINT('',(25.8800414539374,0.,-75.7581216659255));
#40124=CARTESIAN_POINT('Origin',(31.3800414539374,0.,-75.7581216659255));
#40125=CARTESIAN_POINT('',(29.9536323812222,0.,-70.4463086837813));
#40126=CARTESIAN_POINT('Origin',(31.3800414539374,0.,-75.7581216659255));
#40127=CARTESIAN_POINT('',(70.4463086837813,0.,-29.9536323812221));
#40128=CARTESIAN_POINT('Origin',(0.,0.,0.));
#40129=CARTESIAN_POINT('',(70.2581216659255,0.,-31.3800414539373));
#40130=CARTESIAN_POINT('Origin',(75.7581216659255,0.,-31.3800414539373));
#40131=CARTESIAN_POINT('',(70.9934791577936,0.,-28.6326460019314));
#40132=CARTESIAN_POINT('Origin',(75.7581216659255,0.,-31.3800414539373));
#40133=CARTESIAN_POINT('',(70.9934791577936,0.,28.6326460019314));
#40134=CARTESIAN_POINT('Origin',(0.,0.,0.));
#40135=CARTESIAN_POINT('',(70.2581216659255,0.,31.3800414539374));
#40136=CARTESIAN_POINT('Origin',(75.7581216659255,0.,31.3800414539374));
#40137=CARTESIAN_POINT('',(70.4463086837813,0.,29.9536323812221));
#40138=CARTESIAN_POINT('Origin',(75.7581216659255,0.,31.3800414539374));
#40139=CARTESIAN_POINT('',(29.953632381222,0.,70.4463086837814));
#40140=CARTESIAN_POINT('Origin',(0.,0.,0.));
#40141=CARTESIAN_POINT('',(25.8800414539374,0.,75.7581216659255));
#40142=CARTESIAN_POINT('Origin',(31.3800414539374,0.,75.7581216659255));
#40143=CARTESIAN_POINT('',(28.6326460019316,0.,70.9934791577936));
#40144=CARTESIAN_POINT('Origin',(31.3800414539374,0.,75.7581216659255));
#40145=CARTESIAN_POINT('',(-9.37467124747299E-15,0.,76.55));
#40146=CARTESIAN_POINT('Origin',(0.,0.,0.));
#40147=CARTESIAN_POINT('',(-28.6326460019314,0.,70.9934791577936));
#40148=CARTESIAN_POINT('Origin',(0.,0.,0.));
#40149=CARTESIAN_POINT('',(-36.8800414539374,0.,75.7581216659255));
#40150=CARTESIAN_POINT('Origin',(-31.3800414539374,0.,75.7581216659255));
#40151=CARTESIAN_POINT('',(-29.9536323812221,0.,70.4463086837813));
#40152=CARTESIAN_POINT('Origin',(-31.3800414539374,0.,75.7581216659255));
#40153=CARTESIAN_POINT('',(-70.4463086837814,0.,29.953632381222));
#40154=CARTESIAN_POINT('Origin',(0.,0.,0.));
#40155=CARTESIAN_POINT('',(-81.2581216659255,0.,31.3800414539374));
#40156=CARTESIAN_POINT('Origin',(-75.7581216659255,0.,31.3800414539374));
#40157=CARTESIAN_POINT('Origin',(-75.7581216659255,0.,31.3800414539374));
#40158=CARTESIAN_POINT('Origin',(0.,-18.5,0.));
#40159=CARTESIAN_POINT('',(-6.85059334670459E-15,-19.5606601717798,-55.9393398282202));
#40160=CARTESIAN_POINT('Origin',(-5.13794501002844E-15,-19.5606601717798,
0.));
#40161=CARTESIAN_POINT('',(-6.72069993826926E-15,-20.,-54.8786796564404));
#40162=CARTESIAN_POINT('Origin',(-6.72069993826926E-15,-18.5,-54.8786796564404));
#40163=CARTESIAN_POINT('Origin',(0.,-20.,0.));
#40164=CARTESIAN_POINT('Origin',(0.,-19.5,0.));
#40165=CARTESIAN_POINT('',(-6.86545080374577E-15,-19.4393398282202,-56.0606601717798));
#40166=CARTESIAN_POINT('Origin',(-5.14908810280933E-15,-19.4393398282202,
0.));
#40167=CARTESIAN_POINT('',(-6.85802207522518E-15,-19.5,-56.));
#40168=CARTESIAN_POINT('Origin',(0.,-20.,55.5));
#40169=CARTESIAN_POINT('',(-4.34959053993225,-20.,-4.15347838401794));
#40170=CARTESIAN_POINT('',(-6.39699831604958,-20.,-3.79740738868713));
#40171=CARTESIAN_POINT('Ctrl Pts',(-4.34959053993225,-20.,-4.15347838401794));
#40172=CARTESIAN_POINT('Ctrl Pts',(-5.57128190994263,-20.,-4.15347838401794));
#40173=CARTESIAN_POINT('Ctrl Pts',(-6.39699831604958,-20.,-3.79740738868713));
#40174=CARTESIAN_POINT('',(-7.69235968589783,-20.,-2.72612595558167));
#40175=CARTESIAN_POINT('Ctrl Pts',(-6.39699831604958,-20.,-3.79740738868713));
#40176=CARTESIAN_POINT('Ctrl Pts',(-7.2227144241333,-20.,-3.44133758544922));
#40177=CARTESIAN_POINT('Ctrl Pts',(-7.69235968589783,-20.,-2.72612595558167));
#40178=CARTESIAN_POINT('',(-8.18656161427498,-20.,-1.10845828056335));
#40179=CARTESIAN_POINT('Ctrl Pts',(-7.69235968589783,-20.,-2.72612595558167));
#40180=CARTESIAN_POINT('Ctrl Pts',(-8.16200498491526,-20.,-2.01091432571411));
#40181=CARTESIAN_POINT('Ctrl Pts',(-8.18656161427498,-20.,-1.10845828056335));
#40182=CARTESIAN_POINT('',(-7.06309646368027,-20.,-1.0102322101593));
#40183=CARTESIAN_POINT('',(-1.66843011664469,-20.,-0.538569269720264));
#40184=CARTESIAN_POINT('',(-6.69167771935463,-20.,-2.11834931373596));
#40185=CARTESIAN_POINT('Ctrl Pts',(-7.06309646368027,-20.,-1.0102322101593));
#40186=CARTESIAN_POINT('Ctrl Pts',(-6.98328748345375,-20.,-1.68553912639618));
#40187=CARTESIAN_POINT('Ctrl Pts',(-6.69167771935463,-20.,-2.11834931373596));
#40188=CARTESIAN_POINT('',(-5.78615248203278,-20.,-2.81821274757385));
#40189=CARTESIAN_POINT('Ctrl Pts',(-6.69167771935463,-20.,-2.11834931373596));
#40190=CARTESIAN_POINT('Ctrl Pts',(-6.4000678062439,-20.,-2.55115950107574));
#40191=CARTESIAN_POINT('Ctrl Pts',(-5.78615248203278,-20.,-2.81821274757385));
#40192=CARTESIAN_POINT('',(-4.40484285354614,-20.,-3.08526659011841));
#40193=CARTESIAN_POINT('Ctrl Pts',(-5.78615248203278,-20.,-2.81821274757385));
#40194=CARTESIAN_POINT('Ctrl Pts',(-5.17223715782166,-20.,-3.08526659011841));
#40195=CARTESIAN_POINT('Ctrl Pts',(-4.40484285354614,-20.,-3.08526659011841));
#40196=CARTESIAN_POINT('',(-3.20156872272491,-20.,-2.88267397880554));
#40197=CARTESIAN_POINT('Ctrl Pts',(-4.40484285354614,-20.,-3.08526659011841));
#40198=CARTESIAN_POINT('Ctrl Pts',(-3.7233966588974,-20.,-3.08526659011841));
#40199=CARTESIAN_POINT('Ctrl Pts',(-3.20156872272491,-20.,-2.88267397880554));
#40200=CARTESIAN_POINT('',(-2.4249655008316,-20.,-2.32708060741425));
#40201=CARTESIAN_POINT('Ctrl Pts',(-3.20156872272491,-20.,-2.88267397880554));
#40202=CARTESIAN_POINT('Ctrl Pts',(-2.67974019050598,-20.,-2.68008136749268));
#40203=CARTESIAN_POINT('Ctrl Pts',(-2.4249655008316,-20.,-2.32708060741425));
#40204=CARTESIAN_POINT('',(-2.17019081115723,-20.,-1.5566166639328));
#40205=CARTESIAN_POINT('Ctrl Pts',(-2.4249655008316,-20.,-2.32708060741425));
#40206=CARTESIAN_POINT('Ctrl Pts',(-2.17019081115723,-20.,-1.97407925128937));
#40207=CARTESIAN_POINT('Ctrl Pts',(-2.17019081115723,-20.,-1.5566166639328));
#40208=CARTESIAN_POINT('',(-2.41575658321381,-20.,-0.816848516464234));
#40209=CARTESIAN_POINT('Ctrl Pts',(-2.17019081115723,-20.,-1.5566166639328));
#40210=CARTESIAN_POINT('Ctrl Pts',(-2.17019081115723,-20.,-1.13301539421082));
#40211=CARTESIAN_POINT('Ctrl Pts',(-2.41575658321381,-20.,-0.816848516464234));
#40212=CARTESIAN_POINT('',(-3.22612524032593,-20.,-0.28581166267395));
#40213=CARTESIAN_POINT('Ctrl Pts',(-2.41575658321381,-20.,-0.816848516464234));
#40214=CARTESIAN_POINT('Ctrl Pts',(-2.66132295131683,-20.,-0.500682830810547));
#40215=CARTESIAN_POINT('Ctrl Pts',(-3.22612524032593,-20.,-0.28581166267395));
#40216=CARTESIAN_POINT('',(-4.82844471931458,-20.,0.15313720703125));
#40217=CARTESIAN_POINT('Ctrl Pts',(-3.22612524032593,-20.,-0.28581166267395));
#40218=CARTESIAN_POINT('Ctrl Pts',(-3.5883355140686,-20.,-0.144611835479737));
#40219=CARTESIAN_POINT('Ctrl Pts',(-4.82844471931458,-20.,0.15313720703125));
#40220=CARTESIAN_POINT('',(-6.5658250451088,-20.,0.714870452880859));
#40221=CARTESIAN_POINT('Ctrl Pts',(-4.82844471931458,-20.,0.15313720703125));
#40222=CARTESIAN_POINT('Ctrl Pts',(-6.0685533285141,-20.,0.450886249542236));
#40223=CARTESIAN_POINT('Ctrl Pts',(-6.5658250451088,-20.,0.714870452880859));
#40224=CARTESIAN_POINT('',(-7.52660259604454,-20.,1.55286467075348));
#40225=CARTESIAN_POINT('Ctrl Pts',(-6.5658250451088,-20.,0.714870452880859));
#40226=CARTESIAN_POINT('Ctrl Pts',(-7.21043616533279,-20.,1.05252361297607));
#40227=CARTESIAN_POINT('Ctrl Pts',(-7.52660259604454,-20.,1.55286467075348));
#40228=CARTESIAN_POINT('',(-7.84276902675629,-20.,2.67326033115387));
#40229=CARTESIAN_POINT('Ctrl Pts',(-7.52660259604454,-20.,1.55286467075348));
#40230=CARTESIAN_POINT('Ctrl Pts',(-7.84276902675629,-20.,2.05320572853088));
#40231=CARTESIAN_POINT('Ctrl Pts',(-7.84276902675629,-20.,2.67326033115387));
#40232=CARTESIAN_POINT('',(-7.4560022354126,-20.,3.9471343755722));
#40233=CARTESIAN_POINT('Ctrl Pts',(-7.84276902675629,-20.,2.67326033115387));
#40234=CARTESIAN_POINT('Ctrl Pts',(-7.84276902675629,-20.,3.35470592975616));
#40235=CARTESIAN_POINT('Ctrl Pts',(-7.4560022354126,-20.,3.9471343755722));
#40236=CARTESIAN_POINT('',(-6.32639795541763,-20.,4.84652078151703));
#40237=CARTESIAN_POINT('Ctrl Pts',(-7.4560022354126,-20.,3.9471343755722));
#40238=CARTESIAN_POINT('Ctrl Pts',(-7.06923559308052,-20.,4.53956282138824));
#40239=CARTESIAN_POINT('Ctrl Pts',(-6.32639795541763,-20.,4.84652078151703));
#40240=CARTESIAN_POINT('',(-4.67496573925018,-20.,5.15347814559937));
#40241=CARTESIAN_POINT('Ctrl Pts',(-6.32639795541763,-20.,4.84652078151703));
#40242=CARTESIAN_POINT('Ctrl Pts',(-5.58356046676636,-20.,5.15347814559937));
#40243=CARTESIAN_POINT('Ctrl Pts',(-4.67496573925018,-20.,5.15347814559937));
#40244=CARTESIAN_POINT('',(-2.90995895862579,-20.,4.83117258548737));
#40245=CARTESIAN_POINT('Ctrl Pts',(-4.67496573925018,-20.,5.15347814559937));
#40246=CARTESIAN_POINT('Ctrl Pts',(-3.67428362369537,-20.,5.15347814559937));
#40247=CARTESIAN_POINT('Ctrl Pts',(-2.90995895862579,-20.,4.83117258548737));
#40248=CARTESIAN_POINT('',(-1.73431098461151,-20.,3.88267314434052));
#40249=CARTESIAN_POINT('Ctrl Pts',(-2.90995895862579,-20.,4.83117258548737));
#40250=CARTESIAN_POINT('Ctrl Pts',(-2.14563429355621,-20.,4.50886702537537));
#40251=CARTESIAN_POINT('Ctrl Pts',(-1.73431098461151,-20.,3.88267314434052));
#40252=CARTESIAN_POINT('',(-1.29229187965393,-20.,2.46452903747559));
#40253=CARTESIAN_POINT('Ctrl Pts',(-1.73431098461151,-20.,3.88267314434052));
#40254=CARTESIAN_POINT('Ctrl Pts',(-1.32298767566681,-20.,3.25647985935211));
#40255=CARTESIAN_POINT('Ctrl Pts',(-1.29229187965393,-20.,2.46452903747559));
#40256=CARTESIAN_POINT('',(-2.4341744184494,-20.,2.37858092784882));
#40257=CARTESIAN_POINT('',(1.33492752978397,-20.,2.6622766464846));
#40258=CARTESIAN_POINT('',(-3.05729866027832,-20.,3.66780316829681));
#40259=CARTESIAN_POINT('Ctrl Pts',(-2.4341744184494,-20.,2.37858092784882));
#40260=CARTESIAN_POINT('Ctrl Pts',(-2.52626180648804,-20.,3.2319233417511));
#40261=CARTESIAN_POINT('Ctrl Pts',(-3.05729866027832,-20.,3.66780316829681));
#40262=CARTESIAN_POINT('',(-4.62585210800171,-20.,4.10368299484253));
#40263=CARTESIAN_POINT('Ctrl Pts',(-3.05729866027832,-20.,3.66780316829681));
#40264=CARTESIAN_POINT('Ctrl Pts',(-3.5883355140686,-20.,4.10368299484253));
#40265=CARTESIAN_POINT('Ctrl Pts',(-4.62585210800171,-20.,4.10368299484253));
#40266=CARTESIAN_POINT('',(-6.20054543018341,-20.,3.70770728588104));
#40267=CARTESIAN_POINT('Ctrl Pts',(-4.62585210800171,-20.,4.10368299484253));
#40268=CARTESIAN_POINT('Ctrl Pts',(-5.70634365081787,-20.,4.10368299484253));
#40269=CARTESIAN_POINT('Ctrl Pts',(-6.20054543018341,-20.,3.70770728588104));
#40270=CARTESIAN_POINT('',(-6.69474720954895,-20.,2.75306916236877));
#40271=CARTESIAN_POINT('Ctrl Pts',(-6.20054543018341,-20.,3.70770728588104));
#40272=CARTESIAN_POINT('Ctrl Pts',(-6.69474720954895,-20.,3.311732172966));
#40273=CARTESIAN_POINT('Ctrl Pts',(-6.69474720954895,-20.,2.75306916236877));
#40274=CARTESIAN_POINT('',(-6.34481549263,-20.,1.95497906208038));
#40275=CARTESIAN_POINT('Ctrl Pts',(-6.69474720954895,-20.,2.75306916236877));
#40276=CARTESIAN_POINT('Ctrl Pts',(-6.69474720954895,-20.,2.26807570457458));
#40277=CARTESIAN_POINT('Ctrl Pts',(-6.34481549263,-20.,1.95497906208038));
#40278=CARTESIAN_POINT('',(-4.54911291599274,-20.,1.31343758106232));
#40279=CARTESIAN_POINT('Ctrl Pts',(-6.34481549263,-20.,1.95497906208038));
#40280=CARTESIAN_POINT('Ctrl Pts',(-6.00102305412292,-20.,1.64188241958618));
#40281=CARTESIAN_POINT('Ctrl Pts',(-4.54911291599274,-20.,1.31343758106232));
#40282=CARTESIAN_POINT('',(-2.55695760250092,-20.,0.739426374435425));
#40283=CARTESIAN_POINT('Ctrl Pts',(-4.54911291599274,-20.,1.31343758106232));
#40284=CARTESIAN_POINT('Ctrl Pts',(-3.09720277786255,-20.,0.984992742538452));
#40285=CARTESIAN_POINT('Ctrl Pts',(-2.55695760250092,-20.,0.739426374435425));
#40286=CARTESIAN_POINT('',(-1.39665722846985,-20.,-0.1783766746521));
#40287=CARTESIAN_POINT('Ctrl Pts',(-2.55695760250092,-20.,0.739426374435425));
#40288=CARTESIAN_POINT('Ctrl Pts',(-1.77114546298981,-20.,0.377216696739197));
#40289=CARTESIAN_POINT('Ctrl Pts',(-1.39665722846985,-20.,-0.1783766746521));
#40290=CARTESIAN_POINT('',(-1.02216899394989,-20.,-1.4583899974823));
#40291=CARTESIAN_POINT('Ctrl Pts',(-1.39665722846985,-20.,-0.1783766746521));
#40292=CARTESIAN_POINT('Ctrl Pts',(-1.02216899394989,-20.,-0.733970642089844));
#40293=CARTESIAN_POINT('Ctrl Pts',(-1.02216899394989,-20.,-1.4583899974823));
#40294=CARTESIAN_POINT('',(-1.43349230289459,-20.,-2.81207346916199));
#40295=CARTESIAN_POINT('Ctrl Pts',(-1.02216899394989,-20.,-1.4583899974823));
#40296=CARTESIAN_POINT('Ctrl Pts',(-1.02216899394989,-20.,-2.17667126655579));
#40297=CARTESIAN_POINT('Ctrl Pts',(-1.43349230289459,-20.,-2.81207346916199));
#40298=CARTESIAN_POINT('',(-2.61527955532074,-20.,-3.80047702789307));
#40299=CARTESIAN_POINT('Ctrl Pts',(-1.43349230289459,-20.,-2.81207346916199));
#40300=CARTESIAN_POINT('Ctrl Pts',(-1.84481561183929,-20.,-3.44747567176819));
#40301=CARTESIAN_POINT('Ctrl Pts',(-2.61527955532074,-20.,-3.80047702789307));
#40302=CARTESIAN_POINT('Ctrl Pts',(-2.61527955532074,-20.,-3.80047702789307));
#40303=CARTESIAN_POINT('Ctrl Pts',(-3.38574349880219,-20.,-4.15347838401794));
#40304=CARTESIAN_POINT('Ctrl Pts',(-4.34959053993225,-20.,-4.15347838401794));
#40305=CARTESIAN_POINT('',(25.4253059625626,-20.,4.99999976158142));
#40306=CARTESIAN_POINT('',(21.833900809288,-20.,-0.187585592269898));
#40307=CARTESIAN_POINT('',(33.1234064883977,-20.,16.1194785828128));
#40308=CARTESIAN_POINT('',(21.833900809288,-20.,-4.));
#40309=CARTESIAN_POINT('',(21.833900809288,-20.,27.656207203865));
#40310=CARTESIAN_POINT('',(20.6429049372673,-20.,-4.));
#40311=CARTESIAN_POINT('',(10.916950404644,-20.,-4.));
#40312=CARTESIAN_POINT('',(20.6429049372673,-20.,-0.187585592269898));
#40313=CARTESIAN_POINT('',(20.6429049372673,-20.,25.75));
#40314=CARTESIAN_POINT('',(17.1742831147276,-20.,4.99999976158142));
#40315=CARTESIAN_POINT('',(4.58852554825927,-20.,23.8229487480263));
#40316=CARTESIAN_POINT('',(18.6231234669685,-20.,4.99999976158142));
#40317=CARTESIAN_POINT('',(8.58714155736379,-20.,4.99999976158142));
#40318=CARTESIAN_POINT('',(20.3973388671875,-20.,2.28649353981018));
#40319=CARTESIAN_POINT('',(4.2691955553234,-20.,26.9530685323169));
#40320=CARTESIAN_POINT('',(21.3120725750923,-20.,0.763983488082886));
#40321=CARTESIAN_POINT('Ctrl Pts',(20.3973388671875,-20.,2.28649353981018));
#40322=CARTESIAN_POINT('Ctrl Pts',(20.8884710073471,-20.,1.52523851394653));
#40323=CARTESIAN_POINT('Ctrl Pts',(21.3120725750923,-20.,0.763983488082886));
#40324=CARTESIAN_POINT('',(22.2943377494812,-20.,2.3540244102478));
#40325=CARTESIAN_POINT('Ctrl Pts',(21.3120725750923,-20.,0.763983488082886));
#40326=CARTESIAN_POINT('Ctrl Pts',(21.7172569036484,-20.,1.46998620033264));
#40327=CARTESIAN_POINT('Ctrl Pts',(22.2943377494812,-20.,2.3540244102478));
#40328=CARTESIAN_POINT('',(24.0378570556641,-20.,4.99999976158142));
#40329=CARTESIAN_POINT('',(31.1284359424709,-20.,15.7607047877004));
#40330=CARTESIAN_POINT('',(12.018928527832,-20.,4.99999976158142));
#40331=CARTESIAN_POINT('',(-25.6470237061142,-20.,4.99999976158142));
#40332=CARTESIAN_POINT('',(-18.0214869976044,-20.,4.99999976158142));
#40333=CARTESIAN_POINT('',(-12.2644948586822,-20.,4.99999976158142));
#40334=CARTESIAN_POINT('',(-18.0214869976044,-20.,3.93792605400085));
#40335=CARTESIAN_POINT('',(-18.0214869976044,-20.,30.2499998807907));
#40336=CARTESIAN_POINT('',(-23.3379939198494,-20.,3.93792605400085));
#40337=CARTESIAN_POINT('',(-9.01074349880219,-20.,3.93792605400085));
#40338=CARTESIAN_POINT('',(-23.3379939198494,-20.,1.18144607543945));
#40339=CARTESIAN_POINT('',(-23.3379939198494,-20.,29.7189630270004));
#40340=CARTESIAN_POINT('',(-18.3591401576996,-20.,1.18144607543945));
#40341=CARTESIAN_POINT('',(-11.6689969599247,-20.,1.18144607543945));
#40342=CARTESIAN_POINT('',(-18.3591401576996,-20.,0.125511646270752));
#40343=CARTESIAN_POINT('',(-18.3591401576996,-20.,28.3407230377197));
#40344=CARTESIAN_POINT('',(-23.3379939198494,-20.,0.125511646270752));
#40345=CARTESIAN_POINT('',(-9.17957007884979,-20.,0.125511646270748));
#40346=CARTESIAN_POINT('',(-23.3379939198494,-20.,-2.93792629241943));
#40347=CARTESIAN_POINT('',(-23.3379939198494,-20.,27.8127558231354));
#40348=CARTESIAN_POINT('',(-17.8127557039261,-20.,-2.93792629241943));
#40349=CARTESIAN_POINT('',(-11.6689969599247,-20.,-2.93792629241944));
#40350=CARTESIAN_POINT('',(-17.8127557039261,-20.,-4.));
#40351=CARTESIAN_POINT('',(-17.8127557039261,-20.,26.2810368537903));
#40352=CARTESIAN_POINT('',(-25.6470237061142,-20.,-4.));
#40353=CARTESIAN_POINT('',(-8.90637785196304,-20.,-4.));
#40354=CARTESIAN_POINT('',(-25.6470237061142,-20.,-4.));
#40355=CARTESIAN_POINT('',(-17.3346091195702,-20.,4.99999976158142));
#40356=CARTESIAN_POINT('',(-12.8400406241417,-20.,4.99999976158142));
#40357=CARTESIAN_POINT('',(-8.10828756541014,-20.,4.99999976158142));
#40358=CARTESIAN_POINT('',(-11.1855381727219,-20.,4.72680723667145));
#40359=CARTESIAN_POINT('Ctrl Pts',(-12.8400406241417,-20.,4.99999976158142));
#40360=CARTESIAN_POINT('Ctrl Pts',(-11.8086624145508,-20.,4.99999976158142));
#40361=CARTESIAN_POINT('Ctrl Pts',(-11.1855381727219,-20.,4.72680723667145));
#40362=CARTESIAN_POINT('',(-10.2094125747681,-20.,3.8857433795929));
#40363=CARTESIAN_POINT('Ctrl Pts',(-11.1855381727219,-20.,4.72680723667145));
#40364=CARTESIAN_POINT('Ctrl Pts',(-10.5624139308929,-20.,4.45361471176147));
#40365=CARTESIAN_POINT('Ctrl Pts',(-10.2094125747681,-20.,3.8857433795929));
#40366=CARTESIAN_POINT('',(-9.85641181468963,-20.,2.69781684875488));
#40367=CARTESIAN_POINT('Ctrl Pts',(-10.2094125747681,-20.,3.8857433795929));
#40368=CARTESIAN_POINT('Ctrl Pts',(-9.85641181468963,-20.,3.31787145137787));
#40369=CARTESIAN_POINT('Ctrl Pts',(-9.85641181468963,-20.,2.69781684875488));
#40370=CARTESIAN_POINT('',(-10.1695084571838,-20.,1.6111866235733));
#40371=CARTESIAN_POINT('Ctrl Pts',(-9.85641181468963,-20.,2.69781684875488));
#40372=CARTESIAN_POINT('Ctrl Pts',(-9.85641181468963,-20.,2.12073659896851));
#40373=CARTESIAN_POINT('Ctrl Pts',(-10.1695084571838,-20.,1.6111866235733));
#40374=CARTESIAN_POINT('',(-11.1149382591248,-20.,0.788540005683899));
#40375=CARTESIAN_POINT('Ctrl Pts',(-10.1695084571838,-20.,1.6111866235733));
#40376=CARTESIAN_POINT('Ctrl Pts',(-10.482605099678,-20.,1.1016366481781));
#40377=CARTESIAN_POINT('Ctrl Pts',(-11.1149382591248,-20.,0.788540005683899));
#40378=CARTESIAN_POINT('',(-9.85948085784912,-20.,-0.0279673337936404));
#40379=CARTESIAN_POINT('Ctrl Pts',(-11.1149382591248,-20.,0.788540005683899));
#40380=CARTESIAN_POINT('Ctrl Pts',(-10.2984303236008,-20.,0.549112915992737));
#40381=CARTESIAN_POINT('Ctrl Pts',(-9.85948085784912,-20.,-0.0279673337936404));
#40382=CARTESIAN_POINT('',(-9.42053139209747,-20.,-1.39085972309113));
#40383=CARTESIAN_POINT('Ctrl Pts',(-9.85948085784912,-20.,-0.0279673337936404));
#40384=CARTESIAN_POINT('Ctrl Pts',(-9.42053139209747,-20.,-0.605048179626465));
#40385=CARTESIAN_POINT('Ctrl Pts',(-9.42053139209747,-20.,-1.39085972309113));
#40386=CARTESIAN_POINT('',(-9.68758463859558,-20.,-2.56650769710541));
#40387=CARTESIAN_POINT('Ctrl Pts',(-9.42053139209747,-20.,-1.39085972309113));
#40388=CARTESIAN_POINT('Ctrl Pts',(-9.42053139209747,-20.,-2.02319228649139));
#40389=CARTESIAN_POINT('Ctrl Pts',(-9.68758463859558,-20.,-2.56650769710541));
#40390=CARTESIAN_POINT('',(-10.3475439548492,-20.,-3.40450191497803));
#40391=CARTESIAN_POINT('Ctrl Pts',(-9.68758463859558,-20.,-2.56650769710541));
#40392=CARTESIAN_POINT('Ctrl Pts',(-9.95463788509369,-20.,-3.10982251167297));
#40393=CARTESIAN_POINT('Ctrl Pts',(-10.3475439548492,-20.,-3.40450191497803));
#40394=CARTESIAN_POINT('',(-11.3328778743744,-20.,-3.84959125518799));
#40395=CARTESIAN_POINT('Ctrl Pts',(-10.3475439548492,-20.,-3.40450191497803));
#40396=CARTESIAN_POINT('Ctrl Pts',(-10.7404494285583,-20.,-3.69918131828308));
#40397=CARTESIAN_POINT('Ctrl Pts',(-11.3328778743744,-20.,-3.84959125518799));
#40398=CARTESIAN_POINT('',(-12.7847883105278,-20.,-4.));
#40399=CARTESIAN_POINT('Ctrl Pts',(-11.3328778743744,-20.,-3.84959125518799));
#40400=CARTESIAN_POINT('Ctrl Pts',(-11.9253063201904,-20.,-4.));
#40401=CARTESIAN_POINT('Ctrl Pts',(-12.7847883105278,-20.,-4.));
#40402=CARTESIAN_POINT('',(-17.3346091195702,-20.,-4.));
#40403=CARTESIAN_POINT('',(-6.3923941552639,-20.,-4.));
#40404=CARTESIAN_POINT('',(-17.3346091195702,-20.,-4.));
#40405=CARTESIAN_POINT('',(-0.494909523403555,-20.,4.99999976158142));
#40406=CARTESIAN_POINT('',(4.61357444524765,-20.,4.99999976158142));
#40407=CARTESIAN_POINT('',(0.31156223267317,-20.,4.99999976158142));
#40408=CARTESIAN_POINT('',(6.44304215908051,-20.,4.75750303268433));
#40409=CARTESIAN_POINT('Ctrl Pts',(4.61357444524765,-20.,4.99999976158142));
#40410=CARTESIAN_POINT('Ctrl Pts',(5.81684827804566,-20.,4.99999976158142));
#40411=CARTESIAN_POINT('Ctrl Pts',(6.44304215908051,-20.,4.75750303268433));
#40412=CARTESIAN_POINT('',(7.44372427463532,-20.,3.90109097957611));
#40413=CARTESIAN_POINT('Ctrl Pts',(6.44304215908051,-20.,4.75750303268433));
#40414=CARTESIAN_POINT('Ctrl Pts',(7.06923604011536,-20.,4.51500630378723));
#40415=CARTESIAN_POINT('Ctrl Pts',(7.44372427463532,-20.,3.90109097957611));
#40416=CARTESIAN_POINT('',(7.81821250915528,-20.,2.54433786869049));
#40417=CARTESIAN_POINT('Ctrl Pts',(7.44372427463532,-20.,3.90109097957611));
#40418=CARTESIAN_POINT('Ctrl Pts',(7.81821250915528,-20.,3.28717565536499));
#40419=CARTESIAN_POINT('Ctrl Pts',(7.81821250915528,-20.,2.54433786869049));
#40420=CARTESIAN_POINT('',(7.19815790653229,-20.,0.92974042892456));
#40421=CARTESIAN_POINT('Ctrl Pts',(7.81821250915528,-20.,2.54433786869049));
#40422=CARTESIAN_POINT('Ctrl Pts',(7.81821250915528,-20.,1.58663010597229));
#40423=CARTESIAN_POINT('Ctrl Pts',(7.19815790653229,-20.,0.92974042892456));
#40424=CARTESIAN_POINT('',(5.28274238109589,-20.,0.0948152542114256));
#40425=CARTESIAN_POINT('Ctrl Pts',(7.19815790653229,-20.,0.92974042892456));
#40426=CARTESIAN_POINT('Ctrl Pts',(6.57810330390931,-20.,0.272850751876831));
#40427=CARTESIAN_POINT('Ctrl Pts',(5.28274238109589,-20.,0.0948152542114256));
#40428=CARTESIAN_POINT('',(6.00102305412293,-20.,-0.353342533111572));
#40429=CARTESIAN_POINT('Ctrl Pts',(5.28274238109589,-20.,0.0948152542114256));
#40430=CARTESIAN_POINT('Ctrl Pts',(5.7554566860199,-20.,-0.132333278656006));
#40431=CARTESIAN_POINT('Ctrl Pts',(6.00102305412293,-20.,-0.353342533111572));
#40432=CARTESIAN_POINT('',(6.98942661285401,-20.,-1.55047798156738));
#40433=CARTESIAN_POINT('Ctrl Pts',(6.00102305412293,-20.,-0.353342533111572));
#40434=CARTESIAN_POINT('Ctrl Pts',(6.52285099029541,-20.,-0.832196712493897));
#40435=CARTESIAN_POINT('Ctrl Pts',(6.98942661285401,-20.,-1.55047798156738));
#40436=CARTESIAN_POINT('',(7.89500652006261,-20.,-2.96744382018624));
#40437=CARTESIAN_POINT('',(-6.96767281131813,-20.,20.2882718988485));
#40438=CARTESIAN_POINT('',(10.9548091465744,-20.,4.99999976158142));
#40439=CARTESIAN_POINT('',(7.65239799219948,-20.,-3.5991740309707));
#40440=CARTESIAN_POINT('',(14.6435883014006,-20.,4.99999976158142));
#40441=CARTESIAN_POINT('',(6.07622772455216,-20.,4.99999976158142));
#40442=CARTESIAN_POINT('',(18.3270808427138,-20.,-4.));
#40443=CARTESIAN_POINT('',(14.4702638890185,-20.,5.42348905947456));
#40444=CARTESIAN_POINT('',(15.762277841568,-20.,-4.));
#40445=CARTESIAN_POINT('',(8.55951547622681,-20.,-4.));
#40446=CARTESIAN_POINT('',(14.7124826908112,-20.,-1.27421581745148));
#40447=CARTESIAN_POINT('',(4.76650014291145,-20.,24.5504432976375));
#40448=CARTESIAN_POINT('',(10.9491813182831,-20.,-1.27421581745148));
#40449=CARTESIAN_POINT('',(7.35624134540558,-20.,-1.27421581745148));
#40450=CARTESIAN_POINT('',(9.96077753603459,-20.,-4.));
#40451=CARTESIAN_POINT('',(19.410324588737,-20.,22.0596189038341));
#40452=CARTESIAN_POINT('',(7.05695748329163,-20.,-4.));
#40453=CARTESIAN_POINT('',(4.27745550870896,-20.,-4.));
#40454=CARTESIAN_POINT('',(5.86596190929413,-20.,-2.12755823135376));
#40455=CARTESIAN_POINT('',(-7.43172077059746,-20.,18.7785954266824));
#40456=CARTESIAN_POINT('',(5.00648021697998,-20.,-0.887449026107788));
#40457=CARTESIAN_POINT('Ctrl Pts',(5.86596190929413,-20.,-2.12755823135376));
#40458=CARTESIAN_POINT('Ctrl Pts',(5.34413397312165,-20.,-1.31719017028809));
#40459=CARTESIAN_POINT('Ctrl Pts',(5.00648021697998,-20.,-0.887449026107788));
#40460=CARTESIAN_POINT('',(4.40177381038666,-20.,-0.28581166267395));
#40461=CARTESIAN_POINT('Ctrl Pts',(5.00648021697998,-20.,-0.887449026107788));
#40462=CARTESIAN_POINT('Ctrl Pts',(4.66882705688477,-20.,-0.45770788192749));
#40463=CARTESIAN_POINT('Ctrl Pts',(4.40177381038666,-20.,-0.28581166267395));
#40464=CARTESIAN_POINT('',(3.85845869779587,-20.,-0.0463845729827883));
#40465=CARTESIAN_POINT('Ctrl Pts',(4.40177381038666,-20.,-0.28581166267395));
#40466=CARTESIAN_POINT('Ctrl Pts',(4.13472056388855,-20.,-0.11391544342041));
#40467=CARTESIAN_POINT('Ctrl Pts',(3.85845869779587,-20.,-0.0463845729827883));
#40468=CARTESIAN_POINT('',(3.1954300403595,-20.,-0.00341081619262718));
#40469=CARTESIAN_POINT('Ctrl Pts',(3.85845869779587,-20.,-0.0463845729827883));
#40470=CARTESIAN_POINT('Ctrl Pts',(3.65586668252945,-20.,-0.00341081619262718));
#40471=CARTESIAN_POINT('Ctrl Pts',(3.1954300403595,-20.,-0.00341081619262718));
#40472=CARTESIAN_POINT('',(1.81412041187287,-20.,-0.00341081619262718));
#40473=CARTESIAN_POINT('',(1.59771502017975,-20.,-0.00341081619263051));
#40474=CARTESIAN_POINT('',(1.81412041187287,-20.,-4.));
#40475=CARTESIAN_POINT('',(1.81412041187287,-20.,27.7482945919037));
#40476=CARTESIAN_POINT('',(-0.494909523403555,-20.,-4.));
#40477=CARTESIAN_POINT('',(0.907060205936434,-20.,-4.));
#40478=CARTESIAN_POINT('',(-0.494909523403555,-20.,-4.));
#40479=CARTESIAN_POINT('Origin',(-56.,-15.5,3.50000000000001));
#40480=CARTESIAN_POINT('',(-56.2783262011229,-15.5,5.00000000000001));
#40481=CARTESIAN_POINT('Ctrl Pts',(-56.2783262011229,-15.5,5.00000000000001));
#40482=CARTESIAN_POINT('Ctrl Pts',(-56.2783262011229,-15.6883461217826,
5.00000000000001));
#40483=CARTESIAN_POINT('Ctrl Pts',(-56.2817103328366,-15.889189778178,4.96235566707569));
#40484=CARTESIAN_POINT('Ctrl Pts',(-56.2949857165266,-16.2585410496607,
4.80941523738751));
#40485=CARTESIAN_POINT('Ctrl Pts',(-56.3048219679644,-16.4270526075957,
4.69412389350914));
#40486=CARTESIAN_POINT('Ctrl Pts',(-56.3263779287031,-16.6934822832211,
4.42798167302479));
#40487=CARTESIAN_POINT('Ctrl Pts',(-56.3395353657988,-16.8090480003591,
4.25923828551909));
#40488=CARTESIAN_POINT('Ctrl Pts',(-56.366268079425,-16.9623071985392,3.88949595769795));
#40489=CARTESIAN_POINT('Ctrl Pts',(-56.379789702144,-17.,3.68849285843234));
#40490=CARTESIAN_POINT('Ctrl Pts',(-56.3914887194867,-17.,3.50000000000001));
#40491=CARTESIAN_POINT('',(-56.,-15.5,5.00000000000001));
#40492=CARTESIAN_POINT('Origin',(-72.5,-14.,-3.49999999999999));
#40493=CARTESIAN_POINT('',(-72.5,-15.5,-4.99999999999999));
#40494=CARTESIAN_POINT('Origin',(-72.5,-15.5,-3.49999999999999));
#40495=CARTESIAN_POINT('',(-72.5,-14.,-4.99999999999999));
#40496=CARTESIAN_POINT('Origin',(-72.5,-15.5,-3.49999999999999));
#40497=CARTESIAN_POINT('Origin',(-72.5,-15.5,-3.49999999999999));
#40498=CARTESIAN_POINT('Origin',(-68.,-15.5,-3.49999999999999));
#40499=CARTESIAN_POINT('',(-56.2783262011229,-15.5,-4.99999999999999));
#40500=CARTESIAN_POINT('',(-68.,-15.5,-4.99999999999999));
#40501=CARTESIAN_POINT('Ctrl Pts',(-56.3914887194867,-17.,-3.49999999999999));
#40502=CARTESIAN_POINT('Ctrl Pts',(-56.379789702144,-17.,-3.68849285843232));
#40503=CARTESIAN_POINT('Ctrl Pts',(-56.366268079425,-16.9623071985392,-3.88949595769794));
#40504=CARTESIAN_POINT('Ctrl Pts',(-56.3395353657988,-16.8090480003591,
-4.25923828551908));
#40505=CARTESIAN_POINT('Ctrl Pts',(-56.3263779287031,-16.6934822832211,
-4.42798167302477));
#40506=CARTESIAN_POINT('Ctrl Pts',(-56.3048219679644,-16.4270526075957,
-4.69412389350912));
#40507=CARTESIAN_POINT('Ctrl Pts',(-56.2949857165266,-16.2585410496607,
-4.80941523738749));
#40508=CARTESIAN_POINT('Ctrl Pts',(-56.2817103328366,-15.889189778178,-4.96235566707568));
#40509=CARTESIAN_POINT('Ctrl Pts',(-56.2783262011229,-15.6883461217826,
-4.99999999999999));
#40510=CARTESIAN_POINT('Ctrl Pts',(-56.2783262011229,-15.5,-4.99999999999999));
#40511=CARTESIAN_POINT('Origin',(-74.,-14.,-4.99999999999999));
#40512=CARTESIAN_POINT('',(-56.2783262011229,-16.45,-4.99999999999999));
#40513=CARTESIAN_POINT('Origin',(0.,-18.3786796564404,0.));
#40514=CARTESIAN_POINT('',(-6.91925441518255E-15,-18.3786796564404,-56.5));
#40515=CARTESIAN_POINT('Origin',(0.,-18.3786796564404,0.));
#40516=CARTESIAN_POINT('Origin',(-6.73555739531044E-15,-18.3786796564404,
-55.));
#40517=CARTESIAN_POINT('Origin',(0.,-16.45,0.));
#40518=CARTESIAN_POINT('',(-5.00000000000001,-15.5,-56.2783262011229));
#40519=CARTESIAN_POINT('',(-5.00000000000001,-16.45,-56.2783262011229));
#40520=CARTESIAN_POINT('Ctrl Pts',(-5.00000000000001,-15.5,-56.2783262011229));
#40521=CARTESIAN_POINT('Ctrl Pts',(-5.00000000000001,-15.6883461217826,
-56.2783262011229));
#40522=CARTESIAN_POINT('Ctrl Pts',(-4.96235566707569,-15.889189778178,-56.2817103328366));
#40523=CARTESIAN_POINT('Ctrl Pts',(-4.80941523738751,-16.2585410496607,
-56.2949857165266));
#40524=CARTESIAN_POINT('Ctrl Pts',(-4.69412389350914,-16.4270526075957,
-56.3048219679644));
#40525=CARTESIAN_POINT('Ctrl Pts',(-4.42798167302479,-16.6934822832211,
-56.3263779287031));
#40526=CARTESIAN_POINT('Ctrl Pts',(-4.2592382855191,-16.8090480003591,-56.3395353657988));
#40527=CARTESIAN_POINT('Ctrl Pts',(-3.88949595769795,-16.9623071985392,
-56.366268079425));
#40528=CARTESIAN_POINT('Ctrl Pts',(-3.68849285843234,-17.,-56.379789702144));
#40529=CARTESIAN_POINT('Ctrl Pts',(-3.50000000000001,-17.,-56.3914887194867));
#40530=CARTESIAN_POINT('',(-6.91925441518255E-15,-16.45,-56.5));
#40531=CARTESIAN_POINT('',(-56.2783262011229,-16.45,5.00000000000001));
#40532=CARTESIAN_POINT('Origin',(-3.50000000000001,-15.5,-56.));
#40533=CARTESIAN_POINT('',(-5.00000000000001,-15.5,-56.));
#40534=CARTESIAN_POINT('Origin',(-5.00000000000001,-14.,-50.));
#40535=CARTESIAN_POINT('Origin',(-2.22044604925031E-15,-6.5,-1.11022302462516E-15));
#40536=CARTESIAN_POINT('',(-26.4408249076837,-5.,48.7968521341409));
#40537=CARTESIAN_POINT('',(26.4408249076837,-5.,48.7968521341409));
#40538=CARTESIAN_POINT('Origin',(-2.22044604925031E-15,-5.,-1.11022302462516E-15));
#40539=CARTESIAN_POINT('',(28.5,-6.5,49.363448015713));
#40540=CARTESIAN_POINT('Ctrl Pts',(26.4408249076837,-5.,48.7968521341409));
#40541=CARTESIAN_POINT('Ctrl Pts',(26.4433428933823,-5.,48.7975634354717));
#40542=CARTESIAN_POINT('Ctrl Pts',(26.4458608993077,-5.00000333058454,48.7982746736245));
#40543=CARTESIAN_POINT('Ctrl Pts',(26.6669469009444,-5.00058824010722,48.860716770933));
#40544=CARTESIAN_POINT('Ctrl Pts',(26.8870499673497,-5.02626861297965,48.9223486234079));
#40545=CARTESIAN_POINT('Ctrl Pts',(27.3015455654892,-5.12770348678069,49.037476260629));
#40546=CARTESIAN_POINT('Ctrl Pts',(27.4994252131301,-5.20145984176535,49.0919888636193));
#40547=CARTESIAN_POINT('Ctrl Pts',(27.8654608685803,-5.40254624808677,49.1921485479794));
#40548=CARTESIAN_POINT('Ctrl Pts',(28.0359950887546,-5.53136222218403,49.2384417005703));
#40549=CARTESIAN_POINT('Ctrl Pts',(28.2793834312809,-5.80849396878292,49.3042039204227));
#40550=CARTESIAN_POINT('Ctrl Pts',(28.3653378990205,-5.94334681379896,49.3273143295766));
#40551=CARTESIAN_POINT('Ctrl Pts',(28.4731331307579,-6.22254302463316,49.3562553083628));
#40552=CARTESIAN_POINT('Ctrl Pts',(28.5,-6.35969279486339,49.363448015713));
#40553=CARTESIAN_POINT('Ctrl Pts',(28.5,-6.5,49.363448015713));
#40554=CARTESIAN_POINT('',(-28.5,-6.5,49.363448015713));
#40555=CARTESIAN_POINT('Origin',(-2.22044604925031E-15,-6.5,-1.11022302462516E-15));
#40556=CARTESIAN_POINT('Ctrl Pts',(-28.5,-6.5,49.363448015713));
#40557=CARTESIAN_POINT('Ctrl Pts',(-28.5,-6.35969279486338,49.363448015713));
#40558=CARTESIAN_POINT('Ctrl Pts',(-28.4731331307579,-6.22254302463313,
49.3562553083628));
#40559=CARTESIAN_POINT('Ctrl Pts',(-28.3653378990205,-5.94334681379896,
49.3273143295766));
#40560=CARTESIAN_POINT('Ctrl Pts',(-28.2793834312809,-5.80849396878292,
49.3042039204227));
#40561=CARTESIAN_POINT('Ctrl Pts',(-28.0359950887546,-5.53136222218405,
49.2384417005703));
#40562=CARTESIAN_POINT('Ctrl Pts',(-27.8654608685804,-5.40254624808679,
49.1921485479794));
#40563=CARTESIAN_POINT('Ctrl Pts',(-27.4994252131301,-5.20145984176534,
49.0919888636193));
#40564=CARTESIAN_POINT('Ctrl Pts',(-27.3015455654892,-5.12770348678068,
49.037476260629));
#40565=CARTESIAN_POINT('Ctrl Pts',(-26.8870499673495,-5.0262686129796,48.9223486234078));
#40566=CARTESIAN_POINT('Ctrl Pts',(-26.666946900943,-5.00058824010721,48.8607167709328));
#40567=CARTESIAN_POINT('Ctrl Pts',(-26.4458608993078,-5.00000333058454,
48.7982746736245));
#40568=CARTESIAN_POINT('Ctrl Pts',(-26.4433428933823,-5.,48.7975634354716));
#40569=CARTESIAN_POINT('Ctrl Pts',(-26.4408249076837,-5.,48.7968521341409));
#40570=CARTESIAN_POINT('Origin',(31.4497077307402,-6.5,57.4724916728338));
#40571=CARTESIAN_POINT('',(33.7929481589963,-5.,61.5311031489229));
#40572=CARTESIAN_POINT('',(31.4497077307402,-5.,57.4724916728338));
#40573=CARTESIAN_POINT('',(35.1,-6.5,60.7949833456676));
#40574=CARTESIAN_POINT('Ctrl Pts',(35.1,-6.5,60.7949833456676));
#40575=CARTESIAN_POINT('Ctrl Pts',(35.1,-6.31165607666986,60.7949833456676));
#40576=CARTESIAN_POINT('Ctrl Pts',(35.0674179958086,-6.11075826580663,60.8138311041577));
#40577=CARTESIAN_POINT('Ctrl Pts',(34.9347215325305,-5.74118910309827,60.8901559359346));
#40578=CARTESIAN_POINT('Ctrl Pts',(34.8345853962734,-5.57251778949233,60.9475955008384));
#40579=CARTESIAN_POINT('Ctrl Pts',(34.603070183953,-5.30614953382508,61.0793359017089));
#40580=CARTESIAN_POINT('Ctrl Pts',(34.4562535838124,-5.19070605094542,61.1624128165762));
#40581=CARTESIAN_POINT('Ctrl Pts',(34.1337535001687,-5.03763156427752,61.3429786085339));
#40582=CARTESIAN_POINT('Ctrl Pts',(33.9580490505859,-5.,61.4404295613393));
#40583=CARTESIAN_POINT('Ctrl Pts',(33.7929481589963,-5.,61.5311031489229));
#40584=CARTESIAN_POINT('',(32.7487458364169,-6.5,56.7224916728338));
#40585=CARTESIAN_POINT('Origin',(-28.1497077307402,-6.5,51.7567240078565));
#40586=CARTESIAN_POINT('',(-35.1,-6.5,60.7949833456676));
#40587=CARTESIAN_POINT('',(-29.4487458364169,-6.5,51.0067240078565));
#40588=CARTESIAN_POINT('',(-33.7929481589964,-5.,61.5311031489229));
#40589=CARTESIAN_POINT('Ctrl Pts',(-33.7929481589964,-5.,61.5311031489229));
#40590=CARTESIAN_POINT('Ctrl Pts',(-33.9580490505859,-5.,61.4404295613392));
#40591=CARTESIAN_POINT('Ctrl Pts',(-34.1337535001687,-5.03763156427752,
61.3429786085339));
#40592=CARTESIAN_POINT('Ctrl Pts',(-34.4562535838124,-5.19070605094542,
61.1624128165762));
#40593=CARTESIAN_POINT('Ctrl Pts',(-34.603070183953,-5.30614953382508,61.0793359017089));
#40594=CARTESIAN_POINT('Ctrl Pts',(-34.8345853962734,-5.57251778949232,
60.9475955008384));
#40595=CARTESIAN_POINT('Ctrl Pts',(-34.9347215325305,-5.74118910309827,
60.8901559359346));
#40596=CARTESIAN_POINT('Ctrl Pts',(-35.0674179958086,-6.11075826580663,
60.8138311041577));
#40597=CARTESIAN_POINT('Ctrl Pts',(-35.1,-6.31165607666986,60.7949833456676));
#40598=CARTESIAN_POINT('Ctrl Pts',(-35.1,-6.5,60.7949833456676));
#40599=CARTESIAN_POINT('',(-28.1497077307402,-5.,51.7567240078565));
#40600=CARTESIAN_POINT('Origin',(0.,-5.,70.2));
#40601=CARTESIAN_POINT('Origin',(0.,-5.,0.));
#40602=CARTESIAN_POINT('Origin',(0.,-4.52901994577491,0.));
#40603=CARTESIAN_POINT('',(-8.61200836217972E-15,-4.52901994577491,70.2));
#40604=CARTESIAN_POINT('',(-8.59702053001442E-15,-4.52901994577491,-70.2));
#40605=CARTESIAN_POINT('Origin',(0.,-4.52901994577491,0.));
#40606=CARTESIAN_POINT('Origin',(0.,-4.52901994577491,0.));
#40607=CARTESIAN_POINT('',(0.,-3.05,71.95));
#40608=CARTESIAN_POINT('Origin',(-8.79602563487587E-15,-4.52901994577491,
71.7));
#40609=CARTESIAN_POINT('Origin',(0.,-3.05,0.));
#40610=CARTESIAN_POINT('Origin',(0.,-2.45,0.));
#40611=CARTESIAN_POINT('',(-35.1,-9.,60.7949833456676));
#40612=CARTESIAN_POINT('',(-35.1,-5.,60.7949833456676));
#40613=CARTESIAN_POINT('',(-8.59702053001442E-15,-9.,-70.2));
#40614=CARTESIAN_POINT('Origin',(1.55431223447522E-14,-9.,2.22044604925031E-15));
#40615=CARTESIAN_POINT('',(-8.59702053001442E-15,-2.45,-70.2));
#40616=CARTESIAN_POINT('',(35.1,-9.,60.7949833456676));
#40617=CARTESIAN_POINT('Origin',(1.55431223447522E-14,-9.,2.22044604925031E-15));
#40618=CARTESIAN_POINT('',(35.1,-5.,60.7949833456676));
#40619=CARTESIAN_POINT('Origin',(0.,-1.5,0.));
#40620=CARTESIAN_POINT('Ctrl Pts',(29.9536323812222,-2.71050543121376E-19,
-70.4463086837813));
#40621=CARTESIAN_POINT('Ctrl Pts',(29.4931113267111,3.61002085224869E-16,
-70.5699748242382));
#40622=CARTESIAN_POINT('Ctrl Pts',(29.0477953810644,-8.57026255143317E-17,
-70.754095087701));
#40623=CARTESIAN_POINT('Ctrl Pts',(28.6326460019314,-6.68817215151996E-17,
-70.9934791577936));
#40624=CARTESIAN_POINT('Ctrl Pts',(-28.6326460019314,1.4975542507456E-17,
-70.9934791577936));
#40625=CARTESIAN_POINT('Ctrl Pts',(-29.0457287289759,2.12326426962524E-18,
-70.7552867637899));
#40626=CARTESIAN_POINT('Ctrl Pts',(-29.4908073407614,-9.21355752057452E-17,
-70.570593525701));
#40627=CARTESIAN_POINT('Ctrl Pts',(-29.9536323812221,-8.76170880639848E-17,
-70.4463086837813));
#40628=CARTESIAN_POINT('Ctrl Pts',(-70.4463086837813,-3.38135552543917E-17,
-29.9536323812221));
#40629=CARTESIAN_POINT('Ctrl Pts',(-70.5699748242384,-4.02332320349957E-17,
-29.4931113267108));
#40630=CARTESIAN_POINT('Ctrl Pts',(-70.7540950877011,6.7489870141098E-18,
-29.0477953810642));
#40631=CARTESIAN_POINT('Ctrl Pts',(-70.9934791577937,1.68728963093057E-17,
-28.6326460019314));
#40632=CARTESIAN_POINT('Ctrl Pts',(-70.9934791577936,-2.71050543121376E-19,
28.6326460019316));
#40633=CARTESIAN_POINT('Ctrl Pts',(-70.75528676379,-4.16998824018934E-16,
29.0457287289757));
#40634=CARTESIAN_POINT('Ctrl Pts',(-70.5705935257011,-4.11774089579395E-16,
29.4908073407612));
#40635=CARTESIAN_POINT('Ctrl Pts',(-70.4463086837814,7.45388993583784E-19,
29.953632381222));
#40636=CARTESIAN_POINT('Ctrl Pts',(-29.9536323812221,-6.22060996463558E-17,
70.4463086837813));
#40637=CARTESIAN_POINT('Ctrl Pts',(-29.493111326711,3.15609360022052E-16,
70.5699748242383));
#40638=CARTESIAN_POINT('Ctrl Pts',(-29.0477953810643,-5.68950025513662E-17,
70.754095087701));
#40639=CARTESIAN_POINT('Ctrl Pts',(-28.6326460019314,-6.24771501894772E-17,
70.9934791577936));
#40640=CARTESIAN_POINT('',(-9.19097422760089E-15,-1.5,75.05));
#40641=CARTESIAN_POINT('Origin',(-9.37467124747299E-15,-1.5,76.55));
#40642=CARTESIAN_POINT('',(9.19097422760089E-15,-1.5,-75.05));
#40643=CARTESIAN_POINT('Origin',(0.,-1.5,0.));
#40644=CARTESIAN_POINT('Origin',(0.,-1.5,0.));
#40645=CARTESIAN_POINT('Ctrl Pts',(28.6326460019316,1.74827600313288E-17,
70.9934791577936));
#40646=CARTESIAN_POINT('Ctrl Pts',(29.0457287289756,-7.84991024395544E-16,
70.75528676379));
#40647=CARTESIAN_POINT('Ctrl Pts',(29.4908073407612,-3.46969577256769E-16,
70.5705935257011));
#40648=CARTESIAN_POINT('Ctrl Pts',(29.953632381222,6.44422666271072E-17,
70.4463086837814));
#40649=CARTESIAN_POINT('Ctrl Pts',(70.4463086837813,-1.61817174243462E-16,
29.9536323812221));
#40650=CARTESIAN_POINT('Ctrl Pts',(70.5699748242384,2.02397638118641E-16,
29.4931113267108));
#40651=CARTESIAN_POINT('Ctrl Pts',(70.7540950877011,3.82018796963149E-16,
29.0477953810642));
#40652=CARTESIAN_POINT('Ctrl Pts',(70.9934791577936,1.31459513413867E-17,
28.6326460019314));
#40653=CARTESIAN_POINT('Ctrl Pts',(70.9934791577936,1.03676832743926E-17,
-28.6326460019314));
#40654=CARTESIAN_POINT('Ctrl Pts',(70.7552867637899,-2.39154738916311E-18,
-29.0457287289758));
#40655=CARTESIAN_POINT('Ctrl Pts',(70.5705935257011,-5.99316384971288E-17,
-29.4908073407614));
#40656=CARTESIAN_POINT('Ctrl Pts',(70.4463086837813,-4.58075417875126E-17,
-29.9536323812221));
#40657=CARTESIAN_POINT('Origin',(-75.7581216659255,-14.1,-31.3800414539373));
#40658=CARTESIAN_POINT('',(-81.2581216659255,-14.1,-31.3800414539373));
#40659=CARTESIAN_POINT('Origin',(-31.3800414539373,-14.1,-75.7581216659255));
#40660=CARTESIAN_POINT('',(-36.8800414539373,-14.1,-75.7581216659255));
#40661=CARTESIAN_POINT('Origin',(31.3800414539374,-14.1,-75.7581216659255));
#40662=CARTESIAN_POINT('',(25.8800414539374,-14.1,-75.7581216659255));
#40663=CARTESIAN_POINT('Origin',(75.7581216659255,-14.1,-31.3800414539373));
#40664=CARTESIAN_POINT('',(70.2581216659255,-14.1,-31.3800414539373));
#40665=CARTESIAN_POINT('Origin',(0.,-1.475,0.));
#40666=CARTESIAN_POINT('',(-9.19097422760089E-15,-3.05,-75.05));
#40667=CARTESIAN_POINT('Origin',(0.,-3.05,0.));
#40668=CARTESIAN_POINT('',(-9.19097422760089E-15,-1.475,-75.05));
#40669=CARTESIAN_POINT('Origin',(-0.494909523403555,-18.5,-4.));
#40670=CARTESIAN_POINT('',(0.623124465346341,-19.5,4.99999976158142));
#40671=CARTESIAN_POINT('Origin',(-0.494909523403555,-18.5,4.99999976158142));
#40672=CARTESIAN_POINT('',(0.623124465346341,-19.5,-4.));
#40673=CARTESIAN_POINT('Origin',(-0.494909523403555,-18.5,-4.));
#40674=CARTESIAN_POINT('',(0.623124465346341,-19.5,-4.));
#40675=CARTESIAN_POINT('Origin',(-17.3346091195702,-18.5,-4.));
#40676=CARTESIAN_POINT('',(-16.2165751308203,-19.5,4.99999976158142));
#40677=CARTESIAN_POINT('Origin',(-17.3346091195702,-18.5,4.99999976158142));
#40678=CARTESIAN_POINT('',(-16.2165751308203,-19.5,-4.));
#40679=CARTESIAN_POINT('Origin',(-17.3346091195702,-18.5,-4.));
#40680=CARTESIAN_POINT('',(-16.2165751308203,-19.5,-4.));
#40681=CARTESIAN_POINT('Origin',(-25.6470237061142,-18.5,-4.));
#40682=CARTESIAN_POINT('',(-24.5289897173643,-19.5,4.99999976158142));
#40683=CARTESIAN_POINT('Origin',(-25.6470237061142,-18.5,4.99999976158142));
#40684=CARTESIAN_POINT('',(-24.5289897173643,-19.5,-4.));
#40685=CARTESIAN_POINT('Origin',(-25.6470237061142,-18.5,-4.));
#40686=CARTESIAN_POINT('',(-24.5289897173643,-19.5,-4.));
#40687=CARTESIAN_POINT('Origin',(7.65239799219948,-18.5,-3.5991740309707));
#40688=CARTESIAN_POINT('',(12.1524554491043,-19.5,4.99999976158142));
#40689=CARTESIAN_POINT('Origin',(10.9548091465744,-18.5,4.99999976158142));
#40690=CARTESIAN_POINT('',(8.55491101741791,-19.6302085441738,-4.));
#40691=CARTESIAN_POINT('Origin',(7.89500652006261,-18.5,-2.96744382018624));
#40692=CARTESIAN_POINT('',(8.69611181435176,-19.5,-4.));
#40693=CARTESIAN_POINT('Origin',(7.49846551182189,-18.5,-4.));
#40694=CARTESIAN_POINT('',(8.69611181435176,-19.5,-4.));
#40695=CARTESIAN_POINT('Origin',(14.4702638890185,-18.5,5.42348905947456));
#40696=CARTESIAN_POINT('',(17.1190309524536,-19.5,-4.));
#40697=CARTESIAN_POINT('Origin',(18.3270808427138,-18.5,-4.));
#40698=CARTESIAN_POINT('',(13.4355384111405,-19.5,4.99999976158142));
#40699=CARTESIAN_POINT('Origin',(14.6435883014006,-18.5,4.99999976158142));
#40700=CARTESIAN_POINT('',(13.4355384111405,-19.5,4.99999976158142));
#40701=CARTESIAN_POINT('Origin',(14.7124826908112,-20.,-1.27421581745148));
#40702=CARTESIAN_POINT('',(14.7124826908112,-19.5,-1.27421581745148));
#40703=CARTESIAN_POINT('',(14.7124826908112,-20.,-1.27421581745148));
#40704=CARTESIAN_POINT('',(10.9491813182831,-19.5,-1.27421581745148));
#40705=CARTESIAN_POINT('',(14.7124826908112,-19.5,-1.27421581745148));
#40706=CARTESIAN_POINT('',(10.9491813182831,-20.,-1.27421581745148));
#40707=CARTESIAN_POINT('Origin',(15.762277841568,-20.,-4.));
#40708=CARTESIAN_POINT('',(15.762277841568,-19.5,-4.));
#40709=CARTESIAN_POINT('',(15.762277841568,-20.,-4.));
#40710=CARTESIAN_POINT('',(15.762277841568,-19.5,-4.));
#40711=CARTESIAN_POINT('Origin',(17.1190309524536,-20.,-4.));
#40712=CARTESIAN_POINT('',(17.1190309524536,-19.5,-4.));
#40713=CARTESIAN_POINT('Origin',(12.1524554491043,-20.,4.99999976158142));
#40714=CARTESIAN_POINT('',(12.1524554491043,-19.5,4.99999976158142));
#40715=CARTESIAN_POINT('Origin',(9.96077753603459,-20.,-4.));
#40716=CARTESIAN_POINT('',(9.96077753603459,-19.5,-4.));
#40717=CARTESIAN_POINT('',(9.96077753603459,-20.,-4.));
#40718=CARTESIAN_POINT('',(9.96077753603459,-19.5,-4.));
#40719=CARTESIAN_POINT('',(8.55491101741791,-19.5,-4.));
#40720=CARTESIAN_POINT('',(8.55491101741791,-20.,-4.));
#40721=CARTESIAN_POINT('',(7.05695748329163,-19.5,-4.));
#40722=CARTESIAN_POINT('',(8.55491101741791,-19.5,-4.));
#40723=CARTESIAN_POINT('',(7.05695748329163,-20.,-4.));
#40724=CARTESIAN_POINT('Origin',(10.9491813182831,-20.,-1.27421581745148));
#40725=CARTESIAN_POINT('',(10.9491813182831,-19.5,-1.27421581745148));
#40726=CARTESIAN_POINT('Origin',(12.9075713834027,-19.5,0.49999988079071));
#40727=CARTESIAN_POINT('Origin',(-23.3379939198494,-20.,-2.93792629241943));
#40728=CARTESIAN_POINT('',(-23.3379939198494,-19.5,-2.93792629241943));
#40729=CARTESIAN_POINT('',(-23.3379939198494,-20.,-2.93792629241943));
#40730=CARTESIAN_POINT('',(-17.8127557039261,-19.5,-2.93792629241943));
#40731=CARTESIAN_POINT('',(-23.3379939198494,-19.5,-2.93792629241943));
#40732=CARTESIAN_POINT('',(-17.8127557039261,-20.,-2.93792629241943));
#40733=CARTESIAN_POINT('Origin',(-23.3379939198494,-20.,0.125511646270752));
#40734=CARTESIAN_POINT('',(-23.3379939198494,-19.5,0.125511646270752));
#40735=CARTESIAN_POINT('',(-23.3379939198494,-20.,0.125511646270752));
#40736=CARTESIAN_POINT('',(-23.3379939198494,-19.5,0.125511646270752));
#40737=CARTESIAN_POINT('Origin',(-18.3591401576996,-20.,0.125511646270752));
#40738=CARTESIAN_POINT('',(-18.3591401576996,-19.5,0.125511646270752));
#40739=CARTESIAN_POINT('',(-18.3591401576996,-20.,0.125511646270752));
#40740=CARTESIAN_POINT('',(-18.3591401576996,-19.5,0.125511646270752));
#40741=CARTESIAN_POINT('Origin',(-18.3591401576996,-20.,1.18144607543945));
#40742=CARTESIAN_POINT('',(-18.3591401576996,-19.5,1.18144607543945));
#40743=CARTESIAN_POINT('',(-18.3591401576996,-20.,1.18144607543945));
#40744=CARTESIAN_POINT('',(-18.3591401576996,-19.5,1.18144607543945));
#40745=CARTESIAN_POINT('Origin',(-23.3379939198494,-20.,1.18144607543945));
#40746=CARTESIAN_POINT('',(-23.3379939198494,-19.5,1.18144607543945));
#40747=CARTESIAN_POINT('',(-23.3379939198494,-20.,1.18144607543945));
#40748=CARTESIAN_POINT('',(-23.3379939198494,-19.5,1.18144607543945));
#40749=CARTESIAN_POINT('Origin',(-23.3379939198494,-20.,3.93792605400085));
#40750=CARTESIAN_POINT('',(-23.3379939198494,-19.5,3.93792605400085));
#40751=CARTESIAN_POINT('',(-23.3379939198494,-20.,3.93792605400085));
#40752=CARTESIAN_POINT('',(-23.3379939198494,-19.5,3.93792605400085));
#40753=CARTESIAN_POINT('Origin',(-18.0214869976044,-20.,3.93792605400085));
#40754=CARTESIAN_POINT('',(-18.0214869976044,-19.5,3.93792605400085));
#40755=CARTESIAN_POINT('',(-18.0214869976044,-20.,3.93792605400085));
#40756=CARTESIAN_POINT('',(-18.0214869976044,-19.5,3.93792605400085));
#40757=CARTESIAN_POINT('Origin',(-18.0214869976044,-20.,4.99999976158142));
#40758=CARTESIAN_POINT('',(-18.0214869976044,-19.5,4.99999976158142));
#40759=CARTESIAN_POINT('',(-18.0214869976044,-20.,4.99999976158142));
#40760=CARTESIAN_POINT('',(-18.0214869976044,-19.5,4.99999976158142));
#40761=CARTESIAN_POINT('Origin',(-24.5289897173643,-20.,4.99999976158142));
#40762=CARTESIAN_POINT('',(-24.5289897173643,-19.5,4.99999976158142));
#40763=CARTESIAN_POINT('Origin',(-17.8127557039261,-20.,-4.));
#40764=CARTESIAN_POINT('',(-17.8127557039261,-19.5,-4.));
#40765=CARTESIAN_POINT('',(-17.8127557039261,-20.,-4.));
#40766=CARTESIAN_POINT('',(-17.8127557039261,-19.5,-4.));
#40767=CARTESIAN_POINT('Origin',(-17.8127557039261,-20.,-2.93792629241943));
#40768=CARTESIAN_POINT('',(-17.8127557039261,-19.5,-2.93792629241943));
#40769=CARTESIAN_POINT('Origin',(-21.1708727106452,-19.5,0.49999988079071));
#40770=CARTESIAN_POINT('Ctrl Pts',(-10.3475439548492,-20.,-3.40450191497803));
#40771=CARTESIAN_POINT('Ctrl Pts',(-10.3475439548492,-19.5,-3.40450191497803));
#40772=CARTESIAN_POINT('Ctrl Pts',(-10.7404494285583,-20.,-3.69918131828308));
#40773=CARTESIAN_POINT('Ctrl Pts',(-10.7404494285583,-19.5,-3.69918131828308));
#40774=CARTESIAN_POINT('Ctrl Pts',(-11.3328778743744,-20.,-3.84959125518799));
#40775=CARTESIAN_POINT('Ctrl Pts',(-11.3328778743744,-19.5,-3.84959125518799));
#40776=CARTESIAN_POINT('',(-10.3475439548492,-19.5,-3.40450191497803));
#40777=CARTESIAN_POINT('',(-10.3475439548492,-20.,-3.40450191497803));
#40778=CARTESIAN_POINT('',(-11.3328778743744,-19.5,-3.84959125518799));
#40779=CARTESIAN_POINT('Ctrl Pts',(-10.3475439548492,-19.5,-3.40450191497803));
#40780=CARTESIAN_POINT('Ctrl Pts',(-10.7404494285583,-19.5,-3.69918131828308));
#40781=CARTESIAN_POINT('Ctrl Pts',(-11.3328778743744,-19.5,-3.84959125518799));
#40782=CARTESIAN_POINT('',(-11.3328778743744,-20.,-3.84959125518799));
#40783=CARTESIAN_POINT('Ctrl Pts',(-9.68758463859558,-20.,-2.56650769710541));
#40784=CARTESIAN_POINT('Ctrl Pts',(-9.68758463859558,-19.5,-2.56650769710541));
#40785=CARTESIAN_POINT('Ctrl Pts',(-9.95463788509369,-20.,-3.10982251167297));
#40786=CARTESIAN_POINT('Ctrl Pts',(-9.95463788509369,-19.5,-3.10982251167297));
#40787=CARTESIAN_POINT('Ctrl Pts',(-10.3475439548492,-20.,-3.40450191497803));
#40788=CARTESIAN_POINT('Ctrl Pts',(-10.3475439548492,-19.5,-3.40450191497803));
#40789=CARTESIAN_POINT('',(-9.68758463859558,-19.5,-2.56650769710541));
#40790=CARTESIAN_POINT('',(-9.68758463859558,-20.,-2.56650769710541));
#40791=CARTESIAN_POINT('Ctrl Pts',(-9.68758463859558,-19.5,-2.56650769710541));
#40792=CARTESIAN_POINT('Ctrl Pts',(-9.95463788509369,-19.5,-3.10982251167297));
#40793=CARTESIAN_POINT('Ctrl Pts',(-10.3475439548492,-19.5,-3.40450191497803));
#40794=CARTESIAN_POINT('Ctrl Pts',(-9.42053139209747,-20.,-1.39085972309113));
#40795=CARTESIAN_POINT('Ctrl Pts',(-9.42053139209747,-19.5,-1.39085972309113));
#40796=CARTESIAN_POINT('Ctrl Pts',(-9.42053139209747,-20.,-2.02319228649139));
#40797=CARTESIAN_POINT('Ctrl Pts',(-9.42053139209747,-19.5,-2.02319228649139));
#40798=CARTESIAN_POINT('Ctrl Pts',(-9.68758463859558,-20.,-2.56650769710541));
#40799=CARTESIAN_POINT('Ctrl Pts',(-9.68758463859558,-19.5,-2.56650769710541));
#40800=CARTESIAN_POINT('',(-9.42053139209747,-19.5,-1.39085972309113));
#40801=CARTESIAN_POINT('',(-9.42053139209747,-20.,-1.39085972309113));
#40802=CARTESIAN_POINT('Ctrl Pts',(-9.42053139209747,-19.5,-1.39085972309113));
#40803=CARTESIAN_POINT('Ctrl Pts',(-9.42053139209747,-19.5,-2.02319228649139));
#40804=CARTESIAN_POINT('Ctrl Pts',(-9.68758463859558,-19.5,-2.56650769710541));
#40805=CARTESIAN_POINT('Ctrl Pts',(-9.85948085784912,-20.,-0.0279673337936404));
#40806=CARTESIAN_POINT('Ctrl Pts',(-9.85948085784912,-19.5,-0.0279673337936404));
#40807=CARTESIAN_POINT('Ctrl Pts',(-9.42053139209747,-20.,-0.605048179626465));
#40808=CARTESIAN_POINT('Ctrl Pts',(-9.42053139209747,-19.5,-0.605048179626465));
#40809=CARTESIAN_POINT('Ctrl Pts',(-9.42053139209747,-20.,-1.39085972309113));
#40810=CARTESIAN_POINT('Ctrl Pts',(-9.42053139209747,-19.5,-1.39085972309113));
#40811=CARTESIAN_POINT('',(-9.85948085784912,-19.5,-0.0279673337936404));
#40812=CARTESIAN_POINT('',(-9.85948085784912,-20.,-0.0279673337936404));
#40813=CARTESIAN_POINT('Ctrl Pts',(-9.85948085784912,-19.5,-0.0279673337936404));
#40814=CARTESIAN_POINT('Ctrl Pts',(-9.42053139209747,-19.5,-0.605048179626465));
#40815=CARTESIAN_POINT('Ctrl Pts',(-9.42053139209747,-19.5,-1.39085972309113));
#40816=CARTESIAN_POINT('Ctrl Pts',(-11.1149382591248,-20.,0.788540005683899));
#40817=CARTESIAN_POINT('Ctrl Pts',(-11.1149382591248,-19.5,0.788540005683899));
#40818=CARTESIAN_POINT('Ctrl Pts',(-10.2984303236008,-20.,0.549112915992737));
#40819=CARTESIAN_POINT('Ctrl Pts',(-10.2984303236008,-19.5,0.549112915992737));
#40820=CARTESIAN_POINT('Ctrl Pts',(-9.85948085784912,-20.,-0.0279673337936404));
#40821=CARTESIAN_POINT('Ctrl Pts',(-9.85948085784912,-19.5,-0.0279673337936404));
#40822=CARTESIAN_POINT('',(-11.1149382591248,-19.5,0.788540005683899));
#40823=CARTESIAN_POINT('',(-11.1149382591248,-20.,0.788540005683899));
#40824=CARTESIAN_POINT('Ctrl Pts',(-11.1149382591248,-19.5,0.788540005683899));
#40825=CARTESIAN_POINT('Ctrl Pts',(-10.2984303236008,-19.5,0.549112915992737));
#40826=CARTESIAN_POINT('Ctrl Pts',(-9.85948085784912,-19.5,-0.0279673337936404));
#40827=CARTESIAN_POINT('Ctrl Pts',(-10.1695084571838,-20.,1.6111866235733));
#40828=CARTESIAN_POINT('Ctrl Pts',(-10.1695084571838,-19.5,1.6111866235733));
#40829=CARTESIAN_POINT('Ctrl Pts',(-10.482605099678,-20.,1.1016366481781));
#40830=CARTESIAN_POINT('Ctrl Pts',(-10.482605099678,-19.5,1.1016366481781));
#40831=CARTESIAN_POINT('Ctrl Pts',(-11.1149382591248,-20.,0.788540005683899));
#40832=CARTESIAN_POINT('Ctrl Pts',(-11.1149382591248,-19.5,0.788540005683899));
#40833=CARTESIAN_POINT('',(-10.1695084571838,-19.5,1.6111866235733));
#40834=CARTESIAN_POINT('',(-10.1695084571838,-20.,1.6111866235733));
#40835=CARTESIAN_POINT('Ctrl Pts',(-10.1695084571838,-19.5,1.6111866235733));
#40836=CARTESIAN_POINT('Ctrl Pts',(-10.482605099678,-19.5,1.1016366481781));
#40837=CARTESIAN_POINT('Ctrl Pts',(-11.1149382591248,-19.5,0.788540005683899));
#40838=CARTESIAN_POINT('Ctrl Pts',(-9.85641181468963,-20.,2.69781684875488));
#40839=CARTESIAN_POINT('Ctrl Pts',(-9.85641181468963,-19.5,2.69781684875488));
#40840=CARTESIAN_POINT('Ctrl Pts',(-9.85641181468963,-20.,2.12073659896851));
#40841=CARTESIAN_POINT('Ctrl Pts',(-9.85641181468963,-19.5,2.12073659896851));
#40842=CARTESIAN_POINT('Ctrl Pts',(-10.1695084571838,-20.,1.6111866235733));
#40843=CARTESIAN_POINT('Ctrl Pts',(-10.1695084571838,-19.5,1.6111866235733));
#40844=CARTESIAN_POINT('',(-9.85641181468963,-19.5,2.69781684875488));
#40845=CARTESIAN_POINT('',(-9.85641181468963,-20.,2.69781684875488));
#40846=CARTESIAN_POINT('Ctrl Pts',(-9.85641181468963,-19.5,2.69781684875488));
#40847=CARTESIAN_POINT('Ctrl Pts',(-9.85641181468963,-19.5,2.12073659896851));
#40848=CARTESIAN_POINT('Ctrl Pts',(-10.1695084571838,-19.5,1.6111866235733));
#40849=CARTESIAN_POINT('Ctrl Pts',(-10.2094125747681,-20.,3.8857433795929));
#40850=CARTESIAN_POINT('Ctrl Pts',(-10.2094125747681,-19.5,3.8857433795929));
#40851=CARTESIAN_POINT('Ctrl Pts',(-9.85641181468963,-20.,3.31787145137787));
#40852=CARTESIAN_POINT('Ctrl Pts',(-9.85641181468963,-19.5,3.31787145137787));
#40853=CARTESIAN_POINT('Ctrl Pts',(-9.85641181468963,-20.,2.69781684875488));
#40854=CARTESIAN_POINT('Ctrl Pts',(-9.85641181468963,-19.5,2.69781684875488));
#40855=CARTESIAN_POINT('',(-10.2094125747681,-19.5,3.8857433795929));
#40856=CARTESIAN_POINT('',(-10.2094125747681,-20.,3.8857433795929));
#40857=CARTESIAN_POINT('Ctrl Pts',(-10.2094125747681,-19.5,3.8857433795929));
#40858=CARTESIAN_POINT('Ctrl Pts',(-9.85641181468963,-19.5,3.31787145137787));
#40859=CARTESIAN_POINT('Ctrl Pts',(-9.85641181468963,-19.5,2.69781684875488));
#40860=CARTESIAN_POINT('Ctrl Pts',(-11.1855381727219,-20.,4.72680723667145));
#40861=CARTESIAN_POINT('Ctrl Pts',(-11.1855381727219,-19.5,4.72680723667145));
#40862=CARTESIAN_POINT('Ctrl Pts',(-10.5624139308929,-20.,4.45361471176147));
#40863=CARTESIAN_POINT('Ctrl Pts',(-10.5624139308929,-19.5,4.45361471176147));
#40864=CARTESIAN_POINT('Ctrl Pts',(-10.2094125747681,-20.,3.8857433795929));
#40865=CARTESIAN_POINT('Ctrl Pts',(-10.2094125747681,-19.5,3.8857433795929));
#40866=CARTESIAN_POINT('',(-11.1855381727219,-19.5,4.72680723667145));
#40867=CARTESIAN_POINT('',(-11.1855381727219,-20.,4.72680723667145));
#40868=CARTESIAN_POINT('Ctrl Pts',(-11.1855381727219,-19.5,4.72680723667145));
#40869=CARTESIAN_POINT('Ctrl Pts',(-10.5624139308929,-19.5,4.45361471176147));
#40870=CARTESIAN_POINT('Ctrl Pts',(-10.2094125747681,-19.5,3.8857433795929));
#40871=CARTESIAN_POINT('Ctrl Pts',(-12.8400406241417,-20.,4.99999976158142));
#40872=CARTESIAN_POINT('Ctrl Pts',(-12.8400406241417,-19.5,4.99999976158142));
#40873=CARTESIAN_POINT('Ctrl Pts',(-11.8086624145508,-20.,4.99999976158142));
#40874=CARTESIAN_POINT('Ctrl Pts',(-11.8086624145508,-19.5,4.99999976158142));
#40875=CARTESIAN_POINT('Ctrl Pts',(-11.1855381727219,-20.,4.72680723667145));
#40876=CARTESIAN_POINT('Ctrl Pts',(-11.1855381727219,-19.5,4.72680723667145));
#40877=CARTESIAN_POINT('',(-12.8400406241417,-19.5,4.99999976158142));
#40878=CARTESIAN_POINT('',(-12.8400406241417,-20.,4.99999976158142));
#40879=CARTESIAN_POINT('Ctrl Pts',(-12.8400406241417,-19.5,4.99999976158142));
#40880=CARTESIAN_POINT('Ctrl Pts',(-11.8086624145508,-19.5,4.99999976158142));
#40881=CARTESIAN_POINT('Ctrl Pts',(-11.1855381727219,-19.5,4.72680723667145));
#40882=CARTESIAN_POINT('Origin',(-16.2165751308203,-20.,4.99999976158142));
#40883=CARTESIAN_POINT('',(-16.2165751308203,-19.5,4.99999976158142));
#40884=CARTESIAN_POINT('Origin',(-12.7847883105278,-20.,-4.));
#40885=CARTESIAN_POINT('',(-12.7847883105278,-19.5,-4.));
#40886=CARTESIAN_POINT('',(-12.7847883105278,-20.,-4.));
#40887=CARTESIAN_POINT('',(-12.7847883105278,-19.5,-4.));
#40888=CARTESIAN_POINT('Ctrl Pts',(-11.3328778743744,-20.,-3.84959125518799));
#40889=CARTESIAN_POINT('Ctrl Pts',(-11.3328778743744,-19.5,-3.84959125518799));
#40890=CARTESIAN_POINT('Ctrl Pts',(-11.9253063201904,-20.,-4.));
#40891=CARTESIAN_POINT('Ctrl Pts',(-11.9253063201904,-19.5,-4.));
#40892=CARTESIAN_POINT('Ctrl Pts',(-12.7847883105278,-20.,-4.));
#40893=CARTESIAN_POINT('Ctrl Pts',(-12.7847883105278,-19.5,-4.));
#40894=CARTESIAN_POINT('Ctrl Pts',(-11.3328778743744,-19.5,-3.84959125518799));
#40895=CARTESIAN_POINT('Ctrl Pts',(-11.9253063201904,-19.5,-4.));
#40896=CARTESIAN_POINT('Ctrl Pts',(-12.7847883105278,-19.5,-4.));
#40897=CARTESIAN_POINT('Origin',(-12.8185532614589,-19.5,0.49999988079071));
#40898=CARTESIAN_POINT('Ctrl Pts',(-4.34959053993225,-20.,-4.15347838401794));
#40899=CARTESIAN_POINT('Ctrl Pts',(-4.34959053993225,-19.5,-4.15347838401794));
#40900=CARTESIAN_POINT('Ctrl Pts',(-5.57128190994263,-20.,-4.15347838401794));
#40901=CARTESIAN_POINT('Ctrl Pts',(-5.57128190994263,-19.5,-4.15347838401794));
#40902=CARTESIAN_POINT('Ctrl Pts',(-6.39699831604958,-20.,-3.79740738868713));
#40903=CARTESIAN_POINT('Ctrl Pts',(-6.39699831604958,-19.5,-3.79740738868713));
#40904=CARTESIAN_POINT('',(-4.34959053993225,-19.5,-4.15347838401794));
#40905=CARTESIAN_POINT('',(-4.34959053993225,-20.,-4.15347838401794));
#40906=CARTESIAN_POINT('',(-6.39699831604958,-19.5,-3.79740738868713));
#40907=CARTESIAN_POINT('Ctrl Pts',(-4.34959053993225,-19.5,-4.15347838401794));
#40908=CARTESIAN_POINT('Ctrl Pts',(-5.57128190994263,-19.5,-4.15347838401794));
#40909=CARTESIAN_POINT('Ctrl Pts',(-6.39699831604958,-19.5,-3.79740738868713));
#40910=CARTESIAN_POINT('',(-6.39699831604958,-20.,-3.79740738868713));
#40911=CARTESIAN_POINT('Ctrl Pts',(-2.61527955532074,-20.,-3.80047702789307));
#40912=CARTESIAN_POINT('Ctrl Pts',(-2.61527955532074,-19.5,-3.80047702789307));
#40913=CARTESIAN_POINT('Ctrl Pts',(-3.38574349880219,-20.,-4.15347838401794));
#40914=CARTESIAN_POINT('Ctrl Pts',(-3.38574349880219,-19.5,-4.15347838401794));
#40915=CARTESIAN_POINT('Ctrl Pts',(-4.34959053993225,-20.,-4.15347838401794));
#40916=CARTESIAN_POINT('Ctrl Pts',(-4.34959053993225,-19.5,-4.15347838401794));
#40917=CARTESIAN_POINT('',(-2.61527955532074,-19.5,-3.80047702789307));
#40918=CARTESIAN_POINT('',(-2.61527955532074,-20.,-3.80047702789307));
#40919=CARTESIAN_POINT('Ctrl Pts',(-2.61527955532074,-19.5,-3.80047702789307));
#40920=CARTESIAN_POINT('Ctrl Pts',(-3.38574349880219,-19.5,-4.15347838401794));
#40921=CARTESIAN_POINT('Ctrl Pts',(-4.34959053993225,-19.5,-4.15347838401794));
#40922=CARTESIAN_POINT('Ctrl Pts',(-1.43349230289459,-20.,-2.81207346916199));
#40923=CARTESIAN_POINT('Ctrl Pts',(-1.43349230289459,-19.5,-2.81207346916199));
#40924=CARTESIAN_POINT('Ctrl Pts',(-1.84481561183929,-20.,-3.44747567176819));
#40925=CARTESIAN_POINT('Ctrl Pts',(-1.84481561183929,-19.5,-3.44747567176819));
#40926=CARTESIAN_POINT('Ctrl Pts',(-2.61527955532074,-20.,-3.80047702789307));
#40927=CARTESIAN_POINT('Ctrl Pts',(-2.61527955532074,-19.5,-3.80047702789307));
#40928=CARTESIAN_POINT('',(-1.43349230289459,-19.5,-2.81207346916199));
#40929=CARTESIAN_POINT('',(-1.43349230289459,-20.,-2.81207346916199));
#40930=CARTESIAN_POINT('Ctrl Pts',(-1.43349230289459,-19.5,-2.81207346916199));
#40931=CARTESIAN_POINT('Ctrl Pts',(-1.84481561183929,-19.5,-3.44747567176819));
#40932=CARTESIAN_POINT('Ctrl Pts',(-2.61527955532074,-19.5,-3.80047702789307));
#40933=CARTESIAN_POINT('Ctrl Pts',(-1.02216899394989,-20.,-1.4583899974823));
#40934=CARTESIAN_POINT('Ctrl Pts',(-1.02216899394989,-19.5,-1.4583899974823));
#40935=CARTESIAN_POINT('Ctrl Pts',(-1.02216899394989,-20.,-2.17667126655579));
#40936=CARTESIAN_POINT('Ctrl Pts',(-1.02216899394989,-19.5,-2.17667126655579));
#40937=CARTESIAN_POINT('Ctrl Pts',(-1.43349230289459,-20.,-2.81207346916199));
#40938=CARTESIAN_POINT('Ctrl Pts',(-1.43349230289459,-19.5,-2.81207346916199));
#40939=CARTESIAN_POINT('',(-1.02216899394989,-19.5,-1.4583899974823));
#40940=CARTESIAN_POINT('',(-1.02216899394989,-20.,-1.4583899974823));
#40941=CARTESIAN_POINT('Ctrl Pts',(-1.02216899394989,-19.5,-1.4583899974823));
#40942=CARTESIAN_POINT('Ctrl Pts',(-1.02216899394989,-19.5,-2.17667126655579));
#40943=CARTESIAN_POINT('Ctrl Pts',(-1.43349230289459,-19.5,-2.81207346916199));
#40944=CARTESIAN_POINT('Ctrl Pts',(-1.39665722846985,-20.,-0.1783766746521));
#40945=CARTESIAN_POINT('Ctrl Pts',(-1.39665722846985,-19.5,-0.1783766746521));
#40946=CARTESIAN_POINT('Ctrl Pts',(-1.02216899394989,-20.,-0.733970642089844));
#40947=CARTESIAN_POINT('Ctrl Pts',(-1.02216899394989,-19.5,-0.733970642089844));
#40948=CARTESIAN_POINT('Ctrl Pts',(-1.02216899394989,-20.,-1.4583899974823));
#40949=CARTESIAN_POINT('Ctrl Pts',(-1.02216899394989,-19.5,-1.4583899974823));
#40950=CARTESIAN_POINT('',(-1.39665722846985,-19.5,-0.1783766746521));
#40951=CARTESIAN_POINT('',(-1.39665722846985,-20.,-0.1783766746521));
#40952=CARTESIAN_POINT('Ctrl Pts',(-1.39665722846985,-19.5,-0.1783766746521));
#40953=CARTESIAN_POINT('Ctrl Pts',(-1.02216899394989,-19.5,-0.733970642089844));
#40954=CARTESIAN_POINT('Ctrl Pts',(-1.02216899394989,-19.5,-1.4583899974823));
#40955=CARTESIAN_POINT('Ctrl Pts',(-2.55695760250092,-20.,0.739426374435425));
#40956=CARTESIAN_POINT('Ctrl Pts',(-2.55695760250092,-19.5,0.739426374435425));
#40957=CARTESIAN_POINT('Ctrl Pts',(-1.77114546298981,-20.,0.377216696739197));
#40958=CARTESIAN_POINT('Ctrl Pts',(-1.77114546298981,-19.5,0.377216696739197));
#40959=CARTESIAN_POINT('Ctrl Pts',(-1.39665722846985,-20.,-0.1783766746521));
#40960=CARTESIAN_POINT('Ctrl Pts',(-1.39665722846985,-19.5,-0.1783766746521));
#40961=CARTESIAN_POINT('',(-2.55695760250092,-19.5,0.739426374435425));
#40962=CARTESIAN_POINT('',(-2.55695760250092,-20.,0.739426374435425));
#40963=CARTESIAN_POINT('Ctrl Pts',(-2.55695760250092,-19.5,0.739426374435425));
#40964=CARTESIAN_POINT('Ctrl Pts',(-1.77114546298981,-19.5,0.377216696739197));
#40965=CARTESIAN_POINT('Ctrl Pts',(-1.39665722846985,-19.5,-0.1783766746521));
#40966=CARTESIAN_POINT('Ctrl Pts',(-4.54911291599274,-20.,1.31343758106232));
#40967=CARTESIAN_POINT('Ctrl Pts',(-4.54911291599274,-19.5,1.31343758106232));
#40968=CARTESIAN_POINT('Ctrl Pts',(-3.09720277786255,-20.,0.984992742538452));
#40969=CARTESIAN_POINT('Ctrl Pts',(-3.09720277786255,-19.5,0.984992742538452));
#40970=CARTESIAN_POINT('Ctrl Pts',(-2.55695760250092,-20.,0.739426374435425));
#40971=CARTESIAN_POINT('Ctrl Pts',(-2.55695760250092,-19.5,0.739426374435425));
#40972=CARTESIAN_POINT('',(-4.54911291599274,-19.5,1.31343758106232));
#40973=CARTESIAN_POINT('',(-4.54911291599274,-20.,1.31343758106232));
#40974=CARTESIAN_POINT('Ctrl Pts',(-4.54911291599274,-19.5,1.31343758106232));
#40975=CARTESIAN_POINT('Ctrl Pts',(-3.09720277786255,-19.5,0.984992742538452));
#40976=CARTESIAN_POINT('Ctrl Pts',(-2.55695760250092,-19.5,0.739426374435425));
#40977=CARTESIAN_POINT('Ctrl Pts',(-6.34481549263,-20.,1.95497906208038));
#40978=CARTESIAN_POINT('Ctrl Pts',(-6.34481549263,-19.5,1.95497906208038));
#40979=CARTESIAN_POINT('Ctrl Pts',(-6.00102305412292,-20.,1.64188241958618));
#40980=CARTESIAN_POINT('Ctrl Pts',(-6.00102305412292,-19.5,1.64188241958618));
#40981=CARTESIAN_POINT('Ctrl Pts',(-4.54911291599274,-20.,1.31343758106232));
#40982=CARTESIAN_POINT('Ctrl Pts',(-4.54911291599274,-19.5,1.31343758106232));
#40983=CARTESIAN_POINT('',(-6.34481549263,-19.5,1.95497906208038));
#40984=CARTESIAN_POINT('',(-6.34481549263,-20.,1.95497906208038));
#40985=CARTESIAN_POINT('Ctrl Pts',(-6.34481549263,-19.5,1.95497906208038));
#40986=CARTESIAN_POINT('Ctrl Pts',(-6.00102305412292,-19.5,1.64188241958618));
#40987=CARTESIAN_POINT('Ctrl Pts',(-4.54911291599274,-19.5,1.31343758106232));
#40988=CARTESIAN_POINT('Ctrl Pts',(-6.69474720954895,-20.,2.75306916236877));
#40989=CARTESIAN_POINT('Ctrl Pts',(-6.69474720954895,-19.5,2.75306916236877));
#40990=CARTESIAN_POINT('Ctrl Pts',(-6.69474720954895,-20.,2.26807570457458));
#40991=CARTESIAN_POINT('Ctrl Pts',(-6.69474720954895,-19.5,2.26807570457458));
#40992=CARTESIAN_POINT('Ctrl Pts',(-6.34481549263,-20.,1.95497906208038));
#40993=CARTESIAN_POINT('Ctrl Pts',(-6.34481549263,-19.5,1.95497906208038));
#40994=CARTESIAN_POINT('',(-6.69474720954895,-19.5,2.75306916236877));
#40995=CARTESIAN_POINT('',(-6.69474720954895,-20.,2.75306916236877));
#40996=CARTESIAN_POINT('Ctrl Pts',(-6.69474720954895,-19.5,2.75306916236877));
#40997=CARTESIAN_POINT('Ctrl Pts',(-6.69474720954895,-19.5,2.26807570457458));
#40998=CARTESIAN_POINT('Ctrl Pts',(-6.34481549263,-19.5,1.95497906208038));
#40999=CARTESIAN_POINT('Ctrl Pts',(-6.20054543018341,-20.,3.70770728588104));
#41000=CARTESIAN_POINT('Ctrl Pts',(-6.20054543018341,-19.5,3.70770728588104));
#41001=CARTESIAN_POINT('Ctrl Pts',(-6.69474720954895,-20.,3.311732172966));
#41002=CARTESIAN_POINT('Ctrl Pts',(-6.69474720954895,-19.5,3.311732172966));
#41003=CARTESIAN_POINT('Ctrl Pts',(-6.69474720954895,-20.,2.75306916236877));
#41004=CARTESIAN_POINT('Ctrl Pts',(-6.69474720954895,-19.5,2.75306916236877));
#41005=CARTESIAN_POINT('',(-6.20054543018341,-19.5,3.70770728588104));
#41006=CARTESIAN_POINT('',(-6.20054543018341,-20.,3.70770728588104));
#41007=CARTESIAN_POINT('Ctrl Pts',(-6.20054543018341,-19.5,3.70770728588104));
#41008=CARTESIAN_POINT('Ctrl Pts',(-6.69474720954895,-19.5,3.311732172966));
#41009=CARTESIAN_POINT('Ctrl Pts',(-6.69474720954895,-19.5,2.75306916236877));
#41010=CARTESIAN_POINT('Ctrl Pts',(-4.62585210800171,-20.,4.10368299484253));
#41011=CARTESIAN_POINT('Ctrl Pts',(-4.62585210800171,-19.5,4.10368299484253));
#41012=CARTESIAN_POINT('Ctrl Pts',(-5.70634365081787,-20.,4.10368299484253));
#41013=CARTESIAN_POINT('Ctrl Pts',(-5.70634365081787,-19.5,4.10368299484253));
#41014=CARTESIAN_POINT('Ctrl Pts',(-6.20054543018341,-20.,3.70770728588104));
#41015=CARTESIAN_POINT('Ctrl Pts',(-6.20054543018341,-19.5,3.70770728588104));
#41016=CARTESIAN_POINT('',(-4.62585210800171,-19.5,4.10368299484253));
#41017=CARTESIAN_POINT('',(-4.62585210800171,-20.,4.10368299484253));
#41018=CARTESIAN_POINT('Ctrl Pts',(-4.62585210800171,-19.5,4.10368299484253));
#41019=CARTESIAN_POINT('Ctrl Pts',(-5.70634365081787,-19.5,4.10368299484253));
#41020=CARTESIAN_POINT('Ctrl Pts',(-6.20054543018341,-19.5,3.70770728588104));
#41021=CARTESIAN_POINT('Ctrl Pts',(-3.05729866027832,-20.,3.66780316829681));
#41022=CARTESIAN_POINT('Ctrl Pts',(-3.05729866027832,-19.5,3.66780316829681));
#41023=CARTESIAN_POINT('Ctrl Pts',(-3.5883355140686,-20.,4.10368299484253));
#41024=CARTESIAN_POINT('Ctrl Pts',(-3.5883355140686,-19.5,4.10368299484253));
#41025=CARTESIAN_POINT('Ctrl Pts',(-4.62585210800171,-20.,4.10368299484253));
#41026=CARTESIAN_POINT('Ctrl Pts',(-4.62585210800171,-19.5,4.10368299484253));
#41027=CARTESIAN_POINT('',(-3.05729866027832,-19.5,3.66780316829681));
#41028=CARTESIAN_POINT('',(-3.05729866027832,-20.,3.66780316829681));
#41029=CARTESIAN_POINT('Ctrl Pts',(-3.05729866027832,-19.5,3.66780316829681));
#41030=CARTESIAN_POINT('Ctrl Pts',(-3.5883355140686,-19.5,4.10368299484253));
#41031=CARTESIAN_POINT('Ctrl Pts',(-4.62585210800171,-19.5,4.10368299484253));
#41032=CARTESIAN_POINT('Ctrl Pts',(-2.4341744184494,-20.,2.37858092784882));
#41033=CARTESIAN_POINT('Ctrl Pts',(-2.4341744184494,-19.5,2.37858092784882));
#41034=CARTESIAN_POINT('Ctrl Pts',(-2.52626180648804,-20.,3.2319233417511));
#41035=CARTESIAN_POINT('Ctrl Pts',(-2.52626180648804,-19.5,3.2319233417511));
#41036=CARTESIAN_POINT('Ctrl Pts',(-3.05729866027832,-20.,3.66780316829681));
#41037=CARTESIAN_POINT('Ctrl Pts',(-3.05729866027832,-19.5,3.66780316829681));
#41038=CARTESIAN_POINT('',(-2.4341744184494,-19.5,2.37858092784882));
#41039=CARTESIAN_POINT('',(-2.4341744184494,-20.,2.37858092784882));
#41040=CARTESIAN_POINT('Ctrl Pts',(-2.4341744184494,-19.5,2.37858092784882));
#41041=CARTESIAN_POINT('Ctrl Pts',(-2.52626180648804,-19.5,3.2319233417511));
#41042=CARTESIAN_POINT('Ctrl Pts',(-3.05729866027832,-19.5,3.66780316829681));
#41043=CARTESIAN_POINT('Origin',(-1.29229187965393,-20.,2.46452903747559));
#41044=CARTESIAN_POINT('',(-1.29229187965393,-19.5,2.46452903747559));
#41045=CARTESIAN_POINT('',(-1.29229187965393,-20.,2.46452903747559));
#41046=CARTESIAN_POINT('',(-1.29229187965393,-19.5,2.46452903747559));
#41047=CARTESIAN_POINT('Ctrl Pts',(-1.73431098461151,-20.,3.88267314434052));
#41048=CARTESIAN_POINT('Ctrl Pts',(-1.73431098461151,-19.5,3.88267314434052));
#41049=CARTESIAN_POINT('Ctrl Pts',(-1.32298767566681,-20.,3.25647985935211));
#41050=CARTESIAN_POINT('Ctrl Pts',(-1.32298767566681,-19.5,3.25647985935211));
#41051=CARTESIAN_POINT('Ctrl Pts',(-1.29229187965393,-20.,2.46452903747559));
#41052=CARTESIAN_POINT('Ctrl Pts',(-1.29229187965393,-19.5,2.46452903747559));
#41053=CARTESIAN_POINT('',(-1.73431098461151,-19.5,3.88267314434052));
#41054=CARTESIAN_POINT('',(-1.73431098461151,-20.,3.88267314434052));
#41055=CARTESIAN_POINT('Ctrl Pts',(-1.73431098461151,-19.5,3.88267314434052));
#41056=CARTESIAN_POINT('Ctrl Pts',(-1.32298767566681,-19.5,3.25647985935211));
#41057=CARTESIAN_POINT('Ctrl Pts',(-1.29229187965393,-19.5,2.46452903747559));
#41058=CARTESIAN_POINT('Ctrl Pts',(-2.90995895862579,-20.,4.83117258548737));
#41059=CARTESIAN_POINT('Ctrl Pts',(-2.90995895862579,-19.5,4.83117258548737));
#41060=CARTESIAN_POINT('Ctrl Pts',(-2.14563429355621,-20.,4.50886702537537));
#41061=CARTESIAN_POINT('Ctrl Pts',(-2.14563429355621,-19.5,4.50886702537537));
#41062=CARTESIAN_POINT('Ctrl Pts',(-1.73431098461151,-20.,3.88267314434052));
#41063=CARTESIAN_POINT('Ctrl Pts',(-1.73431098461151,-19.5,3.88267314434052));
#41064=CARTESIAN_POINT('',(-2.90995895862579,-19.5,4.83117258548737));
#41065=CARTESIAN_POINT('',(-2.90995895862579,-20.,4.83117258548737));
#41066=CARTESIAN_POINT('Ctrl Pts',(-2.90995895862579,-19.5,4.83117258548737));
#41067=CARTESIAN_POINT('Ctrl Pts',(-2.14563429355621,-19.5,4.50886702537537));
#41068=CARTESIAN_POINT('Ctrl Pts',(-1.73431098461151,-19.5,3.88267314434052));
#41069=CARTESIAN_POINT('Ctrl Pts',(-4.67496573925018,-20.,5.15347814559937));
#41070=CARTESIAN_POINT('Ctrl Pts',(-4.67496573925018,-19.5,5.15347814559937));
#41071=CARTESIAN_POINT('Ctrl Pts',(-3.67428362369537,-20.,5.15347814559937));
#41072=CARTESIAN_POINT('Ctrl Pts',(-3.67428362369537,-19.5,5.15347814559937));
#41073=CARTESIAN_POINT('Ctrl Pts',(-2.90995895862579,-20.,4.83117258548737));
#41074=CARTESIAN_POINT('Ctrl Pts',(-2.90995895862579,-19.5,4.83117258548737));
#41075=CARTESIAN_POINT('',(-4.67496573925018,-19.5,5.15347814559937));
#41076=CARTESIAN_POINT('',(-4.67496573925018,-20.,5.15347814559937));
#41077=CARTESIAN_POINT('Ctrl Pts',(-4.67496573925018,-19.5,5.15347814559937));
#41078=CARTESIAN_POINT('Ctrl Pts',(-3.67428362369537,-19.5,5.15347814559937));
#41079=CARTESIAN_POINT('Ctrl Pts',(-2.90995895862579,-19.5,4.83117258548737));
#41080=CARTESIAN_POINT('Ctrl Pts',(-6.32639795541763,-20.,4.84652078151703));
#41081=CARTESIAN_POINT('Ctrl Pts',(-6.32639795541763,-19.5,4.84652078151703));
#41082=CARTESIAN_POINT('Ctrl Pts',(-5.58356046676636,-20.,5.15347814559937));
#41083=CARTESIAN_POINT('Ctrl Pts',(-5.58356046676636,-19.5,5.15347814559937));
#41084=CARTESIAN_POINT('Ctrl Pts',(-4.67496573925018,-20.,5.15347814559937));
#41085=CARTESIAN_POINT('Ctrl Pts',(-4.67496573925018,-19.5,5.15347814559937));
#41086=CARTESIAN_POINT('',(-6.32639795541763,-19.5,4.84652078151703));
#41087=CARTESIAN_POINT('',(-6.32639795541763,-20.,4.84652078151703));
#41088=CARTESIAN_POINT('Ctrl Pts',(-6.32639795541763,-19.5,4.84652078151703));
#41089=CARTESIAN_POINT('Ctrl Pts',(-5.58356046676636,-19.5,5.15347814559937));
#41090=CARTESIAN_POINT('Ctrl Pts',(-4.67496573925018,-19.5,5.15347814559937));
#41091=CARTESIAN_POINT('Ctrl Pts',(-7.4560022354126,-20.,3.9471343755722));
#41092=CARTESIAN_POINT('Ctrl Pts',(-7.4560022354126,-19.5,3.9471343755722));
#41093=CARTESIAN_POINT('Ctrl Pts',(-7.06923559308052,-20.,4.53956282138824));
#41094=CARTESIAN_POINT('Ctrl Pts',(-7.06923559308052,-19.5,4.53956282138824));
#41095=CARTESIAN_POINT('Ctrl Pts',(-6.32639795541763,-20.,4.84652078151703));
#41096=CARTESIAN_POINT('Ctrl Pts',(-6.32639795541763,-19.5,4.84652078151703));
#41097=CARTESIAN_POINT('',(-7.4560022354126,-19.5,3.9471343755722));
#41098=CARTESIAN_POINT('',(-7.4560022354126,-20.,3.9471343755722));
#41099=CARTESIAN_POINT('Ctrl Pts',(-7.4560022354126,-19.5,3.9471343755722));
#41100=CARTESIAN_POINT('Ctrl Pts',(-7.06923559308052,-19.5,4.53956282138824));
#41101=CARTESIAN_POINT('Ctrl Pts',(-6.32639795541763,-19.5,4.84652078151703));
#41102=CARTESIAN_POINT('Ctrl Pts',(-7.84276902675629,-20.,2.67326033115387));
#41103=CARTESIAN_POINT('Ctrl Pts',(-7.84276902675629,-19.5,2.67326033115387));
#41104=CARTESIAN_POINT('Ctrl Pts',(-7.84276902675629,-20.,3.35470592975616));
#41105=CARTESIAN_POINT('Ctrl Pts',(-7.84276902675629,-19.5,3.35470592975616));
#41106=CARTESIAN_POINT('Ctrl Pts',(-7.4560022354126,-20.,3.9471343755722));
#41107=CARTESIAN_POINT('Ctrl Pts',(-7.4560022354126,-19.5,3.9471343755722));
#41108=CARTESIAN_POINT('',(-7.84276902675629,-19.5,2.67326033115387));
#41109=CARTESIAN_POINT('',(-7.84276902675629,-20.,2.67326033115387));
#41110=CARTESIAN_POINT('Ctrl Pts',(-7.84276902675629,-19.5,2.67326033115387));
#41111=CARTESIAN_POINT('Ctrl Pts',(-7.84276902675629,-19.5,3.35470592975616));
#41112=CARTESIAN_POINT('Ctrl Pts',(-7.4560022354126,-19.5,3.9471343755722));
#41113=CARTESIAN_POINT('Ctrl Pts',(-7.52660259604454,-20.,1.55286467075348));
#41114=CARTESIAN_POINT('Ctrl Pts',(-7.52660259604454,-19.5,1.55286467075348));
#41115=CARTESIAN_POINT('Ctrl Pts',(-7.84276902675629,-20.,2.05320572853088));
#41116=CARTESIAN_POINT('Ctrl Pts',(-7.84276902675629,-19.5,2.05320572853088));
#41117=CARTESIAN_POINT('Ctrl Pts',(-7.84276902675629,-20.,2.67326033115387));
#41118=CARTESIAN_POINT('Ctrl Pts',(-7.84276902675629,-19.5,2.67326033115387));
#41119=CARTESIAN_POINT('',(-7.52660259604454,-19.5,1.55286467075348));
#41120=CARTESIAN_POINT('',(-7.52660259604454,-20.,1.55286467075348));
#41121=CARTESIAN_POINT('Ctrl Pts',(-7.52660259604454,-19.5,1.55286467075348));
#41122=CARTESIAN_POINT('Ctrl Pts',(-7.84276902675629,-19.5,2.05320572853088));
#41123=CARTESIAN_POINT('Ctrl Pts',(-7.84276902675629,-19.5,2.67326033115387));
#41124=CARTESIAN_POINT('Ctrl Pts',(-6.5658250451088,-20.,0.714870452880859));
#41125=CARTESIAN_POINT('Ctrl Pts',(-6.5658250451088,-19.5,0.714870452880859));
#41126=CARTESIAN_POINT('Ctrl Pts',(-7.21043616533279,-20.,1.05252361297607));
#41127=CARTESIAN_POINT('Ctrl Pts',(-7.21043616533279,-19.5,1.05252361297607));
#41128=CARTESIAN_POINT('Ctrl Pts',(-7.52660259604454,-20.,1.55286467075348));
#41129=CARTESIAN_POINT('Ctrl Pts',(-7.52660259604454,-19.5,1.55286467075348));
#41130=CARTESIAN_POINT('',(-6.5658250451088,-19.5,0.714870452880859));
#41131=CARTESIAN_POINT('',(-6.5658250451088,-20.,0.714870452880859));
#41132=CARTESIAN_POINT('Ctrl Pts',(-6.5658250451088,-19.5,0.714870452880859));
#41133=CARTESIAN_POINT('Ctrl Pts',(-7.21043616533279,-19.5,1.05252361297607));
#41134=CARTESIAN_POINT('Ctrl Pts',(-7.52660259604454,-19.5,1.55286467075348));
#41135=CARTESIAN_POINT('Ctrl Pts',(-4.82844471931458,-20.,0.15313720703125));
#41136=CARTESIAN_POINT('Ctrl Pts',(-4.82844471931458,-19.5,0.15313720703125));
#41137=CARTESIAN_POINT('Ctrl Pts',(-6.0685533285141,-20.,0.450886249542236));
#41138=CARTESIAN_POINT('Ctrl Pts',(-6.0685533285141,-19.5,0.450886249542236));
#41139=CARTESIAN_POINT('Ctrl Pts',(-6.5658250451088,-20.,0.714870452880859));
#41140=CARTESIAN_POINT('Ctrl Pts',(-6.5658250451088,-19.5,0.714870452880859));
#41141=CARTESIAN_POINT('',(-4.82844471931458,-19.5,0.15313720703125));
#41142=CARTESIAN_POINT('',(-4.82844471931458,-20.,0.15313720703125));
#41143=CARTESIAN_POINT('Ctrl Pts',(-4.82844471931458,-19.5,0.15313720703125));
#41144=CARTESIAN_POINT('Ctrl Pts',(-6.0685533285141,-19.5,0.450886249542236));
#41145=CARTESIAN_POINT('Ctrl Pts',(-6.5658250451088,-19.5,0.714870452880859));
#41146=CARTESIAN_POINT('Ctrl Pts',(-3.22612524032593,-20.,-0.28581166267395));
#41147=CARTESIAN_POINT('Ctrl Pts',(-3.22612524032593,-19.5,-0.28581166267395));
#41148=CARTESIAN_POINT('Ctrl Pts',(-3.5883355140686,-20.,-0.144611835479737));
#41149=CARTESIAN_POINT('Ctrl Pts',(-3.5883355140686,-19.5,-0.144611835479737));
#41150=CARTESIAN_POINT('Ctrl Pts',(-4.82844471931458,-20.,0.15313720703125));
#41151=CARTESIAN_POINT('Ctrl Pts',(-4.82844471931458,-19.5,0.15313720703125));
#41152=CARTESIAN_POINT('',(-3.22612524032593,-19.5,-0.28581166267395));
#41153=CARTESIAN_POINT('',(-3.22612524032593,-20.,-0.28581166267395));
#41154=CARTESIAN_POINT('Ctrl Pts',(-3.22612524032593,-19.5,-0.28581166267395));
#41155=CARTESIAN_POINT('Ctrl Pts',(-3.5883355140686,-19.5,-0.144611835479737));
#41156=CARTESIAN_POINT('Ctrl Pts',(-4.82844471931458,-19.5,0.15313720703125));
#41157=CARTESIAN_POINT('Ctrl Pts',(-2.41575658321381,-20.,-0.816848516464234));
#41158=CARTESIAN_POINT('Ctrl Pts',(-2.41575658321381,-19.5,-0.816848516464234));
#41159=CARTESIAN_POINT('Ctrl Pts',(-2.66132295131683,-20.,-0.500682830810547));
#41160=CARTESIAN_POINT('Ctrl Pts',(-2.66132295131683,-19.5,-0.500682830810547));
#41161=CARTESIAN_POINT('Ctrl Pts',(-3.22612524032593,-20.,-0.28581166267395));
#41162=CARTESIAN_POINT('Ctrl Pts',(-3.22612524032593,-19.5,-0.28581166267395));
#41163=CARTESIAN_POINT('',(-2.41575658321381,-19.5,-0.816848516464234));
#41164=CARTESIAN_POINT('',(-2.41575658321381,-20.,-0.816848516464234));
#41165=CARTESIAN_POINT('Ctrl Pts',(-2.41575658321381,-19.5,-0.816848516464234));
#41166=CARTESIAN_POINT('Ctrl Pts',(-2.66132295131683,-19.5,-0.500682830810547));
#41167=CARTESIAN_POINT('Ctrl Pts',(-3.22612524032593,-19.5,-0.28581166267395));
#41168=CARTESIAN_POINT('Ctrl Pts',(-2.17019081115723,-20.,-1.5566166639328));
#41169=CARTESIAN_POINT('Ctrl Pts',(-2.17019081115723,-19.5,-1.5566166639328));
#41170=CARTESIAN_POINT('Ctrl Pts',(-2.17019081115723,-20.,-1.13301539421082));
#41171=CARTESIAN_POINT('Ctrl Pts',(-2.17019081115723,-19.5,-1.13301539421082));
#41172=CARTESIAN_POINT('Ctrl Pts',(-2.41575658321381,-20.,-0.816848516464234));
#41173=CARTESIAN_POINT('Ctrl Pts',(-2.41575658321381,-19.5,-0.816848516464234));
#41174=CARTESIAN_POINT('',(-2.17019081115723,-19.5,-1.5566166639328));
#41175=CARTESIAN_POINT('',(-2.17019081115723,-20.,-1.5566166639328));
#41176=CARTESIAN_POINT('Ctrl Pts',(-2.17019081115723,-19.5,-1.5566166639328));
#41177=CARTESIAN_POINT('Ctrl Pts',(-2.17019081115723,-19.5,-1.13301539421082));
#41178=CARTESIAN_POINT('Ctrl Pts',(-2.41575658321381,-19.5,-0.816848516464234));
#41179=CARTESIAN_POINT('Ctrl Pts',(-2.4249655008316,-20.,-2.32708060741425));
#41180=CARTESIAN_POINT('Ctrl Pts',(-2.4249655008316,-19.5,-2.32708060741425));
#41181=CARTESIAN_POINT('Ctrl Pts',(-2.17019081115723,-20.,-1.97407925128937));
#41182=CARTESIAN_POINT('Ctrl Pts',(-2.17019081115723,-19.5,-1.97407925128937));
#41183=CARTESIAN_POINT('Ctrl Pts',(-2.17019081115723,-20.,-1.5566166639328));
#41184=CARTESIAN_POINT('Ctrl Pts',(-2.17019081115723,-19.5,-1.5566166639328));
#41185=CARTESIAN_POINT('',(-2.4249655008316,-19.5,-2.32708060741425));
#41186=CARTESIAN_POINT('',(-2.4249655008316,-20.,-2.32708060741425));
#41187=CARTESIAN_POINT('Ctrl Pts',(-2.4249655008316,-19.5,-2.32708060741425));
#41188=CARTESIAN_POINT('Ctrl Pts',(-2.17019081115723,-19.5,-1.97407925128937));
#41189=CARTESIAN_POINT('Ctrl Pts',(-2.17019081115723,-19.5,-1.5566166639328));
#41190=CARTESIAN_POINT('Ctrl Pts',(-3.20156872272491,-20.,-2.88267397880554));
#41191=CARTESIAN_POINT('Ctrl Pts',(-3.20156872272491,-19.5,-2.88267397880554));
#41192=CARTESIAN_POINT('Ctrl Pts',(-2.67974019050598,-20.,-2.68008136749268));
#41193=CARTESIAN_POINT('Ctrl Pts',(-2.67974019050598,-19.5,-2.68008136749268));
#41194=CARTESIAN_POINT('Ctrl Pts',(-2.4249655008316,-20.,-2.32708060741425));
#41195=CARTESIAN_POINT('Ctrl Pts',(-2.4249655008316,-19.5,-2.32708060741425));
#41196=CARTESIAN_POINT('',(-3.20156872272491,-19.5,-2.88267397880554));
#41197=CARTESIAN_POINT('',(-3.20156872272491,-20.,-2.88267397880554));
#41198=CARTESIAN_POINT('Ctrl Pts',(-3.20156872272491,-19.5,-2.88267397880554));
#41199=CARTESIAN_POINT('Ctrl Pts',(-2.67974019050598,-19.5,-2.68008136749268));
#41200=CARTESIAN_POINT('Ctrl Pts',(-2.4249655008316,-19.5,-2.32708060741425));
#41201=CARTESIAN_POINT('Ctrl Pts',(-4.40484285354614,-20.,-3.08526659011841));
#41202=CARTESIAN_POINT('Ctrl Pts',(-4.40484285354614,-19.5,-3.08526659011841));
#41203=CARTESIAN_POINT('Ctrl Pts',(-3.7233966588974,-20.,-3.08526659011841));
#41204=CARTESIAN_POINT('Ctrl Pts',(-3.7233966588974,-19.5,-3.08526659011841));
#41205=CARTESIAN_POINT('Ctrl Pts',(-3.20156872272491,-20.,-2.88267397880554));
#41206=CARTESIAN_POINT('Ctrl Pts',(-3.20156872272491,-19.5,-2.88267397880554));
#41207=CARTESIAN_POINT('',(-4.40484285354614,-19.5,-3.08526659011841));
#41208=CARTESIAN_POINT('',(-4.40484285354614,-20.,-3.08526659011841));
#41209=CARTESIAN_POINT('Ctrl Pts',(-4.40484285354614,-19.5,-3.08526659011841));
#41210=CARTESIAN_POINT('Ctrl Pts',(-3.7233966588974,-19.5,-3.08526659011841));
#41211=CARTESIAN_POINT('Ctrl Pts',(-3.20156872272491,-19.5,-2.88267397880554));
#41212=CARTESIAN_POINT('Ctrl Pts',(-5.78615248203278,-20.,-2.81821274757385));
#41213=CARTESIAN_POINT('Ctrl Pts',(-5.78615248203278,-19.5,-2.81821274757385));
#41214=CARTESIAN_POINT('Ctrl Pts',(-5.17223715782166,-20.,-3.08526659011841));
#41215=CARTESIAN_POINT('Ctrl Pts',(-5.17223715782166,-19.5,-3.08526659011841));
#41216=CARTESIAN_POINT('Ctrl Pts',(-4.40484285354614,-20.,-3.08526659011841));
#41217=CARTESIAN_POINT('Ctrl Pts',(-4.40484285354614,-19.5,-3.08526659011841));
#41218=CARTESIAN_POINT('',(-5.78615248203278,-19.5,-2.81821274757385));
#41219=CARTESIAN_POINT('',(-5.78615248203278,-20.,-2.81821274757385));
#41220=CARTESIAN_POINT('Ctrl Pts',(-5.78615248203278,-19.5,-2.81821274757385));
#41221=CARTESIAN_POINT('Ctrl Pts',(-5.17223715782166,-19.5,-3.08526659011841));
#41222=CARTESIAN_POINT('Ctrl Pts',(-4.40484285354614,-19.5,-3.08526659011841));
#41223=CARTESIAN_POINT('Ctrl Pts',(-6.69167771935463,-20.,-2.11834931373596));
#41224=CARTESIAN_POINT('Ctrl Pts',(-6.69167771935463,-19.5,-2.11834931373596));
#41225=CARTESIAN_POINT('Ctrl Pts',(-6.4000678062439,-20.,-2.55115950107574));
#41226=CARTESIAN_POINT('Ctrl Pts',(-6.4000678062439,-19.5,-2.55115950107574));
#41227=CARTESIAN_POINT('Ctrl Pts',(-5.78615248203278,-20.,-2.81821274757385));
#41228=CARTESIAN_POINT('Ctrl Pts',(-5.78615248203278,-19.5,-2.81821274757385));
#41229=CARTESIAN_POINT('',(-6.69167771935463,-19.5,-2.11834931373596));
#41230=CARTESIAN_POINT('',(-6.69167771935463,-20.,-2.11834931373596));
#41231=CARTESIAN_POINT('Ctrl Pts',(-6.69167771935463,-19.5,-2.11834931373596));
#41232=CARTESIAN_POINT('Ctrl Pts',(-6.4000678062439,-19.5,-2.55115950107574));
#41233=CARTESIAN_POINT('Ctrl Pts',(-5.78615248203278,-19.5,-2.81821274757385));
#41234=CARTESIAN_POINT('Ctrl Pts',(-7.06309646368027,-20.,-1.0102322101593));
#41235=CARTESIAN_POINT('Ctrl Pts',(-7.06309646368027,-19.5,-1.0102322101593));
#41236=CARTESIAN_POINT('Ctrl Pts',(-6.98328748345375,-20.,-1.68553912639618));
#41237=CARTESIAN_POINT('Ctrl Pts',(-6.98328748345375,-19.5,-1.68553912639618));
#41238=CARTESIAN_POINT('Ctrl Pts',(-6.69167771935463,-20.,-2.11834931373596));
#41239=CARTESIAN_POINT('Ctrl Pts',(-6.69167771935463,-19.5,-2.11834931373596));
#41240=CARTESIAN_POINT('',(-7.06309646368027,-19.5,-1.0102322101593));
#41241=CARTESIAN_POINT('',(-7.06309646368027,-20.,-1.0102322101593));
#41242=CARTESIAN_POINT('Ctrl Pts',(-7.06309646368027,-19.5,-1.0102322101593));
#41243=CARTESIAN_POINT('Ctrl Pts',(-6.98328748345375,-19.5,-1.68553912639618));
#41244=CARTESIAN_POINT('Ctrl Pts',(-6.69167771935463,-19.5,-2.11834931373596));
#41245=CARTESIAN_POINT('Origin',(-8.18656161427498,-20.,-1.10845828056335));
#41246=CARTESIAN_POINT('',(-8.18656161427498,-19.5,-1.10845828056335));
#41247=CARTESIAN_POINT('',(-8.18656161427498,-20.,-1.10845828056335));
#41248=CARTESIAN_POINT('',(-8.18656161427498,-19.5,-1.10845828056335));
#41249=CARTESIAN_POINT('Ctrl Pts',(-7.69235968589783,-20.,-2.72612595558167));
#41250=CARTESIAN_POINT('Ctrl Pts',(-7.69235968589783,-19.5,-2.72612595558167));
#41251=CARTESIAN_POINT('Ctrl Pts',(-8.16200498491526,-20.,-2.01091432571411));
#41252=CARTESIAN_POINT('Ctrl Pts',(-8.16200498491526,-19.5,-2.01091432571411));
#41253=CARTESIAN_POINT('Ctrl Pts',(-8.18656161427498,-20.,-1.10845828056335));
#41254=CARTESIAN_POINT('Ctrl Pts',(-8.18656161427498,-19.5,-1.10845828056335));
#41255=CARTESIAN_POINT('',(-7.69235968589783,-19.5,-2.72612595558167));
#41256=CARTESIAN_POINT('',(-7.69235968589783,-20.,-2.72612595558167));
#41257=CARTESIAN_POINT('Ctrl Pts',(-7.69235968589783,-19.5,-2.72612595558167));
#41258=CARTESIAN_POINT('Ctrl Pts',(-8.16200498491526,-19.5,-2.01091432571411));
#41259=CARTESIAN_POINT('Ctrl Pts',(-8.18656161427498,-19.5,-1.10845828056335));
#41260=CARTESIAN_POINT('Ctrl Pts',(-6.39699831604958,-20.,-3.79740738868713));
#41261=CARTESIAN_POINT('Ctrl Pts',(-6.39699831604958,-19.5,-3.79740738868713));
#41262=CARTESIAN_POINT('Ctrl Pts',(-7.2227144241333,-20.,-3.44133758544922));
#41263=CARTESIAN_POINT('Ctrl Pts',(-7.2227144241333,-19.5,-3.44133758544922));
#41264=CARTESIAN_POINT('Ctrl Pts',(-7.69235968589783,-20.,-2.72612595558167));
#41265=CARTESIAN_POINT('Ctrl Pts',(-7.69235968589783,-19.5,-2.72612595558167));
#41266=CARTESIAN_POINT('Ctrl Pts',(-6.39699831604958,-19.5,-3.79740738868713));
#41267=CARTESIAN_POINT('Ctrl Pts',(-7.2227144241333,-19.5,-3.44133758544922));
#41268=CARTESIAN_POINT('Ctrl Pts',(-7.69235968589783,-19.5,-2.72612595558167));
#41269=CARTESIAN_POINT('Origin',(-4.60436530411243,-19.5,0.49999988079071));
#41270=CARTESIAN_POINT('Origin',(3.1954300403595,-20.,-0.00341081619262718));
#41271=CARTESIAN_POINT('',(3.1954300403595,-19.5,-0.00341081619262718));
#41272=CARTESIAN_POINT('',(3.1954300403595,-20.,-0.00341081619262718));
#41273=CARTESIAN_POINT('',(1.81412041187287,-19.5,-0.00341081619262718));
#41274=CARTESIAN_POINT('',(3.1954300403595,-19.5,-0.00341081619262718));
#41275=CARTESIAN_POINT('',(1.81412041187287,-20.,-0.00341081619262718));
#41276=CARTESIAN_POINT('Ctrl Pts',(3.85845869779587,-20.,-0.0463845729827883));
#41277=CARTESIAN_POINT('Ctrl Pts',(3.85845869779587,-19.5,-0.0463845729827883));
#41278=CARTESIAN_POINT('Ctrl Pts',(3.65586668252945,-20.,-0.00341081619262718));
#41279=CARTESIAN_POINT('Ctrl Pts',(3.65586668252945,-19.5,-0.00341081619262718));
#41280=CARTESIAN_POINT('Ctrl Pts',(3.1954300403595,-20.,-0.00341081619262718));
#41281=CARTESIAN_POINT('Ctrl Pts',(3.1954300403595,-19.5,-0.00341081619262718));
#41282=CARTESIAN_POINT('',(3.85845869779587,-19.5,-0.0463845729827883));
#41283=CARTESIAN_POINT('',(3.85845869779587,-20.,-0.0463845729827883));
#41284=CARTESIAN_POINT('Ctrl Pts',(3.85845869779587,-19.5,-0.0463845729827883));
#41285=CARTESIAN_POINT('Ctrl Pts',(3.65586668252945,-19.5,-0.00341081619262718));
#41286=CARTESIAN_POINT('Ctrl Pts',(3.1954300403595,-19.5,-0.00341081619262718));
#41287=CARTESIAN_POINT('Ctrl Pts',(4.40177381038666,-20.,-0.28581166267395));
#41288=CARTESIAN_POINT('Ctrl Pts',(4.40177381038666,-19.5,-0.28581166267395));
#41289=CARTESIAN_POINT('Ctrl Pts',(4.13472056388855,-20.,-0.11391544342041));
#41290=CARTESIAN_POINT('Ctrl Pts',(4.13472056388855,-19.5,-0.11391544342041));
#41291=CARTESIAN_POINT('Ctrl Pts',(3.85845869779587,-20.,-0.0463845729827883));
#41292=CARTESIAN_POINT('Ctrl Pts',(3.85845869779587,-19.5,-0.0463845729827883));
#41293=CARTESIAN_POINT('',(4.40177381038666,-19.5,-0.28581166267395));
#41294=CARTESIAN_POINT('',(4.40177381038666,-20.,-0.28581166267395));
#41295=CARTESIAN_POINT('Ctrl Pts',(4.40177381038666,-19.5,-0.28581166267395));
#41296=CARTESIAN_POINT('Ctrl Pts',(4.13472056388855,-19.5,-0.11391544342041));
#41297=CARTESIAN_POINT('Ctrl Pts',(3.85845869779587,-19.5,-0.0463845729827883));
#41298=CARTESIAN_POINT('Ctrl Pts',(5.00648021697998,-20.,-0.887449026107788));
#41299=CARTESIAN_POINT('Ctrl Pts',(5.00648021697998,-19.5,-0.887449026107788));
#41300=CARTESIAN_POINT('Ctrl Pts',(4.66882705688477,-20.,-0.45770788192749));
#41301=CARTESIAN_POINT('Ctrl Pts',(4.66882705688477,-19.5,-0.45770788192749));
#41302=CARTESIAN_POINT('Ctrl Pts',(4.40177381038666,-20.,-0.28581166267395));
#41303=CARTESIAN_POINT('Ctrl Pts',(4.40177381038666,-19.5,-0.28581166267395));
#41304=CARTESIAN_POINT('',(5.00648021697998,-19.5,-0.887449026107788));
#41305=CARTESIAN_POINT('',(5.00648021697998,-20.,-0.887449026107788));
#41306=CARTESIAN_POINT('Ctrl Pts',(5.00648021697998,-19.5,-0.887449026107788));
#41307=CARTESIAN_POINT('Ctrl Pts',(4.66882705688477,-19.5,-0.45770788192749));
#41308=CARTESIAN_POINT('Ctrl Pts',(4.40177381038666,-19.5,-0.28581166267395));
#41309=CARTESIAN_POINT('Ctrl Pts',(5.86596190929413,-20.,-2.12755823135376));
#41310=CARTESIAN_POINT('Ctrl Pts',(5.86596190929413,-19.5,-2.12755823135376));
#41311=CARTESIAN_POINT('Ctrl Pts',(5.34413397312165,-20.,-1.31719017028809));
#41312=CARTESIAN_POINT('Ctrl Pts',(5.34413397312165,-19.5,-1.31719017028809));
#41313=CARTESIAN_POINT('Ctrl Pts',(5.00648021697998,-20.,-0.887449026107788));
#41314=CARTESIAN_POINT('Ctrl Pts',(5.00648021697998,-19.5,-0.887449026107788));
#41315=CARTESIAN_POINT('',(5.86596190929413,-19.5,-2.12755823135376));
#41316=CARTESIAN_POINT('',(5.86596190929413,-20.,-2.12755823135376));
#41317=CARTESIAN_POINT('Ctrl Pts',(5.86596190929413,-19.5,-2.12755823135376));
#41318=CARTESIAN_POINT('Ctrl Pts',(5.34413397312165,-19.5,-1.31719017028809));
#41319=CARTESIAN_POINT('Ctrl Pts',(5.00648021697998,-19.5,-0.887449026107788));
#41320=CARTESIAN_POINT('Origin',(7.05695748329163,-20.,-4.));
#41321=CARTESIAN_POINT('',(7.05695748329163,-19.5,-4.));
#41322=CARTESIAN_POINT('Origin',(6.98942661285401,-20.,-1.55047798156738));
#41323=CARTESIAN_POINT('',(6.98942661285401,-19.5,-1.55047798156738));
#41324=CARTESIAN_POINT('',(6.98942661285401,-20.,-1.55047798156738));
#41325=CARTESIAN_POINT('',(6.98942661285401,-19.5,-1.55047798156738));
#41326=CARTESIAN_POINT('Ctrl Pts',(6.00102305412293,-20.,-0.353342533111572));
#41327=CARTESIAN_POINT('Ctrl Pts',(6.00102305412293,-19.5,-0.353342533111572));
#41328=CARTESIAN_POINT('Ctrl Pts',(6.52285099029541,-20.,-0.832196712493897));
#41329=CARTESIAN_POINT('Ctrl Pts',(6.52285099029541,-19.5,-0.832196712493897));
#41330=CARTESIAN_POINT('Ctrl Pts',(6.98942661285401,-20.,-1.55047798156738));
#41331=CARTESIAN_POINT('Ctrl Pts',(6.98942661285401,-19.5,-1.55047798156738));
#41332=CARTESIAN_POINT('',(6.00102305412293,-19.5,-0.353342533111572));
#41333=CARTESIAN_POINT('',(6.00102305412293,-20.,-0.353342533111572));
#41334=CARTESIAN_POINT('Ctrl Pts',(6.00102305412293,-19.5,-0.353342533111572));
#41335=CARTESIAN_POINT('Ctrl Pts',(6.52285099029541,-19.5,-0.832196712493897));
#41336=CARTESIAN_POINT('Ctrl Pts',(6.98942661285401,-19.5,-1.55047798156738));
#41337=CARTESIAN_POINT('Ctrl Pts',(5.28274238109589,-20.,0.0948152542114256));
#41338=CARTESIAN_POINT('Ctrl Pts',(5.28274238109589,-19.5,0.0948152542114256));
#41339=CARTESIAN_POINT('Ctrl Pts',(5.7554566860199,-20.,-0.132333278656006));
#41340=CARTESIAN_POINT('Ctrl Pts',(5.7554566860199,-19.5,-0.132333278656006));
#41341=CARTESIAN_POINT('Ctrl Pts',(6.00102305412293,-20.,-0.353342533111572));
#41342=CARTESIAN_POINT('Ctrl Pts',(6.00102305412293,-19.5,-0.353342533111572));
#41343=CARTESIAN_POINT('',(5.28274238109589,-19.5,0.0948152542114256));
#41344=CARTESIAN_POINT('',(5.28274238109589,-20.,0.0948152542114256));
#41345=CARTESIAN_POINT('Ctrl Pts',(5.28274238109589,-19.5,0.0948152542114256));
#41346=CARTESIAN_POINT('Ctrl Pts',(5.7554566860199,-19.5,-0.132333278656006));
#41347=CARTESIAN_POINT('Ctrl Pts',(6.00102305412293,-19.5,-0.353342533111572));
#41348=CARTESIAN_POINT('Ctrl Pts',(7.19815790653229,-20.,0.92974042892456));
#41349=CARTESIAN_POINT('Ctrl Pts',(7.19815790653229,-19.5,0.92974042892456));
#41350=CARTESIAN_POINT('Ctrl Pts',(6.57810330390931,-20.,0.272850751876831));
#41351=CARTESIAN_POINT('Ctrl Pts',(6.57810330390931,-19.5,0.272850751876831));
#41352=CARTESIAN_POINT('Ctrl Pts',(5.28274238109589,-20.,0.0948152542114256));
#41353=CARTESIAN_POINT('Ctrl Pts',(5.28274238109589,-19.5,0.0948152542114256));
#41354=CARTESIAN_POINT('',(7.19815790653229,-19.5,0.92974042892456));
#41355=CARTESIAN_POINT('',(7.19815790653229,-20.,0.92974042892456));
#41356=CARTESIAN_POINT('Ctrl Pts',(7.19815790653229,-19.5,0.92974042892456));
#41357=CARTESIAN_POINT('Ctrl Pts',(6.57810330390931,-19.5,0.272850751876831));
#41358=CARTESIAN_POINT('Ctrl Pts',(5.28274238109589,-19.5,0.0948152542114256));
#41359=CARTESIAN_POINT('Ctrl Pts',(7.81821250915528,-20.,2.54433786869049));
#41360=CARTESIAN_POINT('Ctrl Pts',(7.81821250915528,-19.5,2.54433786869049));
#41361=CARTESIAN_POINT('Ctrl Pts',(7.81821250915528,-20.,1.58663010597229));
#41362=CARTESIAN_POINT('Ctrl Pts',(7.81821250915528,-19.5,1.58663010597229));
#41363=CARTESIAN_POINT('Ctrl Pts',(7.19815790653229,-20.,0.92974042892456));
#41364=CARTESIAN_POINT('Ctrl Pts',(7.19815790653229,-19.5,0.92974042892456));
#41365=CARTESIAN_POINT('',(7.81821250915528,-19.5,2.54433786869049));
#41366=CARTESIAN_POINT('',(7.81821250915528,-20.,2.54433786869049));
#41367=CARTESIAN_POINT('Ctrl Pts',(7.81821250915528,-19.5,2.54433786869049));
#41368=CARTESIAN_POINT('Ctrl Pts',(7.81821250915528,-19.5,1.58663010597229));
#41369=CARTESIAN_POINT('Ctrl Pts',(7.19815790653229,-19.5,0.92974042892456));
#41370=CARTESIAN_POINT('Ctrl Pts',(7.44372427463532,-20.,3.90109097957611));
#41371=CARTESIAN_POINT('Ctrl Pts',(7.44372427463532,-19.5,3.90109097957611));
#41372=CARTESIAN_POINT('Ctrl Pts',(7.81821250915528,-20.,3.28717565536499));
#41373=CARTESIAN_POINT('Ctrl Pts',(7.81821250915528,-19.5,3.28717565536499));
#41374=CARTESIAN_POINT('Ctrl Pts',(7.81821250915528,-20.,2.54433786869049));
#41375=CARTESIAN_POINT('Ctrl Pts',(7.81821250915528,-19.5,2.54433786869049));
#41376=CARTESIAN_POINT('',(7.44372427463532,-19.5,3.90109097957611));
#41377=CARTESIAN_POINT('',(7.44372427463532,-20.,3.90109097957611));
#41378=CARTESIAN_POINT('Ctrl Pts',(7.44372427463532,-19.5,3.90109097957611));
#41379=CARTESIAN_POINT('Ctrl Pts',(7.81821250915528,-19.5,3.28717565536499));
#41380=CARTESIAN_POINT('Ctrl Pts',(7.81821250915528,-19.5,2.54433786869049));
#41381=CARTESIAN_POINT('Ctrl Pts',(6.44304215908051,-20.,4.75750303268433));
#41382=CARTESIAN_POINT('Ctrl Pts',(6.44304215908051,-19.5,4.75750303268433));
#41383=CARTESIAN_POINT('Ctrl Pts',(7.06923604011536,-20.,4.51500630378723));
#41384=CARTESIAN_POINT('Ctrl Pts',(7.06923604011536,-19.5,4.51500630378723));
#41385=CARTESIAN_POINT('Ctrl Pts',(7.44372427463532,-20.,3.90109097957611));
#41386=CARTESIAN_POINT('Ctrl Pts',(7.44372427463532,-19.5,3.90109097957611));
#41387=CARTESIAN_POINT('',(6.44304215908051,-19.5,4.75750303268433));
#41388=CARTESIAN_POINT('',(6.44304215908051,-20.,4.75750303268433));
#41389=CARTESIAN_POINT('Ctrl Pts',(6.44304215908051,-19.5,4.75750303268433));
#41390=CARTESIAN_POINT('Ctrl Pts',(7.06923604011536,-19.5,4.51500630378723));
#41391=CARTESIAN_POINT('Ctrl Pts',(7.44372427463532,-19.5,3.90109097957611));
#41392=CARTESIAN_POINT('Ctrl Pts',(4.61357444524765,-20.,4.99999976158142));
#41393=CARTESIAN_POINT('Ctrl Pts',(4.61357444524765,-19.5,4.99999976158142));
#41394=CARTESIAN_POINT('Ctrl Pts',(5.81684827804566,-20.,4.99999976158142));
#41395=CARTESIAN_POINT('Ctrl Pts',(5.81684827804566,-19.5,4.99999976158142));
#41396=CARTESIAN_POINT('Ctrl Pts',(6.44304215908051,-20.,4.75750303268433));
#41397=CARTESIAN_POINT('Ctrl Pts',(6.44304215908051,-19.5,4.75750303268433));
#41398=CARTESIAN_POINT('',(4.61357444524765,-19.5,4.99999976158142));
#41399=CARTESIAN_POINT('',(4.61357444524765,-20.,4.99999976158142));
#41400=CARTESIAN_POINT('Ctrl Pts',(4.61357444524765,-19.5,4.99999976158142));
#41401=CARTESIAN_POINT('Ctrl Pts',(5.81684827804566,-19.5,4.99999976158142));
#41402=CARTESIAN_POINT('Ctrl Pts',(6.44304215908051,-19.5,4.75750303268433));
#41403=CARTESIAN_POINT('Origin',(0.623124465346341,-20.,4.99999976158142));
#41404=CARTESIAN_POINT('',(0.623124465346341,-19.5,4.99999976158142));
#41405=CARTESIAN_POINT('Origin',(1.81412041187287,-20.,-4.));
#41406=CARTESIAN_POINT('',(1.81412041187287,-19.5,-4.));
#41407=CARTESIAN_POINT('',(1.81412041187287,-20.,-4.));
#41408=CARTESIAN_POINT('',(1.81412041187287,-19.5,-4.));
#41409=CARTESIAN_POINT('Origin',(1.81412041187287,-20.,-0.00341081619262718));
#41410=CARTESIAN_POINT('',(1.81412041187287,-19.5,-0.00341081619262718));
#41411=CARTESIAN_POINT('Origin',(4.58901774138213,-19.5,0.49999988079071));
#41412=CARTESIAN_POINT('Origin',(25.4253059625626,-20.,4.99999976158142));
#41413=CARTESIAN_POINT('',(25.4253059625626,-19.5,4.99999976158142));
#41414=CARTESIAN_POINT('',(25.4253059625626,-20.,4.99999976158142));
#41415=CARTESIAN_POINT('',(21.833900809288,-19.5,-0.187585592269898));
#41416=CARTESIAN_POINT('',(25.4253059625626,-19.5,4.99999976158142));
#41417=CARTESIAN_POINT('',(21.833900809288,-20.,-0.187585592269898));
#41418=CARTESIAN_POINT('Origin',(24.0378570556641,-20.,4.99999976158142));
#41419=CARTESIAN_POINT('',(24.0378570556641,-19.5,4.99999976158142));
#41420=CARTESIAN_POINT('',(24.0378570556641,-20.,4.99999976158142));
#41421=CARTESIAN_POINT('',(24.0378570556641,-19.5,4.99999976158142));
#41422=CARTESIAN_POINT('Origin',(22.2943377494812,-20.,2.3540244102478));
#41423=CARTESIAN_POINT('',(22.2943377494812,-19.5,2.3540244102478));
#41424=CARTESIAN_POINT('',(22.2943377494812,-20.,2.3540244102478));
#41425=CARTESIAN_POINT('',(22.2943377494812,-19.5,2.3540244102478));
#41426=CARTESIAN_POINT('Ctrl Pts',(21.3120725750923,-20.,0.763983488082886));
#41427=CARTESIAN_POINT('Ctrl Pts',(21.3120725750923,-19.5,0.763983488082886));
#41428=CARTESIAN_POINT('Ctrl Pts',(21.7172569036484,-20.,1.46998620033264));
#41429=CARTESIAN_POINT('Ctrl Pts',(21.7172569036484,-19.5,1.46998620033264));
#41430=CARTESIAN_POINT('Ctrl Pts',(22.2943377494812,-20.,2.3540244102478));
#41431=CARTESIAN_POINT('Ctrl Pts',(22.2943377494812,-19.5,2.3540244102478));
#41432=CARTESIAN_POINT('',(21.3120725750923,-19.5,0.763983488082886));
#41433=CARTESIAN_POINT('',(21.3120725750923,-20.,0.763983488082886));
#41434=CARTESIAN_POINT('Ctrl Pts',(21.3120725750923,-19.5,0.763983488082886));
#41435=CARTESIAN_POINT('Ctrl Pts',(21.7172569036484,-19.5,1.46998620033264));
#41436=CARTESIAN_POINT('Ctrl Pts',(22.2943377494812,-19.5,2.3540244102478));
#41437=CARTESIAN_POINT('Ctrl Pts',(20.3973388671875,-20.,2.28649353981018));
#41438=CARTESIAN_POINT('Ctrl Pts',(20.3973388671875,-19.5,2.28649353981018));
#41439=CARTESIAN_POINT('Ctrl Pts',(20.8884710073471,-20.,1.52523851394653));
#41440=CARTESIAN_POINT('Ctrl Pts',(20.8884710073471,-19.5,1.52523851394653));
#41441=CARTESIAN_POINT('Ctrl Pts',(21.3120725750923,-20.,0.763983488082886));
#41442=CARTESIAN_POINT('Ctrl Pts',(21.3120725750923,-19.5,0.763983488082886));
#41443=CARTESIAN_POINT('',(20.3973388671875,-19.5,2.28649353981018));
#41444=CARTESIAN_POINT('',(20.3973388671875,-20.,2.28649353981018));
#41445=CARTESIAN_POINT('Ctrl Pts',(20.3973388671875,-19.5,2.28649353981018));
#41446=CARTESIAN_POINT('Ctrl Pts',(20.8884710073471,-19.5,1.52523851394653));
#41447=CARTESIAN_POINT('Ctrl Pts',(21.3120725750923,-19.5,0.763983488082886));
#41448=CARTESIAN_POINT('Origin',(18.6231234669685,-20.,4.99999976158142));
#41449=CARTESIAN_POINT('',(18.6231234669685,-19.5,4.99999976158142));
#41450=CARTESIAN_POINT('',(18.6231234669685,-20.,4.99999976158142));
#41451=CARTESIAN_POINT('',(18.6231234669685,-19.5,4.99999976158142));
#41452=CARTESIAN_POINT('Origin',(17.1742831147276,-20.,4.99999976158142));
#41453=CARTESIAN_POINT('',(17.1742831147276,-19.5,4.99999976158142));
#41454=CARTESIAN_POINT('',(17.1742831147276,-20.,4.99999976158142));
#41455=CARTESIAN_POINT('',(17.1742831147276,-19.5,4.99999976158142));
#41456=CARTESIAN_POINT('Origin',(20.6429049372673,-20.,-0.187585592269898));
#41457=CARTESIAN_POINT('',(20.6429049372673,-19.5,-0.187585592269898));
#41458=CARTESIAN_POINT('',(20.6429049372673,-20.,-0.187585592269898));
#41459=CARTESIAN_POINT('',(20.6429049372673,-19.5,-0.187585592269898));
#41460=CARTESIAN_POINT('Origin',(20.6429049372673,-20.,-4.));
#41461=CARTESIAN_POINT('',(20.6429049372673,-19.5,-4.));
#41462=CARTESIAN_POINT('',(20.6429049372673,-20.,-4.));
#41463=CARTESIAN_POINT('',(20.6429049372673,-19.5,-4.));
#41464=CARTESIAN_POINT('Origin',(21.833900809288,-20.,-4.));
#41465=CARTESIAN_POINT('',(21.833900809288,-19.5,-4.));
#41466=CARTESIAN_POINT('',(21.833900809288,-20.,-4.));
#41467=CARTESIAN_POINT('',(21.833900809288,-19.5,-4.));
#41468=CARTESIAN_POINT('Origin',(21.833900809288,-20.,-0.187585592269898));
#41469=CARTESIAN_POINT('',(21.833900809288,-19.5,-0.187585592269898));
#41470=CARTESIAN_POINT('Origin',(21.2997945386451,-19.5,0.49999988079071));
#41471=CARTESIAN_POINT('Origin',(-75.7581216659255,-14.1,31.3800414539374));
#41472=CARTESIAN_POINT('',(-81.2581216659255,-14.1,31.3800414539374));
#41473=CARTESIAN_POINT('Origin',(31.3800414539374,-14.1,75.7581216659255));
#41474=CARTESIAN_POINT('',(25.8800414539374,-14.1,75.7581216659255));
#41475=CARTESIAN_POINT('Origin',(-31.3800414539374,-14.1,75.7581216659255));
#41476=CARTESIAN_POINT('',(-36.8800414539374,-14.1,75.7581216659255));
#41477=CARTESIAN_POINT('Origin',(75.7581216659255,-14.1,31.3800414539374));
#41478=CARTESIAN_POINT('',(70.2581216659255,-14.1,31.3800414539374));
#41479=CARTESIAN_POINT('Origin',(0.,-3.05,75.05));
#41480=CARTESIAN_POINT('Origin',(-2.22044604925031E-15,-5.,-1.11022302462516E-15));
#41481=CARTESIAN_POINT('',(28.5,-9.,49.363448015713));
#41482=CARTESIAN_POINT('',(28.5,-5.,49.363448015713));
#41483=CARTESIAN_POINT('',(-28.5,-9.,49.363448015713));
#41484=CARTESIAN_POINT('Origin',(-2.22044604925031E-15,-9.,-1.11022302462516E-15));
#41485=CARTESIAN_POINT('',(-28.5,-5.,49.363448015713));
#41486=CARTESIAN_POINT('Origin',(35.1,-5.,60.7949833456676));
#41487=CARTESIAN_POINT('',(35.1,-9.,60.7949833456676));
#41488=CARTESIAN_POINT('Origin',(-28.5,-5.,49.363448015713));
#41489=CARTESIAN_POINT('',(-35.1,-9.,60.7949833456676));
#41490=CARTESIAN_POINT('Origin',(1.77635683940025E-14,-9.,-4.70250832716619));
#41491=CARTESIAN_POINT('Origin',(-50.,-14.,5.00000000000001));
#41492=CARTESIAN_POINT('',(0.,0.,0.));
#41493=CARTESIAN_POINT('Origin',(0.,133.75,0.));
#41494=CARTESIAN_POINT('',(-3.24653866453963E-15,134.,-26.51));
#41495=CARTESIAN_POINT('Origin',(0.,134.,0.));
#41496=CARTESIAN_POINT('',(3.18530632458227E-15,133.5,-26.01));
#41497=CARTESIAN_POINT('',(-3.21592249456095E-15,133.75,-26.26));
#41498=CARTESIAN_POINT('Origin',(0.,133.5,0.));
#41499=CARTESIAN_POINT('Origin',(0.,100.05,0.));
#41500=CARTESIAN_POINT('',(-3.18530632458227E-15,130.65,-26.01));
#41501=CARTESIAN_POINT('Origin',(0.,130.65,0.));
#41502=CARTESIAN_POINT('',(-3.18530632458227E-15,100.05,-26.01));
#41503=CARTESIAN_POINT('Origin',(0.,134.,0.));
#41504=CARTESIAN_POINT('',(47.,134.,-41.));
#41505=CARTESIAN_POINT('',(41.,134.,-47.));
#41506=CARTESIAN_POINT('Origin',(41.,134.,-41.));
#41507=CARTESIAN_POINT('',(-41.,134.,-47.));
#41508=CARTESIAN_POINT('',(-41.,134.,-47.));
#41509=CARTESIAN_POINT('',(-47.,134.,-41.));
#41510=CARTESIAN_POINT('Origin',(-41.,134.,-41.));
#41511=CARTESIAN_POINT('',(-47.,134.,41.));
#41512=CARTESIAN_POINT('',(-47.,134.,41.));
#41513=CARTESIAN_POINT('',(-41.,134.,47.));
#41514=CARTESIAN_POINT('Origin',(-41.,134.,41.));
#41515=CARTESIAN_POINT('',(41.,134.,47.));
#41516=CARTESIAN_POINT('',(41.,134.,47.));
#41517=CARTESIAN_POINT('',(47.,134.,41.));
#41518=CARTESIAN_POINT('Origin',(41.,134.,41.));
#41519=CARTESIAN_POINT('',(47.,134.,-41.));
#41520=CARTESIAN_POINT('Origin',(0.,130.4,0.));
#41521=CARTESIAN_POINT('',(3.24653866453963E-15,130.15,-26.51));
#41522=CARTESIAN_POINT('',(-3.21592249456095E-15,130.4,-26.26));
#41523=CARTESIAN_POINT('Origin',(0.,130.15,0.));
#41524=CARTESIAN_POINT('Origin',(0.,130.15,25.9));
#41525=CARTESIAN_POINT('',(-3.36777869765522E-15,130.15,-27.5));
#41526=CARTESIAN_POINT('Origin',(0.,130.15,0.));
#41527=CARTESIAN_POINT('Origin',(60.,190.,-125.25));
#41528=CARTESIAN_POINT('',(52.5,190.,-125.));
#41529=CARTESIAN_POINT('Origin',(60.,190.,-125.));
#41530=CARTESIAN_POINT('',(53.,190.,-125.5));
#41531=CARTESIAN_POINT('',(52.75,190.,-125.25));
#41532=CARTESIAN_POINT('Origin',(60.,190.,-125.5));
#41533=CARTESIAN_POINT('Origin',(0.,182.5,-125.));
#41534=CARTESIAN_POINT('',(-75.,164.,-125.));
#41535=CARTESIAN_POINT('',(-71.,160.,-125.));
#41536=CARTESIAN_POINT('Origin',(-71.,164.,-125.));
#41537=CARTESIAN_POINT('',(71.,160.,-125.));
#41538=CARTESIAN_POINT('',(-71.,160.,-125.));
#41539=CARTESIAN_POINT('',(75.,164.,-125.));
#41540=CARTESIAN_POINT('Origin',(71.,164.,-125.));
#41541=CARTESIAN_POINT('',(75.,201.,-125.));
#41542=CARTESIAN_POINT('',(75.,164.,-125.));
#41543=CARTESIAN_POINT('',(71.,205.,-125.));
#41544=CARTESIAN_POINT('Origin',(71.,201.,-125.));
#41545=CARTESIAN_POINT('',(0.,205.,-125.));
#41546=CARTESIAN_POINT('',(71.,205.,-125.));
#41547=CARTESIAN_POINT('',(0.,204.5,-125.));
#41548=CARTESIAN_POINT('',(0.,209.75,-125.));
#41549=CARTESIAN_POINT('',(-71.,205.,-125.));
#41550=CARTESIAN_POINT('',(71.,205.,-125.));
#41551=CARTESIAN_POINT('',(-75.,201.,-125.));
#41552=CARTESIAN_POINT('Origin',(-71.,201.,-125.));
#41553=CARTESIAN_POINT('',(-75.,201.,-125.));
#41554=CARTESIAN_POINT('',(-67.5,190.,-125.));
#41555=CARTESIAN_POINT('Origin',(-60.,190.,-125.));
#41556=CARTESIAN_POINT('',(-36.,165.,-125.));
#41557=CARTESIAN_POINT('',(36.,165.,-125.));
#41558=CARTESIAN_POINT('',(-36.,165.,-125.));
#41559=CARTESIAN_POINT('',(-40.,169.,-125.));
#41560=CARTESIAN_POINT('Origin',(-36.,169.,-125.));
#41561=CARTESIAN_POINT('',(-40.,196.,-125.));
#41562=CARTESIAN_POINT('',(-40.,196.,-125.));
#41563=CARTESIAN_POINT('',(-36.,200.,-125.));
#41564=CARTESIAN_POINT('Origin',(-36.,196.,-125.));
#41565=CARTESIAN_POINT('',(36.,200.,-125.));
#41566=CARTESIAN_POINT('',(36.,200.,-125.));
#41567=CARTESIAN_POINT('',(40.,196.,-125.));
#41568=CARTESIAN_POINT('Origin',(36.,196.,-125.));
#41569=CARTESIAN_POINT('',(40.,169.,-125.));
#41570=CARTESIAN_POINT('',(40.,169.,-125.));
#41571=CARTESIAN_POINT('Origin',(36.,169.,-125.));
#41572=CARTESIAN_POINT('Origin',(60.,190.,-125.));
#41573=CARTESIAN_POINT('',(53.,190.,-139.5));
#41574=CARTESIAN_POINT('',(53.,190.,-125.));
#41575=CARTESIAN_POINT('Origin',(60.,190.,-139.5));
#41576=CARTESIAN_POINT('Origin',(-60.,190.,-125.25));
#41577=CARTESIAN_POINT('',(-67.,190.,-125.5));
#41578=CARTESIAN_POINT('',(-67.25,190.,-125.25));
#41579=CARTESIAN_POINT('Origin',(-60.,190.,-125.5));
#41580=CARTESIAN_POINT('Origin',(-60.,190.,-125.));
#41581=CARTESIAN_POINT('',(-67.,190.,-139.5));
#41582=CARTESIAN_POINT('',(-67.,190.,-125.));
#41583=CARTESIAN_POINT('Origin',(-60.,190.,-139.5));
#41584=CARTESIAN_POINT('Origin',(-47.25,193.,38.));
#41585=CARTESIAN_POINT('',(-47.,193.55,41.));
#41586=CARTESIAN_POINT('',(-47.5,193.459836065574,40.5081967213115));
#41587=CARTESIAN_POINT('',(-47.,193.55,41.));
#41588=CARTESIAN_POINT('',(-47.5,192.540163934426,40.5081967213115));
#41589=CARTESIAN_POINT('Origin',(-47.5,193.,38.));
#41590=CARTESIAN_POINT('',(-47.,192.45,41.));
#41591=CARTESIAN_POINT('',(-47.5,192.540163934426,40.5081967213115));
#41592=CARTESIAN_POINT('Origin',(-47.,193.,38.));
#41593=CARTESIAN_POINT('Ctrl Pts',(-47.,192.45,41.));
#41594=CARTESIAN_POINT('Ctrl Pts',(-47.,192.812639548803,41.0664839172805));
#41595=CARTESIAN_POINT('Ctrl Pts',(-47.,193.187360451197,41.0664839172805));
#41596=CARTESIAN_POINT('Ctrl Pts',(-47.,193.55,41.));
#41597=CARTESIAN_POINT('Ctrl Pts',(-47.1666666666667,192.480054644809,40.8360655737705));
#41598=CARTESIAN_POINT('Ctrl Pts',(-47.1666666666667,192.822877824825,40.8989164901067));
#41599=CARTESIAN_POINT('Ctrl Pts',(-47.1666666666667,193.177122175175,40.8989164901067));
#41600=CARTESIAN_POINT('Ctrl Pts',(-47.1666666666667,193.519945355191,40.8360655737705));
#41601=CARTESIAN_POINT('Ctrl Pts',(-47.3333333333333,192.510109289617,40.672131147541));
#41602=CARTESIAN_POINT('Ctrl Pts',(-47.3333333333333,192.833116100846,40.7313490629329));
#41603=CARTESIAN_POINT('Ctrl Pts',(-47.3333333333333,193.166883899154,40.7313490629329));
#41604=CARTESIAN_POINT('Ctrl Pts',(-47.3333333333333,193.489890710383,40.672131147541));
#41605=CARTESIAN_POINT('Ctrl Pts',(-47.5,192.540163934426,40.5081967213115));
#41606=CARTESIAN_POINT('Ctrl Pts',(-47.5,192.843354376868,40.5637816357591));
#41607=CARTESIAN_POINT('Ctrl Pts',(-47.5,193.156645623132,40.5637816357591));
#41608=CARTESIAN_POINT('Ctrl Pts',(-47.5,193.459836065574,40.5081967213115));
#41609=CARTESIAN_POINT('Ctrl Pts',(-47.,193.55,41.));
#41610=CARTESIAN_POINT('Ctrl Pts',(-47.,193.187360451197,41.0664839172805));
#41611=CARTESIAN_POINT('Ctrl Pts',(-47.,192.812639548803,41.0664839172805));
#41612=CARTESIAN_POINT('Ctrl Pts',(-47.,192.45,41.));
#41613=CARTESIAN_POINT('',(-47.5,193.,40.5498854071472));
#41614=CARTESIAN_POINT('Ctrl Pts',(-47.5,192.540163934426,40.5081967213115));
#41615=CARTESIAN_POINT('Ctrl Pts',(-47.5,192.691759155647,40.5359891785353));
#41616=CARTESIAN_POINT('Ctrl Pts',(-47.5,192.845879577824,40.5498854071472));
#41617=CARTESIAN_POINT('Ctrl Pts',(-47.5,193.,40.5498854071472));
#41618=CARTESIAN_POINT('Ctrl Pts',(-47.5,193.,40.5498854071472));
#41619=CARTESIAN_POINT('Ctrl Pts',(-47.5,193.154120422176,40.5498854071472));
#41620=CARTESIAN_POINT('Ctrl Pts',(-47.5,193.308240844353,40.5359891785353));
#41621=CARTESIAN_POINT('Ctrl Pts',(-47.5,193.459836065574,40.5081967213115));
#41622=CARTESIAN_POINT('Origin',(-47.,134.,-41.));
#41623=CARTESIAN_POINT('',(-47.,141.55,41.));
#41624=CARTESIAN_POINT('',(-47.,134.,41.));
#41625=CARTESIAN_POINT('',(-47.,140.45,41.));
#41626=CARTESIAN_POINT('Origin',(-47.,141.,38.));
#41627=CARTESIAN_POINT('',(-47.,134.,41.));
#41628=CARTESIAN_POINT('',(-47.,140.45,-41.));
#41629=CARTESIAN_POINT('',(-47.,134.,-41.));
#41630=CARTESIAN_POINT('',(-47.,141.55,-41.));
#41631=CARTESIAN_POINT('Origin',(-47.,141.,-38.));
#41632=CARTESIAN_POINT('',(-47.,192.45,-41.));
#41633=CARTESIAN_POINT('',(-47.,134.,-41.));
#41634=CARTESIAN_POINT('',(-47.,193.55,-41.));
#41635=CARTESIAN_POINT('Origin',(-47.,193.,-38.));
#41636=CARTESIAN_POINT('',(-47.,203.,-41.));
#41637=CARTESIAN_POINT('',(-47.,134.,-41.));
#41638=CARTESIAN_POINT('',(-47.,203.,0.));
#41639=CARTESIAN_POINT('',(-47.,203.,41.));
#41640=CARTESIAN_POINT('',(-47.,203.,41.));
#41641=CARTESIAN_POINT('',(-47.,203.,41.));
#41642=CARTESIAN_POINT('',(-47.,134.,41.));
#41643=CARTESIAN_POINT('',(-47.,194.,-24.));
#41644=CARTESIAN_POINT('',(-47.,194.,24.));
#41645=CARTESIAN_POINT('',(-47.,194.,-32.5));
#41646=CARTESIAN_POINT('',(-47.,186.,-32.));
#41647=CARTESIAN_POINT('Origin',(-47.,186.,-24.));
#41648=CARTESIAN_POINT('',(-47.,148.,-32.));
#41649=CARTESIAN_POINT('',(-47.,141.,-32.));
#41650=CARTESIAN_POINT('',(-47.,140.,-24.));
#41651=CARTESIAN_POINT('Origin',(-47.,148.,-24.));
#41652=CARTESIAN_POINT('',(-47.,140.,24.));
#41653=CARTESIAN_POINT('',(-47.,140.,-8.5));
#41654=CARTESIAN_POINT('',(-47.,148.,32.));
#41655=CARTESIAN_POINT('Origin',(-47.,148.,24.));
#41656=CARTESIAN_POINT('',(-47.,186.,32.));
#41657=CARTESIAN_POINT('',(-47.,160.,32.));
#41658=CARTESIAN_POINT('Origin',(-47.,186.,24.));
#41659=CARTESIAN_POINT('Origin',(-55.,193.,38.));
#41660=CARTESIAN_POINT('',(-54.5,193.,40.55));
#41661=CARTESIAN_POINT('Origin',(-54.5,193.,38.));
#41662=CARTESIAN_POINT('',(-55.,193.,40.55));
#41663=CARTESIAN_POINT('Origin',(-47.25,141.,-38.));
#41664=CARTESIAN_POINT('',(-47.5,140.540163934426,-40.5081967213115));
#41665=CARTESIAN_POINT('',(-47.,140.45,-41.));
#41666=CARTESIAN_POINT('',(-47.5,141.,-35.45));
#41667=CARTESIAN_POINT('Origin',(-47.5,141.,-38.));
#41668=CARTESIAN_POINT('',(-47.5,141.459836065574,-40.5081967213115));
#41669=CARTESIAN_POINT('Origin',(-47.5,141.,-38.));
#41670=CARTESIAN_POINT('',(-47.5,141.459836065574,-40.5081967213115));
#41671=CARTESIAN_POINT('Ctrl Pts',(-47.,141.55,-41.));
#41672=CARTESIAN_POINT('Ctrl Pts',(-47.,141.187360451197,-41.0664839172806));
#41673=CARTESIAN_POINT('Ctrl Pts',(-47.,140.812639548803,-41.0664839172805));
#41674=CARTESIAN_POINT('Ctrl Pts',(-47.,140.45,-41.));
#41675=CARTESIAN_POINT('Ctrl Pts',(-47.1666666666667,141.519945355191,-40.8360655737705));
#41676=CARTESIAN_POINT('Ctrl Pts',(-47.1666666666667,141.177122175175,-40.8989164901067));
#41677=CARTESIAN_POINT('Ctrl Pts',(-47.1666666666667,140.822877824825,-40.8989164901067));
#41678=CARTESIAN_POINT('Ctrl Pts',(-47.1666666666667,140.480054644809,-40.8360655737705));
#41679=CARTESIAN_POINT('Ctrl Pts',(-47.3333333333333,141.489890710382,-40.672131147541));
#41680=CARTESIAN_POINT('Ctrl Pts',(-47.3333333333333,141.166883899154,-40.7313490629329));
#41681=CARTESIAN_POINT('Ctrl Pts',(-47.3333333333333,140.833116100846,-40.7313490629329));
#41682=CARTESIAN_POINT('Ctrl Pts',(-47.3333333333333,140.510109289617,-40.672131147541));
#41683=CARTESIAN_POINT('Ctrl Pts',(-47.5,141.459836065574,-40.5081967213115));
#41684=CARTESIAN_POINT('Ctrl Pts',(-47.5,141.156645623132,-40.5637816357591));
#41685=CARTESIAN_POINT('Ctrl Pts',(-47.5,140.843354376868,-40.5637816357591));
#41686=CARTESIAN_POINT('Ctrl Pts',(-47.5,140.540163934426,-40.5081967213115));
#41687=CARTESIAN_POINT('Ctrl Pts',(-47.,140.45,-41.));
#41688=CARTESIAN_POINT('Ctrl Pts',(-47.,140.812639548803,-41.0664839172805));
#41689=CARTESIAN_POINT('Ctrl Pts',(-47.,141.187360451197,-41.0664839172806));
#41690=CARTESIAN_POINT('Ctrl Pts',(-47.,141.55,-41.));
#41691=CARTESIAN_POINT('Ctrl Pts',(-47.5,141.459836065574,-40.5081967213115));
#41692=CARTESIAN_POINT('Ctrl Pts',(-47.5,141.156645623132,-40.5637816357591));
#41693=CARTESIAN_POINT('Ctrl Pts',(-47.5,140.843354376868,-40.5637816357591));
#41694=CARTESIAN_POINT('Ctrl Pts',(-47.5,140.540163934426,-40.5081967213115));
#41695=CARTESIAN_POINT('Origin',(-41.,134.,-41.));
#41696=CARTESIAN_POINT('',(-41.,203.,-47.));
#41697=CARTESIAN_POINT('',(-41.,134.,-47.));
#41698=CARTESIAN_POINT('Origin',(-41.,203.,-41.));
#41699=CARTESIAN_POINT('Ctrl Pts',(-47.,192.45,-41.));
#41700=CARTESIAN_POINT('Ctrl Pts',(-47.,192.812639548803,-41.0664839172806));
#41701=CARTESIAN_POINT('Ctrl Pts',(-47.,193.187360451197,-41.0664839172806));
#41702=CARTESIAN_POINT('Ctrl Pts',(-47.,193.55,-41.));
#41703=CARTESIAN_POINT('Origin',(-55.,141.,-38.));
#41704=CARTESIAN_POINT('',(-54.5,141.,-35.45));
#41705=CARTESIAN_POINT('Origin',(-54.5,141.,-38.));
#41706=CARTESIAN_POINT('',(-55.,141.,-35.45));
#41707=CARTESIAN_POINT('Origin',(-47.25,141.,38.));
#41708=CARTESIAN_POINT('',(-47.5,141.459836065574,40.5081967213115));
#41709=CARTESIAN_POINT('',(-47.,141.55,41.));
#41710=CARTESIAN_POINT('',(-47.5,140.540163934426,40.5081967213115));
#41711=CARTESIAN_POINT('Origin',(-47.5,141.,38.));
#41712=CARTESIAN_POINT('',(-47.5,140.540163934426,40.5081967213115));
#41713=CARTESIAN_POINT('Ctrl Pts',(-47.,140.45,41.));
#41714=CARTESIAN_POINT('Ctrl Pts',(-47.,140.812639548803,41.0664839172806));
#41715=CARTESIAN_POINT('Ctrl Pts',(-47.,141.187360451197,41.0664839172805));
#41716=CARTESIAN_POINT('Ctrl Pts',(-47.,141.55,41.));
#41717=CARTESIAN_POINT('Ctrl Pts',(-47.1666666666667,140.480054644809,40.8360655737705));
#41718=CARTESIAN_POINT('Ctrl Pts',(-47.1666666666667,140.822877824825,40.8989164901067));
#41719=CARTESIAN_POINT('Ctrl Pts',(-47.1666666666667,141.177122175175,40.8989164901067));
#41720=CARTESIAN_POINT('Ctrl Pts',(-47.1666666666667,141.519945355191,40.8360655737705));
#41721=CARTESIAN_POINT('Ctrl Pts',(-47.3333333333333,140.510109289617,40.672131147541));
#41722=CARTESIAN_POINT('Ctrl Pts',(-47.3333333333333,140.833116100846,40.7313490629329));
#41723=CARTESIAN_POINT('Ctrl Pts',(-47.3333333333333,141.166883899154,40.7313490629329));
#41724=CARTESIAN_POINT('Ctrl Pts',(-47.3333333333333,141.489890710383,40.672131147541));
#41725=CARTESIAN_POINT('Ctrl Pts',(-47.5,140.540163934426,40.5081967213115));
#41726=CARTESIAN_POINT('Ctrl Pts',(-47.5,140.843354376868,40.5637816357591));
#41727=CARTESIAN_POINT('Ctrl Pts',(-47.5,141.156645623132,40.5637816357591));
#41728=CARTESIAN_POINT('Ctrl Pts',(-47.5,141.459836065574,40.5081967213115));
#41729=CARTESIAN_POINT('Ctrl Pts',(-47.,141.55,41.));
#41730=CARTESIAN_POINT('Ctrl Pts',(-47.,141.187360451197,41.0664839172805));
#41731=CARTESIAN_POINT('Ctrl Pts',(-47.,140.812639548803,41.0664839172806));
#41732=CARTESIAN_POINT('Ctrl Pts',(-47.,140.45,41.));
#41733=CARTESIAN_POINT('',(-47.5,141.,40.5498854071472));
#41734=CARTESIAN_POINT('Ctrl Pts',(-47.5,140.540163934426,40.5081967213115));
#41735=CARTESIAN_POINT('Ctrl Pts',(-47.5,140.691759155647,40.5359891785353));
#41736=CARTESIAN_POINT('Ctrl Pts',(-47.5,140.845879577824,40.5498854071472));
#41737=CARTESIAN_POINT('Ctrl Pts',(-47.5,141.,40.5498854071472));
#41738=CARTESIAN_POINT('Ctrl Pts',(-47.5,141.,40.5498854071472));
#41739=CARTESIAN_POINT('Ctrl Pts',(-47.5,141.154120422176,40.5498854071472));
#41740=CARTESIAN_POINT('Ctrl Pts',(-47.5,141.308240844353,40.5359891785353));
#41741=CARTESIAN_POINT('Ctrl Pts',(-47.5,141.459836065574,40.5081967213115));
#41742=CARTESIAN_POINT('Origin',(-55.,141.,38.));
#41743=CARTESIAN_POINT('',(-54.5,141.,40.55));
#41744=CARTESIAN_POINT('Origin',(-54.5,141.,38.));
#41745=CARTESIAN_POINT('',(-55.,141.,40.55));
#41746=CARTESIAN_POINT('Origin',(-47.25,193.,-38.));
#41747=CARTESIAN_POINT('',(-47.5,192.540163934426,-40.5081967213115));
#41748=CARTESIAN_POINT('',(-47.,192.45,-41.));
#41749=CARTESIAN_POINT('',(-47.5,193.,-35.45));
#41750=CARTESIAN_POINT('Origin',(-47.5,193.,-38.));
#41751=CARTESIAN_POINT('',(-47.5,193.459836065574,-40.5081967213115));
#41752=CARTESIAN_POINT('Origin',(-47.5,193.,-38.));
#41753=CARTESIAN_POINT('',(-47.5,193.459836065574,-40.5081967213115));
#41754=CARTESIAN_POINT('Ctrl Pts',(-47.,193.55,-41.));
#41755=CARTESIAN_POINT('Ctrl Pts',(-47.,193.187360451197,-41.0664839172806));
#41756=CARTESIAN_POINT('Ctrl Pts',(-47.,192.812639548803,-41.0664839172806));
#41757=CARTESIAN_POINT('Ctrl Pts',(-47.,192.45,-41.));
#41758=CARTESIAN_POINT('Ctrl Pts',(-47.1666666666667,193.519945355191,-40.8360655737705));
#41759=CARTESIAN_POINT('Ctrl Pts',(-47.1666666666667,193.177122175175,-40.8989164901067));
#41760=CARTESIAN_POINT('Ctrl Pts',(-47.1666666666667,192.822877824825,-40.8989164901067));
#41761=CARTESIAN_POINT('Ctrl Pts',(-47.1666666666667,192.480054644809,-40.8360655737705));
#41762=CARTESIAN_POINT('Ctrl Pts',(-47.3333333333333,193.489890710383,-40.672131147541));
#41763=CARTESIAN_POINT('Ctrl Pts',(-47.3333333333333,193.166883899154,-40.7313490629329));
#41764=CARTESIAN_POINT('Ctrl Pts',(-47.3333333333333,192.833116100846,-40.7313490629329));
#41765=CARTESIAN_POINT('Ctrl Pts',(-47.3333333333333,192.510109289617,-40.672131147541));
#41766=CARTESIAN_POINT('Ctrl Pts',(-47.5,193.459836065574,-40.5081967213115));
#41767=CARTESIAN_POINT('Ctrl Pts',(-47.5,193.156645623132,-40.5637816357591));
#41768=CARTESIAN_POINT('Ctrl Pts',(-47.5,192.843354376868,-40.5637816357591));
#41769=CARTESIAN_POINT('Ctrl Pts',(-47.5,192.540163934426,-40.5081967213115));
#41770=CARTESIAN_POINT('Ctrl Pts',(-47.5,193.459836065574,-40.5081967213115));
#41771=CARTESIAN_POINT('Ctrl Pts',(-47.5,193.156645623132,-40.5637816357591));
#41772=CARTESIAN_POINT('Ctrl Pts',(-47.5,192.843354376868,-40.5637816357591));
#41773=CARTESIAN_POINT('Ctrl Pts',(-47.5,192.540163934426,-40.5081967213115));
#41774=CARTESIAN_POINT('Origin',(-55.,193.,-38.));
#41775=CARTESIAN_POINT('',(-54.5,193.,-35.45));
#41776=CARTESIAN_POINT('Origin',(-54.5,193.,-38.));
#41777=CARTESIAN_POINT('',(-55.,193.,-35.45));
#41778=CARTESIAN_POINT('Origin',(-54.75,193.,-38.));
#41779=CARTESIAN_POINT('',(-55.,193.,-34.95));
#41780=CARTESIAN_POINT('Origin',(-55.,193.,-38.));
#41781=CARTESIAN_POINT('',(-54.75,193.,-35.2));
#41782=CARTESIAN_POINT('Origin',(-55.,130.,-47.));
#41783=CARTESIAN_POINT('',(-55.,132.,47.));
#41784=CARTESIAN_POINT('',(-55.,132.,-47.));
#41785=CARTESIAN_POINT('',(-55.,132.,-23.5));
#41786=CARTESIAN_POINT('',(-55.,199.531133844866,47.));
#41787=CARTESIAN_POINT('',(-55.,130.,47.));
#41788=CARTESIAN_POINT('',(-55.,199.004037328772,32.85003536606));
#41789=CARTESIAN_POINT('Ctrl Pts',(-55.,199.531133844866,47.0000000000002));
#41790=CARTESIAN_POINT('Ctrl Pts',(-55.,199.22088305859,39.4954174846766));
#41791=CARTESIAN_POINT('Ctrl Pts',(-55.,199.004037328771,32.8500353660488));
#41792=CARTESIAN_POINT('',(-55.,199.,32.6016382508379));
#41793=CARTESIAN_POINT('Ctrl Pts',(-55.,199.004037328772,32.85003536606));
#41794=CARTESIAN_POINT('Ctrl Pts',(-55.,199.001278753317,32.7654969801016));
#41795=CARTESIAN_POINT('Ctrl Pts',(-55.,199.,32.6824692460632));
#41796=CARTESIAN_POINT('Ctrl Pts',(-55.,199.,32.6016382508379));
#41797=CARTESIAN_POINT('',(-55.,199.,-32.6016382508379));
#41798=CARTESIAN_POINT('',(-55.,199.,8.5));
#41799=CARTESIAN_POINT('',(-55.,199.004037328772,-32.85003536606));
#41800=CARTESIAN_POINT('Ctrl Pts',(-55.,199.,-32.6016382508379));
#41801=CARTESIAN_POINT('Ctrl Pts',(-55.,199.,-32.6824692460632));
#41802=CARTESIAN_POINT('Ctrl Pts',(-55.,199.001278753317,-32.7654969801016));
#41803=CARTESIAN_POINT('Ctrl Pts',(-55.,199.004037328772,-32.85003536606));
#41804=CARTESIAN_POINT('',(-55.,199.531133844866,-47.));
#41805=CARTESIAN_POINT('Ctrl Pts',(-55.,199.004037328772,-32.85003536606));
#41806=CARTESIAN_POINT('Ctrl Pts',(-55.,199.22088305859,-39.4954174846828));
#41807=CARTESIAN_POINT('Ctrl Pts',(-55.,199.531133844866,-47.0000000000002));
#41808=CARTESIAN_POINT('',(-55.,130.,-47.));
#41809=CARTESIAN_POINT('',(-55.,141.,41.05));
#41810=CARTESIAN_POINT('Origin',(-55.,141.,38.));
#41811=CARTESIAN_POINT('',(-55.,193.,41.05));
#41812=CARTESIAN_POINT('Origin',(-55.,193.,38.));
#41813=CARTESIAN_POINT('',(-55.,194.,24.));
#41814=CARTESIAN_POINT('',(-55.,194.,-24.));
#41815=CARTESIAN_POINT('',(-55.,194.,-35.5));
#41816=CARTESIAN_POINT('',(-55.,186.,32.));
#41817=CARTESIAN_POINT('Origin',(-55.,186.,24.));
#41818=CARTESIAN_POINT('',(-55.,148.,32.));
#41819=CARTESIAN_POINT('',(-55.,158.,32.));
#41820=CARTESIAN_POINT('',(-55.,140.,24.));
#41821=CARTESIAN_POINT('Origin',(-55.,148.,24.));
#41822=CARTESIAN_POINT('',(-55.,140.,-24.));
#41823=CARTESIAN_POINT('',(-55.,140.,-11.5));
#41824=CARTESIAN_POINT('',(-55.,148.,-32.));
#41825=CARTESIAN_POINT('Origin',(-55.,148.,-24.));
#41826=CARTESIAN_POINT('',(-55.,186.,-32.));
#41827=CARTESIAN_POINT('',(-55.,139.,-32.));
#41828=CARTESIAN_POINT('Origin',(-55.,186.,-24.));
#41829=CARTESIAN_POINT('',(-55.,141.,-34.95));
#41830=CARTESIAN_POINT('Origin',(-55.,141.,-38.));
#41831=CARTESIAN_POINT('Origin',(-54.75,141.,38.));
#41832=CARTESIAN_POINT('',(-54.75,141.,40.8));
#41833=CARTESIAN_POINT('Origin',(-54.75,141.,-38.));
#41834=CARTESIAN_POINT('',(-54.75,141.,-35.2));
#41835=CARTESIAN_POINT('Origin',(-54.75,193.,38.));
#41836=CARTESIAN_POINT('',(-54.75,193.,40.8));
#41837=CARTESIAN_POINT('Origin',(-76.0139789775539,214.75,-76.0139789775538));
#41838=CARTESIAN_POINT('',(-83.5139789775539,215.,-76.0139789775538));
#41839=CARTESIAN_POINT('Origin',(-76.0139789775539,215.,-76.0139789775538));
#41840=CARTESIAN_POINT('',(-83.0139789775539,214.5,-76.0139789775538));
#41841=CARTESIAN_POINT('',(-83.2639789775539,214.75,-76.0139789775538));
#41842=CARTESIAN_POINT('Origin',(-76.0139789775539,214.5,-76.0139789775538));
#41843=CARTESIAN_POINT('Origin',(0.,215.,45.));
#41844=CARTESIAN_POINT('',(-1.50631556295124E-14,215.,-123.));
#41845=CARTESIAN_POINT('Origin',(0.,215.,0.));
#41846=CARTESIAN_POINT('',(-83.5139789775538,215.,76.0139789775539));
#41847=CARTESIAN_POINT('Origin',(-76.0139789775538,215.,76.0139789775539));
#41848=CARTESIAN_POINT('',(68.5139789775538,215.,-76.0139789775539));
#41849=CARTESIAN_POINT('Origin',(76.0139789775538,215.,-76.0139789775539));
#41850=CARTESIAN_POINT('',(-1.12789970201471E-14,215.,92.1));
#41851=CARTESIAN_POINT('Origin',(0.,215.,0.));
#41852=CARTESIAN_POINT('',(68.5139789775538,215.,76.0139789775539));
#41853=CARTESIAN_POINT('Origin',(76.0139789775539,215.,76.0139789775539));
#41854=CARTESIAN_POINT('Origin',(-76.0139789775539,202.9,-76.0139789775538));
#41855=CARTESIAN_POINT('',(-83.0139789775539,202.9,-76.0139789775538));
#41856=CARTESIAN_POINT('Origin',(-76.0139789775539,202.9,-76.0139789775538));
#41857=CARTESIAN_POINT('',(-83.0139789775539,202.9,-76.0139789775538));
#41858=CARTESIAN_POINT('Origin',(-76.0139789775538,214.75,76.0139789775539));
#41859=CARTESIAN_POINT('',(-83.0139789775539,214.5,76.0139789775539));
#41860=CARTESIAN_POINT('',(-83.2639789775538,214.75,76.0139789775539));
#41861=CARTESIAN_POINT('Origin',(-76.0139789775538,214.5,76.0139789775539));
#41862=CARTESIAN_POINT('Origin',(-76.0139789775538,202.9,76.0139789775539));
#41863=CARTESIAN_POINT('',(-83.0139789775539,202.9,76.0139789775539));
#41864=CARTESIAN_POINT('Origin',(-76.0139789775538,202.9,76.0139789775539));
#41865=CARTESIAN_POINT('',(-83.0139789775539,202.9,76.0139789775539));
#41866=CARTESIAN_POINT('Origin',(76.0139789775539,214.75,76.0139789775539));
#41867=CARTESIAN_POINT('',(69.0139789775539,214.5,76.0139789775539));
#41868=CARTESIAN_POINT('',(68.7639789775538,214.75,76.0139789775539));
#41869=CARTESIAN_POINT('Origin',(76.0139789775539,214.5,76.0139789775539));
#41870=CARTESIAN_POINT('Origin',(76.0139789775539,202.9,76.0139789775539));
#41871=CARTESIAN_POINT('',(69.0139789775539,202.9,76.0139789775539));
#41872=CARTESIAN_POINT('Origin',(76.0139789775539,202.9,76.0139789775539));
#41873=CARTESIAN_POINT('',(69.0139789775539,202.9,76.0139789775539));
#41874=CARTESIAN_POINT('Origin',(76.0139789775538,214.75,-76.0139789775539));
#41875=CARTESIAN_POINT('',(69.0139789775538,214.5,-76.0139789775539));
#41876=CARTESIAN_POINT('',(68.7639789775538,214.75,-76.0139789775539));
#41877=CARTESIAN_POINT('Origin',(76.0139789775538,214.5,-76.0139789775539));
#41878=CARTESIAN_POINT('Origin',(76.0139789775538,202.9,-76.0139789775539));
#41879=CARTESIAN_POINT('',(69.0139789775538,202.9,-76.0139789775539));
#41880=CARTESIAN_POINT('Origin',(76.0139789775538,202.9,-76.0139789775539));
#41881=CARTESIAN_POINT('',(69.0139789775538,202.9,-76.0139789775539));
#41882=CARTESIAN_POINT('Origin',(-60.,190.,-139.75));
#41883=CARTESIAN_POINT('',(-67.5,190.,-140.));
#41884=CARTESIAN_POINT('Origin',(-60.,190.,-140.));
#41885=CARTESIAN_POINT('',(-67.25,190.,-139.75));
#41886=CARTESIAN_POINT('Origin',(0.,182.5,-140.));
#41887=CARTESIAN_POINT('',(-73.,201.,-140.));
#41888=CARTESIAN_POINT('',(-73.,164.,-140.));
#41889=CARTESIAN_POINT('',(-73.,191.75,-140.));
#41890=CARTESIAN_POINT('',(-71.,203.,-140.));
#41891=CARTESIAN_POINT('Origin',(-71.,201.,-140.));
#41892=CARTESIAN_POINT('',(71.,203.,-140.));
#41893=CARTESIAN_POINT('',(35.5,203.,-140.));
#41894=CARTESIAN_POINT('',(73.,201.,-140.));
#41895=CARTESIAN_POINT('Origin',(71.,201.,-140.));
#41896=CARTESIAN_POINT('',(73.,164.,-140.));
#41897=CARTESIAN_POINT('',(73.,173.25,-140.));
#41898=CARTESIAN_POINT('',(71.,162.,-140.));
#41899=CARTESIAN_POINT('Origin',(71.,164.,-140.));
#41900=CARTESIAN_POINT('',(-71.,162.,-140.));
#41901=CARTESIAN_POINT('',(-35.5,162.,-140.));
#41902=CARTESIAN_POINT('Origin',(-71.,164.,-140.));
#41903=CARTESIAN_POINT('',(52.5,190.,-140.));
#41904=CARTESIAN_POINT('Origin',(60.,190.,-140.));
#41905=CARTESIAN_POINT('Origin',(60.,190.,-139.75));
#41906=CARTESIAN_POINT('',(52.75,190.,-139.75));
#41907=CARTESIAN_POINT('Origin',(0.,60.,0.));
#41908=CARTESIAN_POINT('',(-8.57252759403147E-15,60.,-70.));
#41909=CARTESIAN_POINT('Origin',(0.,60.,0.));
#41910=CARTESIAN_POINT('',(8.327598234202E-15,62.,-68.));
#41911=CARTESIAN_POINT('Origin',(-8.327598234202E-15,60.,-68.));
#41912=CARTESIAN_POINT('Origin',(0.,62.,0.));
#41913=CARTESIAN_POINT('Origin',(0.,55.,0.));
#41914=CARTESIAN_POINT('',(0.,50.,-70.));
#41915=CARTESIAN_POINT('',(-8.57252759403147E-15,55.,-70.));
#41916=CARTESIAN_POINT('Origin',(0.,50.,0.));
#41917=CARTESIAN_POINT('Origin',(0.,62.,45.));
#41918=CARTESIAN_POINT('',(-46.5121933088198,62.,-41.0121933088198));
#41919=CARTESIAN_POINT('Origin',(-41.0121933088198,62.,-41.0121933088198));
#41920=CARTESIAN_POINT('',(-46.5121933088198,62.,41.0121933088198));
#41921=CARTESIAN_POINT('Origin',(-41.0121933088198,62.,41.0121933088198));
#41922=CARTESIAN_POINT('',(35.5121933088198,62.,41.0121933088198));
#41923=CARTESIAN_POINT('Origin',(41.0121933088198,62.,41.0121933088198));
#41924=CARTESIAN_POINT('',(35.5121933088197,62.,-41.0121933088198));
#41925=CARTESIAN_POINT('Origin',(41.0121933088197,62.,-41.0121933088198));
#41926=CARTESIAN_POINT('',(-5.51091059616309E-15,62.,-45.));
#41927=CARTESIAN_POINT('Origin',(0.,62.,0.));
#41928=CARTESIAN_POINT('Origin',(0.,50.,0.));
#41929=CARTESIAN_POINT('',(-1.6655196468404E-14,48.,-68.));
#41930=CARTESIAN_POINT('Origin',(0.,50.,-68.));
#41931=CARTESIAN_POINT('Origin',(0.,48.,0.));
#41932=CARTESIAN_POINT('Origin',(0.,48.,69.));
#41933=CARTESIAN_POINT('',(-2.75545529808154E-15,48.,-22.5));
#41934=CARTESIAN_POINT('Origin',(0.,48.,0.));
#41935=CARTESIAN_POINT('',(35.5121933088197,48.,-41.0121933088198));
#41936=CARTESIAN_POINT('Origin',(41.0121933088197,48.,-41.0121933088198));
#41937=CARTESIAN_POINT('',(35.5121933088198,48.,41.0121933088198));
#41938=CARTESIAN_POINT('Origin',(41.0121933088198,48.,41.0121933088198));
#41939=CARTESIAN_POINT('',(-46.5121933088198,48.,41.0121933088198));
#41940=CARTESIAN_POINT('Origin',(-41.0121933088198,48.,41.0121933088198));
#41941=CARTESIAN_POINT('',(-46.5121933088198,48.,-41.0121933088198));
#41942=CARTESIAN_POINT('Origin',(-41.0121933088198,48.,-41.0121933088198));
#41943=CARTESIAN_POINT('Origin',(0.,205.34240297561,0.));
#41944=CARTESIAN_POINT('',(-1.52380583888621E-14,203.928189413237,-124.428189413237));
#41945=CARTESIAN_POINT('Origin',(-1.14285437916466E-14,203.928189413237,
0.));
#41946=CARTESIAN_POINT('',(-1.51129017770466E-14,203.381241624228,-123.40620812114));
#41947=CARTESIAN_POINT('Origin',(-1.5064867177615E-14,205.34240297561,-123.013975850864));
#41948=CARTESIAN_POINT('Origin',(-1.1334676332785E-14,203.381241624228,
0.));
#41949=CARTESIAN_POINT('Origin',(0.,203.,0.));
#41950=CARTESIAN_POINT('',(-1.45893939117854E-14,202.526288399142,-119.131441995709));
#41951=CARTESIAN_POINT('',(-1.48794586096403E-14,203.,-121.5));
#41952=CARTESIAN_POINT('Origin',(-1.09420454338391E-14,202.526288399142,
0.));
#41953=CARTESIAN_POINT('Origin',(0.,204.,0.));
#41954=CARTESIAN_POINT('Origin',(0.,204.5,0.));
#41955=CARTESIAN_POINT('',(-1.52468526493845E-14,204.,-124.5));
#41956=CARTESIAN_POINT('Origin',(0.,204.487449750524,0.));
#41957=CARTESIAN_POINT('',(-1.45569142624227E-14,202.491487079295,-118.866225531784));
#41958=CARTESIAN_POINT('Origin',(-1.45413593123538E-14,204.487449750524,
-118.739209725433));
#41959=CARTESIAN_POINT('Origin',(-1.0917685696817E-14,202.491487079295,
0.));
#41960=CARTESIAN_POINT('Origin',(0.,200.75,0.));
#41961=CARTESIAN_POINT('',(-9.76218448463178E-15,200.,-79.7142857142859));
#41962=CARTESIAN_POINT('',(-1.12055182121983E-14,200.75,-91.5));
#41963=CARTESIAN_POINT('',(-36.,200.,-71.1222000991162));
#41964=CARTESIAN_POINT('Origin',(0.,200.,0.));
#41965=CARTESIAN_POINT('',(-38.4051782991124,199.196109721127,-55.));
#41966=CARTESIAN_POINT('Ctrl Pts',(-36.0000000000003,200.,-71.1222000991167));
#41967=CARTESIAN_POINT('Ctrl Pts',(-36.007998757625,200.,-71.1181513594252));
#41968=CARTESIAN_POINT('Ctrl Pts',(-36.0158673510785,199.999975166862,-71.1137294166545));
#41969=CARTESIAN_POINT('Ctrl Pts',(-36.0580820607069,199.999730794732,-71.088038844852));
#41970=CARTESIAN_POINT('Ctrl Pts',(-36.0894047422404,199.999088235995,-71.0608151548038));
#41971=CARTESIAN_POINT('Ctrl Pts',(-36.2557708347516,199.994267844983,-70.8912518979424));
#41972=CARTESIAN_POINT('Ctrl Pts',(-36.3559669090463,199.984858677538,-70.6735956916314));
#41973=CARTESIAN_POINT('Ctrl Pts',(-36.5729453400847,199.961300812392,-70.1447351250176));
#41974=CARTESIAN_POINT('Ctrl Pts',(-36.6773890334391,199.943421017973,-69.7728383598107));
#41975=CARTESIAN_POINT('Ctrl Pts',(-36.8678693651456,199.905921405603,-69.0049790361478));
#41976=CARTESIAN_POINT('Ctrl Pts',(-36.9507101031668,199.886166180182,-68.6082338248749));
#41977=CARTESIAN_POINT('Ctrl Pts',(-37.1771778906456,199.826039691768,-67.4102186809141));
#41978=CARTESIAN_POINT('Ctrl Pts',(-37.2985629364648,199.784876737986,-66.6023010705812));
#41979=CARTESIAN_POINT('Ctrl Pts',(-37.6420334379314,199.656620586686,-64.0895799742341));
#41980=CARTESIAN_POINT('Ctrl Pts',(-37.8330351423798,199.560609339382,-62.2193907504963));
#41981=CARTESIAN_POINT('Ctrl Pts',(-38.1547759803838,199.374640295943,-58.5623760439489));
#41982=CARTESIAN_POINT('Ctrl Pts',(-38.2872235270282,199.284874589309,-56.783650812819));
#41983=CARTESIAN_POINT('Ctrl Pts',(-38.4051782991123,199.196109721127,-55.));
#41984=CARTESIAN_POINT('',(-47.,199.531133844866,-55.));
#41985=CARTESIAN_POINT('Ctrl Pts',(-47.0000000000002,199.531133844866,-55.));
#41986=CARTESIAN_POINT('Ctrl Pts',(-42.5403232540606,199.346764066249,-55.));
#41987=CARTESIAN_POINT('Ctrl Pts',(-38.4051782991124,199.196109721127,-55.));
#41988=CARTESIAN_POINT('Ctrl Pts',(-47.,199.531133844866,-55.));
#41989=CARTESIAN_POINT('Ctrl Pts',(-47.9409191594096,199.570032865355,-55.));
#41990=CARTESIAN_POINT('Ctrl Pts',(-48.922029941875,199.602939608104,-54.8270184848835));
#41991=CARTESIAN_POINT('Ctrl Pts',(-50.9084746105678,199.65289333989,-54.073774081225));
#41992=CARTESIAN_POINT('Ctrl Pts',(-51.8888445983889,199.666147836552,-53.4248639005959));
#41993=CARTESIAN_POINT('Ctrl Pts',(-53.4248639005959,199.666147836552,-51.8888445983889));
#41994=CARTESIAN_POINT('Ctrl Pts',(-54.073774081225,199.65289333989,-50.9084746105678));
#41995=CARTESIAN_POINT('Ctrl Pts',(-54.8270184848835,199.602939608103,-48.922029941875));
#41996=CARTESIAN_POINT('Ctrl Pts',(-55.,199.570032865355,-47.9409191594096));
#41997=CARTESIAN_POINT('Ctrl Pts',(-55.,199.531133844866,-47.));
#41998=CARTESIAN_POINT('Origin',(0.,199.004037328772,-3.18971646165771E-15));
#41999=CARTESIAN_POINT('',(-47.,199.531133844866,55.));
#42000=CARTESIAN_POINT('Ctrl Pts',(-55.,199.531133844866,47.));
#42001=CARTESIAN_POINT('Ctrl Pts',(-55.,199.570032865355,47.9409191594096));
#42002=CARTESIAN_POINT('Ctrl Pts',(-54.8270184848835,199.602939608103,48.922029941875));
#42003=CARTESIAN_POINT('Ctrl Pts',(-54.073774081225,199.65289333989,50.9084746105678));
#42004=CARTESIAN_POINT('Ctrl Pts',(-53.4248639005959,199.666147836552,51.8888445983889));
#42005=CARTESIAN_POINT('Ctrl Pts',(-51.8888445983889,199.666147836552,53.4248639005959));
#42006=CARTESIAN_POINT('Ctrl Pts',(-50.9084746105678,199.65289333989,54.073774081225));
#42007=CARTESIAN_POINT('Ctrl Pts',(-48.922029941875,199.602939608103,54.8270184848835));
#42008=CARTESIAN_POINT('Ctrl Pts',(-47.9409191594096,199.570032865355,55.));
#42009=CARTESIAN_POINT('Ctrl Pts',(-47.,199.531133844866,55.));
#42010=CARTESIAN_POINT('',(-32.85003536606,199.004037328772,55.));
#42011=CARTESIAN_POINT('Ctrl Pts',(-32.85003536606,199.004037328772,55.));
#42012=CARTESIAN_POINT('Ctrl Pts',(-39.4954174846828,199.22088305859,55.));
#42013=CARTESIAN_POINT('Ctrl Pts',(-47.0000000000002,199.531133844866,55.));
#42014=CARTESIAN_POINT('',(32.8500353660599,199.004037328772,55.));
#42015=CARTESIAN_POINT('Origin',(-1.96137728289756E-15,199.004037328772,
0.));
#42016=CARTESIAN_POINT('',(47.,199.531133844866,55.));
#42017=CARTESIAN_POINT('Ctrl Pts',(47.0000000000002,199.531133844866,55.));
#42018=CARTESIAN_POINT('Ctrl Pts',(39.4954174846765,199.22088305859,55.));
#42019=CARTESIAN_POINT('Ctrl Pts',(32.8500353660488,199.004037328771,55.));
#42020=CARTESIAN_POINT('',(55.,199.531133844866,47.));
#42021=CARTESIAN_POINT('Ctrl Pts',(47.,199.531133844866,55.));
#42022=CARTESIAN_POINT('Ctrl Pts',(47.9409191594096,199.570032865355,55.));
#42023=CARTESIAN_POINT('Ctrl Pts',(48.922029941875,199.602939608104,54.8270184848835));
#42024=CARTESIAN_POINT('Ctrl Pts',(50.9084746105678,199.65289333989,54.073774081225));
#42025=CARTESIAN_POINT('Ctrl Pts',(51.8888445983889,199.666147836552,53.4248639005959));
#42026=CARTESIAN_POINT('Ctrl Pts',(53.4248639005959,199.666147836552,51.8888445983889));
#42027=CARTESIAN_POINT('Ctrl Pts',(54.073774081225,199.65289333989,50.9084746105678));
#42028=CARTESIAN_POINT('Ctrl Pts',(54.8270184848835,199.602939608103,48.922029941875));
#42029=CARTESIAN_POINT('Ctrl Pts',(55.,199.570032865355,47.9409191594096));
#42030=CARTESIAN_POINT('Ctrl Pts',(55.,199.531133844866,47.));
#42031=CARTESIAN_POINT('',(55.,199.004037328772,32.85003536606));
#42032=CARTESIAN_POINT('Ctrl Pts',(55.,199.004037328772,32.85003536606));
#42033=CARTESIAN_POINT('Ctrl Pts',(55.,199.22088305859,39.4954174846828));
#42034=CARTESIAN_POINT('Ctrl Pts',(55.,199.531133844866,47.0000000000002));
#42035=CARTESIAN_POINT('',(55.,199.004037328772,-32.85003536606));
#42036=CARTESIAN_POINT('Origin',(0.,199.004037328772,3.92275456579511E-15));
#42037=CARTESIAN_POINT('',(55.,199.531133844866,-47.));
#42038=CARTESIAN_POINT('Ctrl Pts',(55.,199.531133844866,-47.0000000000002));
#42039=CARTESIAN_POINT('Ctrl Pts',(55.,199.22088305859,-39.4954174846766));
#42040=CARTESIAN_POINT('Ctrl Pts',(55.,199.004037328771,-32.8500353660488));
#42041=CARTESIAN_POINT('',(47.,199.531133844866,-55.));
#42042=CARTESIAN_POINT('Ctrl Pts',(55.,199.531133844866,-47.));
#42043=CARTESIAN_POINT('Ctrl Pts',(55.,199.570032865355,-47.9409191594096));
#42044=CARTESIAN_POINT('Ctrl Pts',(54.8270184848835,199.602939608103,-48.922029941875));
#42045=CARTESIAN_POINT('Ctrl Pts',(54.073774081225,199.65289333989,-50.9084746105678));
#42046=CARTESIAN_POINT('Ctrl Pts',(53.4248639005959,199.666147836552,-51.8888445983889));
#42047=CARTESIAN_POINT('Ctrl Pts',(51.8888445983889,199.666147836552,-53.4248639005959));
#42048=CARTESIAN_POINT('Ctrl Pts',(50.9084746105678,199.65289333989,-54.073774081225));
#42049=CARTESIAN_POINT('Ctrl Pts',(48.922029941875,199.602939608103,-54.8270184848835));
#42050=CARTESIAN_POINT('Ctrl Pts',(47.9409191594096,199.570032865355,-55.));
#42051=CARTESIAN_POINT('Ctrl Pts',(47.,199.531133844866,-55.));
#42052=CARTESIAN_POINT('',(38.4051782991124,199.196109721127,-55.));
#42053=CARTESIAN_POINT('Ctrl Pts',(38.4051782991124,199.196109721127,-55.));
#42054=CARTESIAN_POINT('Ctrl Pts',(42.5403232540606,199.346764066249,-55.));
#42055=CARTESIAN_POINT('Ctrl Pts',(47.0000000000002,199.531133844866,-55.));
#42056=CARTESIAN_POINT('',(36.,200.,-71.1222000991162));
#42057=CARTESIAN_POINT('Ctrl Pts',(38.4051782991123,199.196109721126,-55.));
#42058=CARTESIAN_POINT('Ctrl Pts',(38.2872235270282,199.284874589309,-56.783650812819));
#42059=CARTESIAN_POINT('Ctrl Pts',(38.1547759803838,199.374640295943,-58.5623760439489));
#42060=CARTESIAN_POINT('Ctrl Pts',(37.8330351423798,199.560609339382,-62.2193907504964));
#42061=CARTESIAN_POINT('Ctrl Pts',(37.6420334379314,199.656620586686,-64.0895799742343));
#42062=CARTESIAN_POINT('Ctrl Pts',(37.2985629364648,199.784876737986,-66.6023010705813));
#42063=CARTESIAN_POINT('Ctrl Pts',(37.1771778906456,199.826039691768,-67.4102186809141));
#42064=CARTESIAN_POINT('Ctrl Pts',(36.9507101031668,199.886166180182,-68.608233824875));
#42065=CARTESIAN_POINT('Ctrl Pts',(36.8678693651456,199.905921405603,-69.0049790361478));
#42066=CARTESIAN_POINT('Ctrl Pts',(36.6773890334391,199.943421017973,-69.7728383598107));
#42067=CARTESIAN_POINT('Ctrl Pts',(36.5729453400847,199.961300812392,-70.1447351250176));
#42068=CARTESIAN_POINT('Ctrl Pts',(36.3559669090463,199.984858677538,-70.6735956916314));
#42069=CARTESIAN_POINT('Ctrl Pts',(36.2557708347516,199.994267844983,-70.8912518979424));
#42070=CARTESIAN_POINT('Ctrl Pts',(36.0894047422404,199.999088235995,-71.0608151548038));
#42071=CARTESIAN_POINT('Ctrl Pts',(36.0580820607069,199.999730794732,-71.088038844852));
#42072=CARTESIAN_POINT('Ctrl Pts',(36.0158673510785,199.999975166862,-71.1137294166545));
#42073=CARTESIAN_POINT('Ctrl Pts',(36.007998757625,200.,-71.1181513594252));
#42074=CARTESIAN_POINT('Ctrl Pts',(36.0000000000003,200.,-71.1222000991167));
#42075=CARTESIAN_POINT('Origin',(0.,200.,0.));
#42076=CARTESIAN_POINT('Origin',(0.,201.,0.));
#42077=CARTESIAN_POINT('',(55.,199.,32.6016382508379));
#42078=CARTESIAN_POINT('Ctrl Pts',(55.,199.,32.6016382508379));
#42079=CARTESIAN_POINT('Ctrl Pts',(55.,199.,32.6824692460632));
#42080=CARTESIAN_POINT('Ctrl Pts',(55.,199.001278753317,32.7654969801016));
#42081=CARTESIAN_POINT('Ctrl Pts',(55.,199.004037328772,32.85003536606));
#42082=CARTESIAN_POINT('',(55.,199.,-32.6016382508379));
#42083=CARTESIAN_POINT('Origin',(0.,199.,0.));
#42084=CARTESIAN_POINT('Ctrl Pts',(55.,199.004037328772,-32.85003536606));
#42085=CARTESIAN_POINT('Ctrl Pts',(55.,199.001278753317,-32.7654969801016));
#42086=CARTESIAN_POINT('Ctrl Pts',(55.,199.,-32.6824692460632));
#42087=CARTESIAN_POINT('Ctrl Pts',(55.,199.,-32.6016382508379));
#42088=CARTESIAN_POINT('Origin',(0.,199.,64.));
#42089=CARTESIAN_POINT('',(55.,199.,55.5));
#42090=CARTESIAN_POINT('Origin',(0.,201.,0.));
#42091=CARTESIAN_POINT('',(-32.6016382508379,199.,55.));
#42092=CARTESIAN_POINT('Ctrl Pts',(-32.6016382508379,199.,55.));
#42093=CARTESIAN_POINT('Ctrl Pts',(-32.6824692460632,199.,55.));
#42094=CARTESIAN_POINT('Ctrl Pts',(-32.7654969801016,199.001278753317,55.));
#42095=CARTESIAN_POINT('Ctrl Pts',(-32.85003536606,199.004037328772,55.));
#42096=CARTESIAN_POINT('',(32.6016382508379,199.,55.));
#42097=CARTESIAN_POINT('Origin',(0.,199.,0.));
#42098=CARTESIAN_POINT('Ctrl Pts',(32.8500353660599,199.004037328772,55.));
#42099=CARTESIAN_POINT('Ctrl Pts',(32.7654969801016,199.001278753317,55.));
#42100=CARTESIAN_POINT('Ctrl Pts',(32.6824692460632,199.,55.));
#42101=CARTESIAN_POINT('Ctrl Pts',(32.6016382508379,199.,55.));
#42102=CARTESIAN_POINT('Origin',(0.,199.,64.));
#42103=CARTESIAN_POINT('',(-23.5,199.,55.));
#42104=CARTESIAN_POINT('Origin',(0.,201.,0.));
#42105=CARTESIAN_POINT('Origin',(0.,199.,0.));
#42106=CARTESIAN_POINT('Origin',(0.,199.,64.));
#42107=CARTESIAN_POINT('Origin',(-73.,191.75,-138.));
#42108=CARTESIAN_POINT('',(-75.,201.,-138.));
#42109=CARTESIAN_POINT('Origin',(-73.,201.,-138.));
#42110=CARTESIAN_POINT('',(-75.,164.,-138.));
#42111=CARTESIAN_POINT('Origin',(-73.,164.,-138.));
#42112=CARTESIAN_POINT('',(-75.,191.75,-138.));
#42113=CARTESIAN_POINT('Ctrl Pts',(-73.,164.,-140.));
#42114=CARTESIAN_POINT('Ctrl Pts',(-73.,162.,-140.));
#42115=CARTESIAN_POINT('Ctrl Pts',(-71.,162.,-140.));
#42116=CARTESIAN_POINT('Ctrl Pts',(-75.,164.,-140.));
#42117=CARTESIAN_POINT('Ctrl Pts',(-75.,160.,-140.));
#42118=CARTESIAN_POINT('Ctrl Pts',(-71.,160.,-140.));
#42119=CARTESIAN_POINT('Ctrl Pts',(-75.,164.,-138.));
#42120=CARTESIAN_POINT('Ctrl Pts',(-75.,160.,-138.));
#42121=CARTESIAN_POINT('Ctrl Pts',(-71.,160.,-138.));
#42122=CARTESIAN_POINT('',(-71.,160.,-138.));
#42123=CARTESIAN_POINT('Origin',(-71.,162.,-138.));
#42124=CARTESIAN_POINT('Origin',(-71.,164.,-138.));
#42125=CARTESIAN_POINT('Origin',(-35.5,162.,-138.));
#42126=CARTESIAN_POINT('',(71.,160.,-138.));
#42127=CARTESIAN_POINT('Origin',(71.,162.,-138.));
#42128=CARTESIAN_POINT('',(-35.5,160.,-138.));
#42129=CARTESIAN_POINT('Ctrl Pts',(71.,162.,-140.));
#42130=CARTESIAN_POINT('Ctrl Pts',(73.,162.,-140.));
#42131=CARTESIAN_POINT('Ctrl Pts',(73.,164.,-140.));
#42132=CARTESIAN_POINT('Ctrl Pts',(71.,160.,-140.));
#42133=CARTESIAN_POINT('Ctrl Pts',(75.,160.,-140.));
#42134=CARTESIAN_POINT('Ctrl Pts',(75.,164.,-140.));
#42135=CARTESIAN_POINT('Ctrl Pts',(71.,160.,-138.));
#42136=CARTESIAN_POINT('Ctrl Pts',(75.,160.,-138.));
#42137=CARTESIAN_POINT('Ctrl Pts',(75.,164.,-138.));
#42138=CARTESIAN_POINT('',(75.,164.,-138.));
#42139=CARTESIAN_POINT('Origin',(73.,164.,-138.));
#42140=CARTESIAN_POINT('Origin',(71.,164.,-138.));
#42141=CARTESIAN_POINT('Origin',(73.,173.25,-138.));
#42142=CARTESIAN_POINT('',(75.,201.,-138.));
#42143=CARTESIAN_POINT('Origin',(73.,201.,-138.));
#42144=CARTESIAN_POINT('',(75.,173.25,-138.));
#42145=CARTESIAN_POINT('Ctrl Pts',(73.,201.,-140.));
#42146=CARTESIAN_POINT('Ctrl Pts',(73.,203.,-140.));
#42147=CARTESIAN_POINT('Ctrl Pts',(71.,203.,-140.));
#42148=CARTESIAN_POINT('Ctrl Pts',(75.,201.,-140.));
#42149=CARTESIAN_POINT('Ctrl Pts',(75.,205.,-140.));
#42150=CARTESIAN_POINT('Ctrl Pts',(71.,205.,-140.));
#42151=CARTESIAN_POINT('Ctrl Pts',(75.,201.,-138.));
#42152=CARTESIAN_POINT('Ctrl Pts',(75.,205.,-138.));
#42153=CARTESIAN_POINT('Ctrl Pts',(71.,205.,-138.));
#42154=CARTESIAN_POINT('',(71.,205.,-138.));
#42155=CARTESIAN_POINT('Origin',(71.,203.,-138.));
#42156=CARTESIAN_POINT('Origin',(71.,201.,-138.));
#42157=CARTESIAN_POINT('Origin',(35.5,203.,-138.));
#42158=CARTESIAN_POINT('',(-71.,205.,-138.));
#42159=CARTESIAN_POINT('Origin',(-71.,203.,-138.));
#42160=CARTESIAN_POINT('',(35.5,205.,-138.));
#42161=CARTESIAN_POINT('Ctrl Pts',(-71.,203.,-140.));
#42162=CARTESIAN_POINT('Ctrl Pts',(-73.,203.,-140.));
#42163=CARTESIAN_POINT('Ctrl Pts',(-73.,201.,-140.));
#42164=CARTESIAN_POINT('Ctrl Pts',(-71.,205.,-140.));
#42165=CARTESIAN_POINT('Ctrl Pts',(-75.,205.,-140.));
#42166=CARTESIAN_POINT('Ctrl Pts',(-75.,201.,-140.));
#42167=CARTESIAN_POINT('Ctrl Pts',(-71.,205.,-138.));
#42168=CARTESIAN_POINT('Ctrl Pts',(-75.,205.,-138.));
#42169=CARTESIAN_POINT('Ctrl Pts',(-75.,201.,-138.));
#42170=CARTESIAN_POINT('Origin',(-71.,201.,-138.));
#42171=CARTESIAN_POINT('Origin',(71.,201.,-140.));
#42172=CARTESIAN_POINT('',(71.,205.,-140.));
#42173=CARTESIAN_POINT('',(75.,201.,-140.));
#42174=CARTESIAN_POINT('Origin',(71.,205.,-140.));
#42175=CARTESIAN_POINT('',(-71.,205.,-140.));
#42176=CARTESIAN_POINT('Origin',(-71.,201.,-140.));
#42177=CARTESIAN_POINT('',(-75.,201.,-140.));
#42178=CARTESIAN_POINT('Origin',(-75.,201.,-140.));
#42179=CARTESIAN_POINT('',(-75.,164.,-140.));
#42180=CARTESIAN_POINT('Origin',(0.,213.,0.));
#42181=CARTESIAN_POINT('',(-1.53080849893419E-14,213.,-125.));
#42182=CARTESIAN_POINT('Origin',(-1.50631556295124E-14,213.,-123.));
#42183=CARTESIAN_POINT('Origin',(0.,213.,0.));
#42184=CARTESIAN_POINT('Origin',(0.,209.75,0.));
#42185=CARTESIAN_POINT('',(-1.53080849893419E-14,209.75,-125.));
#42186=CARTESIAN_POINT('',(0.,209.75,-125.));
#42187=CARTESIAN_POINT('Origin',(0.,205.,0.));
#42188=CARTESIAN_POINT('',(0.,203.,-47.));
#42189=CARTESIAN_POINT('Origin',(0.,203.,0.));
#42190=CARTESIAN_POINT('',(-5.51091059616309E-15,205.,-45.));
#42191=CARTESIAN_POINT('Origin',(-5.75583995599256E-15,205.,-47.));
#42192=CARTESIAN_POINT('Origin',(0.,205.,0.));
#42193=CARTESIAN_POINT('',(47.,203.,0.));
#42194=CARTESIAN_POINT('Origin',(0.,203.,0.));
#42195=CARTESIAN_POINT('',(0.,203.,47.));
#42196=CARTESIAN_POINT('Origin',(0.,203.,0.));
#42197=CARTESIAN_POINT('Origin',(0.,203.,0.));
#42198=CARTESIAN_POINT('Origin',(0.,203.,0.));
#42199=CARTESIAN_POINT('',(47.,203.,41.));
#42200=CARTESIAN_POINT('',(47.,203.,-41.));
#42201=CARTESIAN_POINT('',(41.,203.,47.));
#42202=CARTESIAN_POINT('Origin',(41.,203.,41.));
#42203=CARTESIAN_POINT('',(41.,203.,47.));
#42204=CARTESIAN_POINT('Origin',(0.,203.,0.));
#42205=CARTESIAN_POINT('',(41.,203.,-47.));
#42206=CARTESIAN_POINT('',(-41.,203.,-47.));
#42207=CARTESIAN_POINT('',(47.,203.,-41.));
#42208=CARTESIAN_POINT('Origin',(41.,203.,-41.));
#42209=CARTESIAN_POINT('',(47.,203.,-41.));
#42210=CARTESIAN_POINT('Origin',(0.,203.,0.));
#42211=CARTESIAN_POINT('',(-41.,203.,-47.));
#42212=CARTESIAN_POINT('Origin',(0.,203.,0.));
#42213=CARTESIAN_POINT('',(-41.,203.,47.));
#42214=CARTESIAN_POINT('',(41.,203.,47.));
#42215=CARTESIAN_POINT('Origin',(-41.,203.,41.));
#42216=CARTESIAN_POINT('Origin',(0.,207.,0.));
#42217=CARTESIAN_POINT('',(5.51091059616309E-15,209.,-45.));
#42218=CARTESIAN_POINT('Origin',(0.,209.,0.));
#42219=CARTESIAN_POINT('',(-5.51091059616309E-15,207.,-45.));
#42220=CARTESIAN_POINT('Origin',(0.,213.,0.));
#42221=CARTESIAN_POINT('',(-1.10340676603177E-14,213.,90.1));
#42222=CARTESIAN_POINT('Origin',(-1.12789970201471E-14,213.,92.1));
#42223=CARTESIAN_POINT('',(1.10340676603177E-14,213.,-90.1));
#42224=CARTESIAN_POINT('Origin',(0.,213.,0.));
#42225=CARTESIAN_POINT('Origin',(0.,213.,0.));
#42226=CARTESIAN_POINT('Origin',(0.,213.05,0.));
#42227=CARTESIAN_POINT('',(-1.10340676603177E-14,211.,-90.1));
#42228=CARTESIAN_POINT('Origin',(0.,211.,0.));
#42229=CARTESIAN_POINT('',(-1.10340676603177E-14,213.05,-90.1));
#42230=CARTESIAN_POINT('Origin',(0.,209.,0.));
#42231=CARTESIAN_POINT('',(-5.75583995599256E-15,211.,-47.));
#42232=CARTESIAN_POINT('Origin',(-5.75583995599256E-15,209.,-47.));
#42233=CARTESIAN_POINT('Origin',(0.,211.,0.));
#42234=CARTESIAN_POINT('Origin',(0.,211.,90.1));
#42235=CARTESIAN_POINT('Origin',(53.,139.,32.));
#42236=CARTESIAN_POINT('',(55.,148.,32.));
#42237=CARTESIAN_POINT('',(53.,148.,30.));
#42238=CARTESIAN_POINT('Origin',(53.,148.,32.));
#42239=CARTESIAN_POINT('',(53.,186.,30.));
#42240=CARTESIAN_POINT('',(53.,139.,30.));
#42241=CARTESIAN_POINT('',(55.,186.,32.));
#42242=CARTESIAN_POINT('Origin',(53.,186.,32.));
#42243=CARTESIAN_POINT('',(55.,139.,32.));
#42244=CARTESIAN_POINT('Origin',(53.,186.,24.));
#42245=CARTESIAN_POINT('',(53.,192.,24.));
#42246=CARTESIAN_POINT('',(55.,194.,24.));
#42247=CARTESIAN_POINT('Origin',(53.,194.,24.));
#42248=CARTESIAN_POINT('Origin',(55.,186.,24.));
#42249=CARTESIAN_POINT('Origin',(53.,186.,24.));
#42250=CARTESIAN_POINT('Origin',(53.,194.,35.5));
#42251=CARTESIAN_POINT('',(53.,192.,-24.));
#42252=CARTESIAN_POINT('',(55.,194.,-24.));
#42253=CARTESIAN_POINT('Origin',(53.,194.,-24.));
#42254=CARTESIAN_POINT('',(55.,194.,35.5));
#42255=CARTESIAN_POINT('',(53.,192.,35.5));
#42256=CARTESIAN_POINT('Origin',(53.,186.,-24.));
#42257=CARTESIAN_POINT('',(53.,186.,-30.));
#42258=CARTESIAN_POINT('',(55.,186.,-32.));
#42259=CARTESIAN_POINT('Origin',(53.,186.,-32.));
#42260=CARTESIAN_POINT('Origin',(55.,186.,-24.));
#42261=CARTESIAN_POINT('Origin',(53.,186.,-24.));
#42262=CARTESIAN_POINT('Origin',(53.,158.,-32.));
#42263=CARTESIAN_POINT('',(53.,148.,-30.));
#42264=CARTESIAN_POINT('',(55.,148.,-32.));
#42265=CARTESIAN_POINT('Origin',(53.,148.,-32.));
#42266=CARTESIAN_POINT('',(55.,158.,-32.));
#42267=CARTESIAN_POINT('',(53.,158.,-30.));
#42268=CARTESIAN_POINT('Origin',(53.,148.,-24.));
#42269=CARTESIAN_POINT('',(53.,142.,-24.));
#42270=CARTESIAN_POINT('',(55.,140.,-24.));
#42271=CARTESIAN_POINT('Origin',(53.,140.,-24.));
#42272=CARTESIAN_POINT('Origin',(55.,148.,-24.));
#42273=CARTESIAN_POINT('Origin',(53.,148.,-24.));
#42274=CARTESIAN_POINT('Origin',(53.,140.,11.5));
#42275=CARTESIAN_POINT('',(53.,142.,24.));
#42276=CARTESIAN_POINT('',(55.,140.,24.));
#42277=CARTESIAN_POINT('Origin',(53.,140.,24.));
#42278=CARTESIAN_POINT('',(55.,140.,11.5));
#42279=CARTESIAN_POINT('',(53.,142.,11.5));
#42280=CARTESIAN_POINT('Origin',(53.,148.,24.));
#42281=CARTESIAN_POINT('Origin',(55.,148.,24.));
#42282=CARTESIAN_POINT('Origin',(53.,148.,24.));
#42283=CARTESIAN_POINT('Origin',(55.,186.,-24.));
#42284=CARTESIAN_POINT('',(49.,192.,-24.));
#42285=CARTESIAN_POINT('',(55.,192.,-24.));
#42286=CARTESIAN_POINT('',(49.,186.,-30.));
#42287=CARTESIAN_POINT('Origin',(49.,186.,-24.));
#42288=CARTESIAN_POINT('',(55.,186.,-30.));
#42289=CARTESIAN_POINT('Origin',(55.,192.,24.));
#42290=CARTESIAN_POINT('',(49.,192.,24.));
#42291=CARTESIAN_POINT('',(55.,192.,24.));
#42292=CARTESIAN_POINT('',(49.,192.,32.5));
#42293=CARTESIAN_POINT('Origin',(55.,186.,24.));
#42294=CARTESIAN_POINT('',(49.,186.,30.));
#42295=CARTESIAN_POINT('',(55.,186.,30.));
#42296=CARTESIAN_POINT('Origin',(49.,186.,24.));
#42297=CARTESIAN_POINT('Origin',(55.,148.,30.));
#42298=CARTESIAN_POINT('',(49.,148.,30.));
#42299=CARTESIAN_POINT('',(55.,148.,30.));
#42300=CARTESIAN_POINT('',(49.,141.,30.));
#42301=CARTESIAN_POINT('Origin',(55.,130.,47.));
#42302=CARTESIAN_POINT('',(55.,132.,-47.));
#42303=CARTESIAN_POINT('',(55.,132.,47.));
#42304=CARTESIAN_POINT('',(55.,132.,23.5));
#42305=CARTESIAN_POINT('',(55.,130.,-47.));
#42306=CARTESIAN_POINT('',(55.,130.,47.));
#42307=CARTESIAN_POINT('Origin',(49.,141.,32.));
#42308=CARTESIAN_POINT('',(47.,186.,32.));
#42309=CARTESIAN_POINT('Origin',(49.,186.,32.));
#42310=CARTESIAN_POINT('',(47.,148.,32.));
#42311=CARTESIAN_POINT('Origin',(49.,148.,32.));
#42312=CARTESIAN_POINT('',(47.,141.,32.));
#42313=CARTESIAN_POINT('Origin',(49.,148.,24.));
#42314=CARTESIAN_POINT('',(49.,142.,24.));
#42315=CARTESIAN_POINT('',(47.,140.,24.));
#42316=CARTESIAN_POINT('Origin',(49.,140.,24.));
#42317=CARTESIAN_POINT('Origin',(47.,148.,24.));
#42318=CARTESIAN_POINT('Origin',(49.,148.,24.));
#42319=CARTESIAN_POINT('Origin',(49.,140.,8.5));
#42320=CARTESIAN_POINT('',(49.,142.,-24.));
#42321=CARTESIAN_POINT('',(47.,140.,-24.));
#42322=CARTESIAN_POINT('Origin',(49.,140.,-24.));
#42323=CARTESIAN_POINT('',(47.,140.,8.5));
#42324=CARTESIAN_POINT('',(49.,142.,8.5));
#42325=CARTESIAN_POINT('Origin',(49.,148.,-24.));
#42326=CARTESIAN_POINT('',(49.,148.,-30.));
#42327=CARTESIAN_POINT('',(47.,148.,-32.));
#42328=CARTESIAN_POINT('Origin',(49.,148.,-32.));
#42329=CARTESIAN_POINT('Origin',(47.,148.,-24.));
#42330=CARTESIAN_POINT('Origin',(49.,148.,-24.));
#42331=CARTESIAN_POINT('Origin',(49.,160.,-32.));
#42332=CARTESIAN_POINT('',(47.,186.,-32.));
#42333=CARTESIAN_POINT('Origin',(49.,186.,-32.));
#42334=CARTESIAN_POINT('',(47.,160.,-32.));
#42335=CARTESIAN_POINT('',(49.,160.,-30.));
#42336=CARTESIAN_POINT('Origin',(49.,186.,-24.));
#42337=CARTESIAN_POINT('',(47.,194.,-24.));
#42338=CARTESIAN_POINT('Origin',(49.,194.,-24.));
#42339=CARTESIAN_POINT('Origin',(47.,186.,-24.));
#42340=CARTESIAN_POINT('Origin',(49.,194.,32.5));
#42341=CARTESIAN_POINT('',(47.,194.,24.));
#42342=CARTESIAN_POINT('Origin',(49.,194.,24.));
#42343=CARTESIAN_POINT('',(47.,194.,32.5));
#42344=CARTESIAN_POINT('Origin',(49.,186.,24.));
#42345=CARTESIAN_POINT('Origin',(47.,186.,24.));
#42346=CARTESIAN_POINT('Origin',(55.,148.,-24.));
#42347=CARTESIAN_POINT('',(55.,148.,-30.));
#42348=CARTESIAN_POINT('',(55.,142.,-24.));
#42349=CARTESIAN_POINT('Origin',(55.,142.,-24.));
#42350=CARTESIAN_POINT('',(55.,142.,24.));
#42351=CARTESIAN_POINT('Origin',(55.,148.,24.));
#42352=CARTESIAN_POINT('Origin',(47.,134.,41.));
#42353=CARTESIAN_POINT('',(47.,134.,41.));
#42354=CARTESIAN_POINT('',(47.,134.,-41.));
#42355=CARTESIAN_POINT('Origin',(-53.,132.,-23.5));
#42356=CARTESIAN_POINT('',(-53.,130.,47.));
#42357=CARTESIAN_POINT('Origin',(-53.,132.,47.));
#42358=CARTESIAN_POINT('',(-53.,130.,-47.));
#42359=CARTESIAN_POINT('Origin',(-53.,132.,-47.));
#42360=CARTESIAN_POINT('',(-53.,130.,-23.5));
#42361=CARTESIAN_POINT('Origin',(-47.,132.,-47.));
#42362=CARTESIAN_POINT('',(-47.,132.,-55.));
#42363=CARTESIAN_POINT('',(-47.,130.,-53.));
#42364=CARTESIAN_POINT('Origin',(-47.,132.,-53.));
#42365=CARTESIAN_POINT('Origin',(-47.,130.,-47.));
#42366=CARTESIAN_POINT('Origin',(-47.,132.,-47.));
#42367=CARTESIAN_POINT('Origin',(23.5,132.,-53.));
#42368=CARTESIAN_POINT('',(47.,132.,-55.));
#42369=CARTESIAN_POINT('',(47.,130.,-53.));
#42370=CARTESIAN_POINT('Origin',(47.,132.,-53.));
#42371=CARTESIAN_POINT('',(23.5,130.,-53.));
#42372=CARTESIAN_POINT('',(23.5,132.,-55.));
#42373=CARTESIAN_POINT('Origin',(47.,132.,-47.));
#42374=CARTESIAN_POINT('',(53.,130.,-47.));
#42375=CARTESIAN_POINT('Origin',(53.,132.,-47.));
#42376=CARTESIAN_POINT('Origin',(47.,130.,-47.));
#42377=CARTESIAN_POINT('Origin',(47.,132.,-47.));
#42378=CARTESIAN_POINT('Origin',(53.,132.,23.5));
#42379=CARTESIAN_POINT('',(53.,130.,47.));
#42380=CARTESIAN_POINT('Origin',(53.,132.,47.));
#42381=CARTESIAN_POINT('',(53.,130.,23.5));
#42382=CARTESIAN_POINT('Origin',(47.,132.,47.));
#42383=CARTESIAN_POINT('',(47.,132.,55.));
#42384=CARTESIAN_POINT('',(47.,130.,53.));
#42385=CARTESIAN_POINT('Origin',(47.,132.,53.));
#42386=CARTESIAN_POINT('Origin',(47.,130.,47.));
#42387=CARTESIAN_POINT('Origin',(47.,132.,47.));
#42388=CARTESIAN_POINT('Origin',(-23.5,132.,53.));
#42389=CARTESIAN_POINT('',(-47.,132.,55.));
#42390=CARTESIAN_POINT('',(-47.,130.,53.));
#42391=CARTESIAN_POINT('Origin',(-47.,132.,53.));
#42392=CARTESIAN_POINT('',(-23.5,130.,53.));
#42393=CARTESIAN_POINT('',(-23.5,132.,55.));
#42394=CARTESIAN_POINT('Origin',(-47.,132.,47.));
#42395=CARTESIAN_POINT('Origin',(-47.,132.,47.));
#42396=CARTESIAN_POINT('Origin',(-47.,130.,47.));
#42397=CARTESIAN_POINT('Origin',(47.,130.,-47.));
#42398=CARTESIAN_POINT('',(47.,130.,-55.));
#42399=CARTESIAN_POINT('Origin',(47.,130.,-55.));
#42400=CARTESIAN_POINT('',(-47.,130.,-55.));
#42401=CARTESIAN_POINT('',(-40.,196.,-55.));
#42402=CARTESIAN_POINT('Origin',(-36.,196.,-55.));
#42403=CARTESIAN_POINT('',(-40.,169.,-55.));
#42404=CARTESIAN_POINT('',(-40.,163.,-55.));
#42405=CARTESIAN_POINT('',(-36.,165.,-55.));
#42406=CARTESIAN_POINT('Origin',(-36.,169.,-55.));
#42407=CARTESIAN_POINT('',(36.,165.,-55.));
#42408=CARTESIAN_POINT('',(5.5,165.,-55.));
#42409=CARTESIAN_POINT('',(40.,169.,-55.));
#42410=CARTESIAN_POINT('Origin',(36.,169.,-55.));
#42411=CARTESIAN_POINT('',(40.,196.,-55.));
#42412=CARTESIAN_POINT('',(40.,149.5,-55.));
#42413=CARTESIAN_POINT('Origin',(36.,196.,-55.));
#42414=CARTESIAN_POINT('Origin',(-47.,130.,-47.));
#42415=CARTESIAN_POINT('Origin',(0.,130.,0.));
#42416=CARTESIAN_POINT('',(4.9326051632324E-15,130.,-40.2777777777778));
#42417=CARTESIAN_POINT('Origin',(0.,130.,0.));
#42418=CARTESIAN_POINT('Origin',(-53.,194.,-35.5));
#42419=CARTESIAN_POINT('',(-53.,192.,-24.));
#42420=CARTESIAN_POINT('Origin',(-53.,194.,-24.));
#42421=CARTESIAN_POINT('',(-53.,192.,24.));
#42422=CARTESIAN_POINT('',(-53.,192.,-35.5));
#42423=CARTESIAN_POINT('Origin',(-53.,194.,24.));
#42424=CARTESIAN_POINT('Origin',(-53.,186.,24.));
#42425=CARTESIAN_POINT('',(-53.,186.,30.));
#42426=CARTESIAN_POINT('Origin',(-53.,186.,32.));
#42427=CARTESIAN_POINT('Origin',(-53.,186.,24.));
#42428=CARTESIAN_POINT('Origin',(-53.,158.,32.));
#42429=CARTESIAN_POINT('',(-53.,148.,30.));
#42430=CARTESIAN_POINT('Origin',(-53.,148.,32.));
#42431=CARTESIAN_POINT('',(-53.,158.,30.));
#42432=CARTESIAN_POINT('Origin',(-53.,148.,24.));
#42433=CARTESIAN_POINT('',(-53.,142.,24.));
#42434=CARTESIAN_POINT('Origin',(-53.,140.,24.));
#42435=CARTESIAN_POINT('Origin',(-53.,148.,24.));
#42436=CARTESIAN_POINT('Origin',(-53.,140.,-11.5));
#42437=CARTESIAN_POINT('',(-53.,142.,-24.));
#42438=CARTESIAN_POINT('Origin',(-53.,140.,-24.));
#42439=CARTESIAN_POINT('',(-53.,142.,-11.5));
#42440=CARTESIAN_POINT('Origin',(-53.,148.,-24.));
#42441=CARTESIAN_POINT('',(-53.,148.,-30.));
#42442=CARTESIAN_POINT('Origin',(-53.,148.,-32.));
#42443=CARTESIAN_POINT('Origin',(-53.,148.,-24.));
#42444=CARTESIAN_POINT('Origin',(-53.,139.,-32.));
#42445=CARTESIAN_POINT('',(-53.,186.,-30.));
#42446=CARTESIAN_POINT('Origin',(-53.,186.,-32.));
#42447=CARTESIAN_POINT('',(-53.,139.,-30.));
#42448=CARTESIAN_POINT('Origin',(-53.,186.,-24.));
#42449=CARTESIAN_POINT('Origin',(-53.,186.,-24.));
#42450=CARTESIAN_POINT('Origin',(-55.,148.,24.));
#42451=CARTESIAN_POINT('',(-49.,148.,30.));
#42452=CARTESIAN_POINT('',(-55.,148.,30.));
#42453=CARTESIAN_POINT('',(-49.,142.,24.));
#42454=CARTESIAN_POINT('Origin',(-49.,148.,24.));
#42455=CARTESIAN_POINT('',(-55.,142.,24.));
#42456=CARTESIAN_POINT('Origin',(-55.,186.,30.));
#42457=CARTESIAN_POINT('',(-49.,186.,30.));
#42458=CARTESIAN_POINT('',(-55.,186.,30.));
#42459=CARTESIAN_POINT('',(-49.,160.,30.));
#42460=CARTESIAN_POINT('Origin',(-55.,186.,24.));
#42461=CARTESIAN_POINT('',(-49.,192.,24.));
#42462=CARTESIAN_POINT('',(-55.,192.,24.));
#42463=CARTESIAN_POINT('Origin',(-49.,186.,24.));
#42464=CARTESIAN_POINT('Origin',(-55.,192.,-24.));
#42465=CARTESIAN_POINT('',(-49.,192.,-24.));
#42466=CARTESIAN_POINT('',(-55.,192.,-24.));
#42467=CARTESIAN_POINT('',(-49.,192.,-32.5));
#42468=CARTESIAN_POINT('Origin',(-49.,194.,-32.5));
#42469=CARTESIAN_POINT('Origin',(-49.,194.,24.));
#42470=CARTESIAN_POINT('Origin',(-49.,194.,-24.));
#42471=CARTESIAN_POINT('Origin',(-49.,186.,-24.));
#42472=CARTESIAN_POINT('',(-49.,186.,-30.));
#42473=CARTESIAN_POINT('Origin',(-49.,186.,-32.));
#42474=CARTESIAN_POINT('Origin',(-49.,186.,-24.));
#42475=CARTESIAN_POINT('Origin',(-49.,141.,-32.));
#42476=CARTESIAN_POINT('',(-49.,148.,-30.));
#42477=CARTESIAN_POINT('Origin',(-49.,148.,-32.));
#42478=CARTESIAN_POINT('',(-49.,141.,-30.));
#42479=CARTESIAN_POINT('Origin',(-49.,148.,-24.));
#42480=CARTESIAN_POINT('',(-49.,142.,-24.));
#42481=CARTESIAN_POINT('Origin',(-49.,140.,-24.));
#42482=CARTESIAN_POINT('Origin',(-49.,148.,-24.));
#42483=CARTESIAN_POINT('Origin',(-49.,140.,-8.5));
#42484=CARTESIAN_POINT('Origin',(-49.,140.,24.));
#42485=CARTESIAN_POINT('',(-49.,142.,-8.5));
#42486=CARTESIAN_POINT('Origin',(-49.,148.,24.));
#42487=CARTESIAN_POINT('Origin',(-49.,148.,32.));
#42488=CARTESIAN_POINT('Origin',(-49.,160.,32.));
#42489=CARTESIAN_POINT('Origin',(-49.,186.,32.));
#42490=CARTESIAN_POINT('Origin',(-49.,186.,24.));
#42491=CARTESIAN_POINT('Origin',(-55.,148.,-24.));
#42492=CARTESIAN_POINT('',(-55.,142.,-24.));
#42493=CARTESIAN_POINT('',(-55.,148.,-30.));
#42494=CARTESIAN_POINT('Origin',(-55.,148.,-30.));
#42495=CARTESIAN_POINT('',(-55.,186.,-30.));
#42496=CARTESIAN_POINT('Origin',(-55.,186.,-24.));
#42497=CARTESIAN_POINT('Origin',(-76.0139789775539,202.9,-76.0139789775538));
#42498=CARTESIAN_POINT('Origin',(-76.0139789775538,202.9,76.0139789775539));
#42499=CARTESIAN_POINT('Origin',(76.0139789775539,202.9,76.0139789775539));
#42500=CARTESIAN_POINT('Origin',(76.0139789775538,202.9,-76.0139789775539));
#42501=CARTESIAN_POINT('Origin',(-41.0121933088198,62.1,-41.0121933088198));
#42502=CARTESIAN_POINT('',(-46.5121933088198,62.1,-41.0121933088198));
#42503=CARTESIAN_POINT('Origin',(-41.0121933088198,62.1,41.0121933088198));
#42504=CARTESIAN_POINT('',(-46.5121933088198,62.1,41.0121933088198));
#42505=CARTESIAN_POINT('Origin',(41.0121933088198,62.1,41.0121933088198));
#42506=CARTESIAN_POINT('',(35.5121933088198,62.1,41.0121933088198));
#42507=CARTESIAN_POINT('Origin',(41.0121933088197,62.1,-41.0121933088198));
#42508=CARTESIAN_POINT('',(35.5121933088197,62.1,-41.0121933088198));
#42509=CARTESIAN_POINT('Origin',(-55.,142.,24.));
#42510=CARTESIAN_POINT('Origin',(55.,186.,-30.));
#42511=CARTESIAN_POINT('Origin',(0.,128.,27.5));
#42512=CARTESIAN_POINT('',(-3.36777869765522E-15,128.,-27.5));
#42513=CARTESIAN_POINT('Origin',(0.,128.,0.));
#42514=CARTESIAN_POINT('',(-3.18530632458227E-15,128.,-26.01));
#42515=CARTESIAN_POINT('Origin',(0.,128.,0.));
#42516=CARTESIAN_POINT('Origin',(0.,129.075,0.));
#42517=CARTESIAN_POINT('',(-3.36777869765522E-15,129.075,-27.5));
#42518=CARTESIAN_POINT('Origin',(0.,66.,26.01));
#42519=CARTESIAN_POINT('',(-3.18530632458227E-15,66.,-26.01));
#42520=CARTESIAN_POINT('Origin',(0.,66.,0.));
#42521=CARTESIAN_POINT('',(-2.75545529808154E-15,66.,-22.5));
#42522=CARTESIAN_POINT('Origin',(0.,66.,0.));
#42523=CARTESIAN_POINT('Origin',(0.,100.05,0.));
#42524=CARTESIAN_POINT('',(-3.18530632458227E-15,100.05,-26.01));
#42525=CARTESIAN_POINT('Origin',(41.,134.,41.));
#42526=CARTESIAN_POINT('',(41.,134.,47.));
#42527=CARTESIAN_POINT('Origin',(-41.,134.,47.));
#42528=CARTESIAN_POINT('',(-41.,134.,47.));
#42529=CARTESIAN_POINT('Origin',(-41.,134.,41.));
#42530=CARTESIAN_POINT('Origin',(41.,134.,-47.));
#42531=CARTESIAN_POINT('',(41.,134.,-47.));
#42532=CARTESIAN_POINT('Origin',(41.,134.,-41.));
#42533=CARTESIAN_POINT('Origin',(75.,164.,-140.));
#42534=CARTESIAN_POINT('',(75.,164.,-140.));
#42535=CARTESIAN_POINT('Origin',(71.,164.,-140.));
#42536=CARTESIAN_POINT('',(71.,160.,-140.));
#42537=CARTESIAN_POINT('Origin',(-71.,160.,-140.));
#42538=CARTESIAN_POINT('',(-71.,160.,-140.));
#42539=CARTESIAN_POINT('Origin',(-71.,164.,-140.));
#42540=CARTESIAN_POINT('Origin',(-36.,165.,-125.));
#42541=CARTESIAN_POINT('',(-36.,165.,-125.));
#42542=CARTESIAN_POINT('',(36.,165.,-125.));
#42543=CARTESIAN_POINT('Origin',(-36.,169.,-125.));
#42544=CARTESIAN_POINT('',(-40.,169.,-125.));
#42545=CARTESIAN_POINT('Origin',(-40.,196.,-125.));
#42546=CARTESIAN_POINT('',(-40.,196.,-125.));
#42547=CARTESIAN_POINT('Origin',(-36.,196.,-125.));
#42548=CARTESIAN_POINT('',(-36.,200.,-125.));
#42549=CARTESIAN_POINT('Origin',(36.,200.,-125.));
#42550=CARTESIAN_POINT('',(36.,200.,-125.));
#42551=CARTESIAN_POINT('Origin',(36.,196.,-125.));
#42552=CARTESIAN_POINT('',(40.,196.,-125.));
#42553=CARTESIAN_POINT('Origin',(40.,169.,-125.));
#42554=CARTESIAN_POINT('',(40.,169.,-125.));
#42555=CARTESIAN_POINT('Origin',(36.,169.,-125.));
#42556=CARTESIAN_POINT('Origin',(-47.,130.,55.));
#42557=CARTESIAN_POINT('',(47.,130.,55.));
#42558=CARTESIAN_POINT('',(-47.,130.,55.));
#42559=CARTESIAN_POINT('Origin',(-47.,130.,47.));
#42560=CARTESIAN_POINT('Origin',(47.,130.,47.));
#42561=CARTESIAN_POINT('Origin',(0.,91.,0.));
#42562=CARTESIAN_POINT('',(-2.75545529808154E-15,91.,-22.5));
#42563=CARTESIAN_POINT('Origin',(0.,98.,0.));
#42564=CARTESIAN_POINT('',(-5.20474889637625E-15,98.,-42.5));
#42565=CARTESIAN_POINT('',(0.,0.,0.));
#42566=CARTESIAN_POINT('Origin',(-11.5124520292426,4.75,-29.3401518343476));
#42567=CARTESIAN_POINT('',(-30.6706202195582,4.95,-62.9230725199241));
#42568=CARTESIAN_POINT('',(-31.0304893797597,4.55,-62.7463841894704));
#42569=CARTESIAN_POINT('Origin',(0.,0.0499999999999893,0.));
#42570=CARTESIAN_POINT('',(-24.60288568297,4.55,-51.613448015713));
#42571=CARTESIAN_POINT('',(-11.6856571099995,4.55,-29.2401518343476));
#42572=CARTESIAN_POINT('',(-24.0564755214562,4.95,-51.4670378541992));
#42573=CARTESIAN_POINT('',(-19.6210007919903,8.19699285765687,-50.2785559823902));
#42574=CARTESIAN_POINT('',(-11.3392469484857,4.95,-29.4401518343476));
#42575=CARTESIAN_POINT('Origin',(-31.60288568297,4.95,-63.7378036686952));
#42576=CARTESIAN_POINT('',(-31.0304893797597,0.75,-62.7463841894704));
#42577=CARTESIAN_POINT('',(-31.0304893797597,0.,-62.7463841894704));
#42578=CARTESIAN_POINT('',(-24.60288568297,0.75,-51.613448015713));
#42579=CARTESIAN_POINT('',(-31.60288568297,0.75,-63.7378036686952));
#42580=CARTESIAN_POINT('',(-24.60288568297,4.95,-51.613448015713));
#42581=CARTESIAN_POINT('Origin',(0.,0.,0.));
#42582=CARTESIAN_POINT('',(-26.2383050414052,4.95,-64.8964663795662));
#42583=CARTESIAN_POINT('Origin',(0.,4.95,0.));
#42584=CARTESIAN_POINT('',(-25.8662005535307,4.55,-65.0456737141259));
#42585=CARTESIAN_POINT('Origin',(0.,0.0499999999999791,0.));
#42586=CARTESIAN_POINT('',(-25.8662005535307,0.75,-65.0456737141259));
#42587=CARTESIAN_POINT('',(-25.8662005535307,0.,-65.0456737141259));
#42588=CARTESIAN_POINT('',(-17.3066919068743,0.75,-67.8268266635004));
#42589=CARTESIAN_POINT('Origin',(0.,0.75,0.));
#42590=CARTESIAN_POINT('',(-17.3066919068743,4.55,-67.8268266635004));
#42591=CARTESIAN_POINT('',(-17.3066919068743,0.,-67.8268266635004));
#42592=CARTESIAN_POINT('',(-16.9179511817127,4.95,-67.9248329244407));
#42593=CARTESIAN_POINT('Origin',(0.,0.0500000000000549,0.));
#42594=CARTESIAN_POINT('',(-12.1722010704987,4.95,-68.9335732506255));
#42595=CARTESIAN_POINT('Origin',(0.,4.95,0.));
#42596=CARTESIAN_POINT('',(-11.7772060092513,4.55,-69.0021551737021));
#42597=CARTESIAN_POINT('Origin',(0.,0.0500000000000049,0.));
#42598=CARTESIAN_POINT('',(-11.7772060092513,0.75,-69.0021551737021));
#42599=CARTESIAN_POINT('',(-11.7772060092513,0.,-69.0021551737021));
#42600=CARTESIAN_POINT('',(-2.82650895093685,0.75,-69.9429113431109));
#42601=CARTESIAN_POINT('Origin',(0.,0.75,0.));
#42602=CARTESIAN_POINT('',(-2.82650895093685,4.55,-69.9429113431109));
#42603=CARTESIAN_POINT('',(-2.82650895093685,0.,-69.9429113431109));
#42604=CARTESIAN_POINT('',(-2.42588649588962,4.95,-69.9579521906485));
#42605=CARTESIAN_POINT('Origin',(0.,0.0499999999999979,0.));
#42606=CARTESIAN_POINT('',(-8.57252759403147E-15,4.95000000000004,-70.));
#42607=CARTESIAN_POINT('Origin',(0.,4.95,0.));
#42608=CARTESIAN_POINT('',(-8.57252759403147E-15,-4.95000000000002,-70.));
#42609=CARTESIAN_POINT('',(-8.57252759403147E-15,0.,-70.));
#42610=CARTESIAN_POINT('',(-2.42588649588962,-4.95,-69.9579521906485));
#42611=CARTESIAN_POINT('Origin',(0.,-4.95,0.));
#42612=CARTESIAN_POINT('',(-2.82650895093685,-4.55,-69.9429113431109));
#42613=CARTESIAN_POINT('Origin',(0.,-0.0500000000000168,0.));
#42614=CARTESIAN_POINT('',(-2.82650895093685,-0.75,-69.9429113431109));
#42615=CARTESIAN_POINT('',(-2.82650895093685,0.,-69.9429113431109));
#42616=CARTESIAN_POINT('',(-11.7772060092513,-0.75,-69.0021551737021));
#42617=CARTESIAN_POINT('Origin',(0.,-0.75,0.));
#42618=CARTESIAN_POINT('',(-11.7772060092513,-4.55,-69.0021551737021));
#42619=CARTESIAN_POINT('',(-11.7772060092513,0.,-69.0021551737021));
#42620=CARTESIAN_POINT('',(-12.1722010704987,-4.95,-68.9335732506255));
#42621=CARTESIAN_POINT('Origin',(0.,-0.0499999999999852,0.));
#42622=CARTESIAN_POINT('',(-16.9179511817127,-4.95,-67.9248329244407));
#42623=CARTESIAN_POINT('Origin',(0.,-4.95,0.));
#42624=CARTESIAN_POINT('',(-17.3066919068743,-4.55,-67.8268266635004));
#42625=CARTESIAN_POINT('Origin',(0.,-0.0500000000000244,0.));
#42626=CARTESIAN_POINT('',(-17.3066919068743,-0.75,-67.8268266635004));
#42627=CARTESIAN_POINT('',(-17.3066919068743,0.,-67.8268266635004));
#42628=CARTESIAN_POINT('',(-25.8662005535307,-0.75,-65.0456737141259));
#42629=CARTESIAN_POINT('Origin',(0.,-0.75,0.));
#42630=CARTESIAN_POINT('',(-25.8662005535307,-4.55,-65.0456737141259));
#42631=CARTESIAN_POINT('',(-25.8662005535307,0.,-65.0456737141259));
#42632=CARTESIAN_POINT('',(-26.2383050414052,-4.95,-64.8964663795662));
#42633=CARTESIAN_POINT('Origin',(0.,-0.0500000000000249,0.));
#42634=CARTESIAN_POINT('',(-30.6706202195582,-4.95,-62.9230725199241));
#42635=CARTESIAN_POINT('Origin',(0.,-4.95,0.));
#42636=CARTESIAN_POINT('',(-31.0304893797597,-4.55,-62.7463841894704));
#42637=CARTESIAN_POINT('Origin',(0.,-0.0500000000000491,0.));
#42638=CARTESIAN_POINT('',(-31.0304893797597,-0.75,-62.7463841894704));
#42639=CARTESIAN_POINT('',(-31.0304893797597,0.,-62.7463841894704));
#42640=CARTESIAN_POINT('',(-38.8247180138197,-0.75,-58.2463841894704));
#42641=CARTESIAN_POINT('Origin',(0.,-0.75,0.));
#42642=CARTESIAN_POINT('',(-38.8247180138197,-4.55,-58.2463841894704));
#42643=CARTESIAN_POINT('',(-38.8247180138197,0.,-58.2463841894704));
#42644=CARTESIAN_POINT('',(-39.1576691766457,-4.95,-58.0230725199241));
#42645=CARTESIAN_POINT('Origin',(0.,-0.0500000000000088,0.));
#42646=CARTESIAN_POINT('',(-43.0828359798445,-4.95,-55.1712719078853));
#42647=CARTESIAN_POINT('Origin',(0.,-4.95,0.));
#42648=CARTESIAN_POINT('',(-43.3981055659413,-4.55,-54.9236236358037));
#42649=CARTESIAN_POINT('Origin',(0.,-0.0499999999998519,0.));
#42650=CARTESIAN_POINT('',(-43.3981055659413,-0.75,-54.9236236358037));
#42651=CARTESIAN_POINT('',(-43.3981055659413,0.,-54.9236236358037));
#42652=CARTESIAN_POINT('',(-50.0864089952379,-0.75,-48.901448178574));
#42653=CARTESIAN_POINT('Origin',(0.,-0.75,0.));
#42654=CARTESIAN_POINT('',(-50.0864089952379,-4.55,-48.901448178574));
#42655=CARTESIAN_POINT('',(-50.0864089952379,0.,-48.901448178574));
#42656=CARTESIAN_POINT('',(-50.3656552695229,-4.95,-48.6137919655685));
#42657=CARTESIAN_POINT('Origin',(0.,-0.0499999999999022,0.));
#42658=CARTESIAN_POINT('',(-53.6121250734278,-4.95,-45.0082219723368));
#42659=CARTESIAN_POINT('Origin',(0.,-4.95,0.));
#42660=CARTESIAN_POINT('',(-53.8690162916761,-4.55,-44.7004371764654));
#42661=CARTESIAN_POINT('Origin',(0.,-0.0499999999999979,0.));
#42662=CARTESIAN_POINT('',(-53.8690162916761,-0.75,-44.7004371764654));
#42663=CARTESIAN_POINT('',(-53.8690162916761,0.,-44.7004371764654));
#42664=CARTESIAN_POINT('',(-59.1590835623084,-0.75,-37.4192842270909));
#42665=CARTESIAN_POINT('Origin',(0.,-0.75,0.));
#42666=CARTESIAN_POINT('',(-59.1590835623084,-4.55,-37.4192842270909));
#42667=CARTESIAN_POINT('',(-59.1590835623084,0.,-37.4192842270909));
#42668=CARTESIAN_POINT('',(-59.372420545894,-4.95,-37.0798554274623));
#42669=CARTESIAN_POINT('Origin',(0.,-0.0500000000000306,0.));
#42670=CARTESIAN_POINT('',(-61.7983070417836,-4.95,-32.8780967631862));
#42671=CARTESIAN_POINT('Origin',(0.,-4.95,0.));
#42672=CARTESIAN_POINT('',(-61.9855925132453,-4.55,-32.5236271160201));
#42673=CARTESIAN_POINT('Origin',(0.,-0.0499999999998472,0.));
#42674=CARTESIAN_POINT('',(-61.9855925132453,-0.75,-32.5236271160201));
#42675=CARTESIAN_POINT('',(-61.9855925132453,0.,-32.5236271160201));
#42676=CARTESIAN_POINT('',(-65.6462223009275,-0.75,-24.3017179972367));
#42677=CARTESIAN_POINT('Origin',(0.,-0.75,0.));
#42678=CARTESIAN_POINT('',(-65.6462223009274,-4.55,-24.3017179972366));
#42679=CARTESIAN_POINT('',(-65.6462223009274,0.,-24.3017179972366));
#42680=CARTESIAN_POINT('',(-65.7843261439265,-4.95,-23.9253512782887));
#42681=CARTESIAN_POINT('Origin',(0.,-0.049999999999976,0.));
#42682=CARTESIAN_POINT('',(-67.2836064512356,-4.95,-19.3110409588722));
#42683=CARTESIAN_POINT('Origin',(0.,-4.95,0.));
#42684=CARTESIAN_POINT('',(-67.3931009021123,-4.55,-18.9253784849265));
#42685=CARTESIAN_POINT('Origin',(0.,-0.0500000000000752,0.));
#42686=CARTESIAN_POINT('',(-67.3931009021122,-0.75,-18.9253784849265));
#42687=CARTESIAN_POINT('',(-67.3931009021123,0.,-18.9253784849265));
#42688=CARTESIAN_POINT('',(-69.2643061194721,-0.75,-10.1220500783223));
#42689=CARTESIAN_POINT('Origin',(0.,-0.75,0.));
#42690=CARTESIAN_POINT('',(-69.2643061194721,-4.55,-10.1220500783223));
#42691=CARTESIAN_POINT('',(-69.2643061194721,0.,-10.1220500783223));
#42692=CARTESIAN_POINT('',(-69.3211410212497,-4.95,-9.72519447168095));
#42693=CARTESIAN_POINT('Origin',(0.,-0.0499999999999407,0.));
#42694=CARTESIAN_POINT('',(-69.8282893962039,-4.95,-4.90000000000001));
#42695=CARTESIAN_POINT('Origin',(0.,-4.95,0.));
#42696=CARTESIAN_POINT('',(-69.8552073935795,-4.55,-4.50000000000001));
#42697=CARTESIAN_POINT('Origin',(0.,-0.0500000000000236,0.));
#42698=CARTESIAN_POINT('',(-69.8552073935795,-0.75,-4.50000000000001));
#42699=CARTESIAN_POINT('',(-69.8552073935795,0.,-4.50000000000001));
#42700=CARTESIAN_POINT('',(-69.8552073935795,-0.75,4.49999999999999));
#42701=CARTESIAN_POINT('Origin',(0.,-0.75,0.));
#42702=CARTESIAN_POINT('',(-69.8552073935795,-4.55,4.49999999999999));
#42703=CARTESIAN_POINT('',(-69.8552073935795,0.,4.49999999999999));
#42704=CARTESIAN_POINT('',(-69.8282893962039,-4.95,4.89999999999999));
#42705=CARTESIAN_POINT('Origin',(0.,-0.0500000000000182,0.));
#42706=CARTESIAN_POINT('',(-69.3211410212497,-4.95,9.7251944716809));
#42707=CARTESIAN_POINT('Origin',(0.,-4.95,0.));
#42708=CARTESIAN_POINT('',(-69.2643061194721,-4.55,10.1220500783222));
#42709=CARTESIAN_POINT('Origin',(0.,-0.0500000000000127,0.));
#42710=CARTESIAN_POINT('',(-69.2643061194721,-0.75,10.1220500783222));
#42711=CARTESIAN_POINT('',(-69.2643061194721,0.,10.1220500783222));
#42712=CARTESIAN_POINT('',(-67.3931009021123,-0.75,18.9253784849265));
#42713=CARTESIAN_POINT('Origin',(0.,-0.75,0.));
#42714=CARTESIAN_POINT('',(-67.3931009021123,-4.55,18.9253784849265));
#42715=CARTESIAN_POINT('',(-67.3931009021123,0.,18.9253784849265));
#42716=CARTESIAN_POINT('',(-67.2836064512357,-4.95,19.3110409588722));
#42717=CARTESIAN_POINT('Origin',(0.,-0.0500000000000002,0.));
#42718=CARTESIAN_POINT('',(-65.7843261439265,-4.95,23.9253512782887));
#42719=CARTESIAN_POINT('Origin',(0.,-4.95,0.));
#42720=CARTESIAN_POINT('',(-65.6462223009275,-4.55,24.3017179972366));
#42721=CARTESIAN_POINT('Origin',(0.,-0.0500000000000877,0.));
#42722=CARTESIAN_POINT('',(-65.6462223009275,-0.75,24.3017179972366));
#42723=CARTESIAN_POINT('',(-65.6462223009275,0.,24.3017179972366));
#42724=CARTESIAN_POINT('',(-61.9855925132453,-0.75,32.52362711602));
#42725=CARTESIAN_POINT('Origin',(0.,-0.75,0.));
#42726=CARTESIAN_POINT('',(-61.9855925132453,-4.55,32.52362711602));
#42727=CARTESIAN_POINT('',(-61.9855925132453,0.,32.52362711602));
#42728=CARTESIAN_POINT('',(-61.7983070417837,-4.95,32.8780967631862));
#42729=CARTESIAN_POINT('Origin',(0.,-0.0500000000000174,0.));
#42730=CARTESIAN_POINT('',(-59.372420545894,-4.95,37.0798554274623));
#42731=CARTESIAN_POINT('Origin',(0.,-4.95,0.));
#42732=CARTESIAN_POINT('',(-59.1590835623084,-4.55,37.4192842270909));
#42733=CARTESIAN_POINT('Origin',(0.,-0.0500000000000454,0.));
#42734=CARTESIAN_POINT('',(-59.1590835623084,-0.75,37.4192842270909));
#42735=CARTESIAN_POINT('',(-59.1590835623084,0.,37.4192842270909));
#42736=CARTESIAN_POINT('',(-53.8690162916761,-0.75,44.7004371764654));
#42737=CARTESIAN_POINT('Origin',(0.,-0.75,0.));
#42738=CARTESIAN_POINT('',(-53.8690162916761,-4.55,44.7004371764654));
#42739=CARTESIAN_POINT('',(-53.8690162916761,0.,44.7004371764654));
#42740=CARTESIAN_POINT('',(-53.6121250734278,-4.95,45.0082219723368));
#42741=CARTESIAN_POINT('Origin',(0.,-0.0499999999999049,0.));
#42742=CARTESIAN_POINT('',(-50.365655269523,-4.95,48.6137919655685));
#42743=CARTESIAN_POINT('Origin',(0.,-4.95,0.));
#42744=CARTESIAN_POINT('',(-50.0864089952379,-4.55,48.9014481785739));
#42745=CARTESIAN_POINT('Origin',(0.,-0.0499999999999206,0.));
#42746=CARTESIAN_POINT('',(-50.0864089952379,-0.75,48.9014481785739));
#42747=CARTESIAN_POINT('',(-50.0864089952379,0.,48.9014481785739));
#42748=CARTESIAN_POINT('',(-43.3981055659414,-0.75,54.9236236358036));
#42749=CARTESIAN_POINT('Origin',(0.,-0.75,0.));
#42750=CARTESIAN_POINT('',(-43.3981055659414,-4.55,54.9236236358036));
#42751=CARTESIAN_POINT('',(-43.3981055659414,0.,54.9236236358036));
#42752=CARTESIAN_POINT('',(-43.0828359798445,-4.95,55.1712719078853));
#42753=CARTESIAN_POINT('Origin',(0.,-0.0499999999999237,0.));
#42754=CARTESIAN_POINT('',(-39.1576691766457,-4.95,58.0230725199241));
#42755=CARTESIAN_POINT('Origin',(0.,-4.95,0.));
#42756=CARTESIAN_POINT('',(-38.8247180138197,-4.55,58.2463841894704));
#42757=CARTESIAN_POINT('Origin',(0.,-0.0500000000000736,0.));
#42758=CARTESIAN_POINT('',(-38.8247180138197,-0.75,58.2463841894704));
#42759=CARTESIAN_POINT('',(-38.8247180138197,0.,58.2463841894704));
#42760=CARTESIAN_POINT('',(-31.0304893797598,-0.75,62.7463841894704));
#42761=CARTESIAN_POINT('Origin',(0.,-0.75,0.));
#42762=CARTESIAN_POINT('',(-31.0304893797598,-4.55,62.7463841894704));
#42763=CARTESIAN_POINT('',(-31.0304893797598,0.,62.7463841894704));
#42764=CARTESIAN_POINT('',(-30.6706202195582,-4.95,62.9230725199241));
#42765=CARTESIAN_POINT('Origin',(0.,-0.0500000000000798,0.));
#42766=CARTESIAN_POINT('',(-26.2383050414052,-4.95,64.8964663795662));
#42767=CARTESIAN_POINT('Origin',(0.,-4.95,0.));
#42768=CARTESIAN_POINT('',(-25.8662005535307,-4.55,65.0456737141259));
#42769=CARTESIAN_POINT('Origin',(0.,-0.0500000000000174,0.));
#42770=CARTESIAN_POINT('',(-25.8662005535307,-0.75,65.0456737141259));
#42771=CARTESIAN_POINT('',(-25.8662005535307,0.,65.0456737141259));
#42772=CARTESIAN_POINT('',(-17.3066919068743,-0.75,67.8268266635004));
#42773=CARTESIAN_POINT('Origin',(0.,-0.75,0.));
#42774=CARTESIAN_POINT('',(-17.3066919068744,-4.55,67.8268266635004));
#42775=CARTESIAN_POINT('',(-17.3066919068744,0.,67.8268266635004));
#42776=CARTESIAN_POINT('',(-16.9179511817127,-4.95,67.9248329244407));
#42777=CARTESIAN_POINT('Origin',(0.,-0.0500000000000237,0.));
#42778=CARTESIAN_POINT('',(-12.1722010704988,-4.95,68.9335732506255));
#42779=CARTESIAN_POINT('Origin',(0.,-4.95,0.));
#42780=CARTESIAN_POINT('',(-11.7772060092514,-4.55,69.002155173702));
#42781=CARTESIAN_POINT('Origin',(0.,-0.0499999999999869,0.));
#42782=CARTESIAN_POINT('',(-11.7772060092514,-0.75,69.002155173702));
#42783=CARTESIAN_POINT('',(-11.7772060092514,0.,69.002155173702));
#42784=CARTESIAN_POINT('',(-2.82650895093691,-0.75,69.9429113431109));
#42785=CARTESIAN_POINT('Origin',(0.,-0.75,0.));
#42786=CARTESIAN_POINT('',(-2.82650895093691,-4.55,69.9429113431109));
#42787=CARTESIAN_POINT('',(-2.82650895093691,0.,69.9429113431109));
#42788=CARTESIAN_POINT('',(-2.42588649588969,-4.95,69.9579521906485));
#42789=CARTESIAN_POINT('Origin',(0.,-0.0499999999999861,0.));
#42790=CARTESIAN_POINT('',(2.4258864958896,-4.95,69.9579521906485));
#42791=CARTESIAN_POINT('Origin',(0.,-4.95,0.));
#42792=CARTESIAN_POINT('',(2.82650895093682,-4.55,69.9429113431109));
#42793=CARTESIAN_POINT('Origin',(0.,-0.049999999999976,0.));
#42794=CARTESIAN_POINT('',(2.82650895093682,-0.75,69.9429113431109));
#42795=CARTESIAN_POINT('',(2.82650895093682,0.,69.9429113431109));
#42796=CARTESIAN_POINT('',(11.7772060092513,-0.75,69.0021551737021));
#42797=CARTESIAN_POINT('Origin',(0.,-0.75,0.));
#42798=CARTESIAN_POINT('',(11.7772060092513,-4.55,69.0021551737021));
#42799=CARTESIAN_POINT('',(11.7772060092513,0.,69.0021551737021));
#42800=CARTESIAN_POINT('',(12.1722010704987,-4.95,68.9335732506255));
#42801=CARTESIAN_POINT('Origin',(0.,-0.0499999999999893,0.));
#42802=CARTESIAN_POINT('',(16.9179511817127,-4.95,67.9248329244407));
#42803=CARTESIAN_POINT('Origin',(0.,-4.95,0.));
#42804=CARTESIAN_POINT('',(17.3066919068743,-4.55,67.8268266635004));
#42805=CARTESIAN_POINT('Origin',(0.,-0.0500000000000205,0.));
#42806=CARTESIAN_POINT('',(17.3066919068743,-0.75,67.8268266635004));
#42807=CARTESIAN_POINT('',(17.3066919068743,0.,67.8268266635004));
#42808=CARTESIAN_POINT('',(25.8662005535307,-0.75,65.0456737141259));
#42809=CARTESIAN_POINT('Origin',(0.,-0.75,0.));
#42810=CARTESIAN_POINT('',(25.8662005535307,-4.55,65.0456737141259));
#42811=CARTESIAN_POINT('',(25.8662005535307,0.,65.0456737141259));
#42812=CARTESIAN_POINT('',(26.2383050414052,-4.95,64.8964663795662));
#42813=CARTESIAN_POINT('Origin',(0.,-0.0499999999999705,0.));
#42814=CARTESIAN_POINT('',(30.6706202195581,-4.95,62.9230725199241));
#42815=CARTESIAN_POINT('Origin',(0.,-4.95,0.));
#42816=CARTESIAN_POINT('',(31.0304893797597,-4.55,62.7463841894704));
#42817=CARTESIAN_POINT('Origin',(0.,-0.0500000000000393,0.));
#42818=CARTESIAN_POINT('',(31.0304893797597,-0.75,62.7463841894704));
#42819=CARTESIAN_POINT('',(31.0304893797597,0.,62.7463841894704));
#42820=CARTESIAN_POINT('',(38.8247180138197,-0.75,58.2463841894704));
#42821=CARTESIAN_POINT('Origin',(0.,-0.75,0.));
#42822=CARTESIAN_POINT('',(38.8247180138197,-4.55,58.2463841894704));
#42823=CARTESIAN_POINT('',(38.8247180138197,0.,58.2463841894704));
#42824=CARTESIAN_POINT('',(39.1576691766456,-4.95,58.0230725199241));
#42825=CARTESIAN_POINT('Origin',(0.,-0.0499999999998987,0.));
#42826=CARTESIAN_POINT('',(43.0828359798445,-4.95,55.1712719078853));
#42827=CARTESIAN_POINT('Origin',(0.,-4.95,0.));
#42828=CARTESIAN_POINT('',(43.3981055659413,-4.55,54.9236236358037));
#42829=CARTESIAN_POINT('Origin',(0.,-0.0499999999999174,0.));
#42830=CARTESIAN_POINT('',(43.3981055659413,-0.75,54.9236236358037));
#42831=CARTESIAN_POINT('',(43.3981055659413,0.,54.9236236358037));
#42832=CARTESIAN_POINT('',(50.0864089952379,-0.75,48.901448178574));
#42833=CARTESIAN_POINT('Origin',(0.,-0.75,0.));
#42834=CARTESIAN_POINT('',(50.0864089952379,-4.55,48.901448178574));
#42835=CARTESIAN_POINT('',(50.0864089952379,0.,48.901448178574));
#42836=CARTESIAN_POINT('',(50.3656552695229,-4.95,48.6137919655685));
#42837=CARTESIAN_POINT('Origin',(0.,-0.0499999999999612,0.));
#42838=CARTESIAN_POINT('',(53.6121250734277,-4.95,45.0082219723368));
#42839=CARTESIAN_POINT('Origin',(0.,-4.95,0.));
#42840=CARTESIAN_POINT('',(53.8690162916761,-4.55,44.7004371764654));
#42841=CARTESIAN_POINT('Origin',(0.,-0.0500000000000486,0.));
#42842=CARTESIAN_POINT('',(53.8690162916761,-0.75,44.7004371764654));
#42843=CARTESIAN_POINT('',(53.8690162916761,0.,44.7004371764654));
#42844=CARTESIAN_POINT('',(59.1590835623084,-0.75,37.4192842270909));
#42845=CARTESIAN_POINT('Origin',(0.,-0.75,0.));
#42846=CARTESIAN_POINT('',(59.1590835623084,-4.55,37.4192842270909));
#42847=CARTESIAN_POINT('',(59.1590835623084,0.,37.4192842270909));
#42848=CARTESIAN_POINT('',(59.372420545894,-4.95,37.0798554274623));
#42849=CARTESIAN_POINT('Origin',(0.,-0.0500000000000174,0.));
#42850=CARTESIAN_POINT('',(61.7983070417836,-4.95,32.8780967631863));
#42851=CARTESIAN_POINT('Origin',(0.,-4.95,0.));
#42852=CARTESIAN_POINT('',(61.9855925132452,-4.55,32.5236271160201));
#42853=CARTESIAN_POINT('Origin',(0.,-0.0500000000001204,0.));
#42854=CARTESIAN_POINT('',(61.9855925132452,-0.75,32.5236271160201));
#42855=CARTESIAN_POINT('',(61.9855925132452,0.,32.5236271160201));
#42856=CARTESIAN_POINT('',(65.6462223009274,-0.75,24.3017179972367));
#42857=CARTESIAN_POINT('Origin',(0.,-0.75,0.));
#42858=CARTESIAN_POINT('',(65.6462223009274,-4.55,24.3017179972367));
#42859=CARTESIAN_POINT('',(65.6462223009274,0.,24.3017179972367));
#42860=CARTESIAN_POINT('',(65.7843261439265,-4.95,23.9253512782888));
#42861=CARTESIAN_POINT('Origin',(0.,-0.049999999999905,0.));
#42862=CARTESIAN_POINT('',(67.2836064512356,-4.95,19.3110409588723));
#42863=CARTESIAN_POINT('Origin',(0.,-4.95,0.));
#42864=CARTESIAN_POINT('',(67.3931009021122,-4.55,18.9253784849265));
#42865=CARTESIAN_POINT('Origin',(0.,-0.0500000000000127,0.));
#42866=CARTESIAN_POINT('',(67.3931009021122,-0.75,18.9253784849265));
#42867=CARTESIAN_POINT('',(67.3931009021122,0.,18.9253784849265));
#42868=CARTESIAN_POINT('',(69.2643061194721,-0.75,10.1220500783223));
#42869=CARTESIAN_POINT('Origin',(0.,-0.75,0.));
#42870=CARTESIAN_POINT('',(69.2643061194721,-4.55,10.1220500783223));
#42871=CARTESIAN_POINT('',(69.2643061194721,0.,10.1220500783223));
#42872=CARTESIAN_POINT('',(69.3211410212497,-4.95,9.72519447168096));
#42873=CARTESIAN_POINT('Origin',(0.,-0.0499999999999331,0.));
#42874=CARTESIAN_POINT('',(69.8282893962039,-4.95,4.9));
#42875=CARTESIAN_POINT('Origin',(0.,-4.95,0.));
#42876=CARTESIAN_POINT('',(69.8552073935795,-4.55,4.5));
#42877=CARTESIAN_POINT('Origin',(0.,-0.0500000000000182,0.));
#42878=CARTESIAN_POINT('',(69.8552073935795,-0.75,4.5));
#42879=CARTESIAN_POINT('',(69.8552073935795,0.,4.5));
#42880=CARTESIAN_POINT('',(69.8552073935795,-0.75,-4.5));
#42881=CARTESIAN_POINT('Origin',(0.,-0.75,0.));
#42882=CARTESIAN_POINT('',(69.8552073935795,-4.55,-4.5));
#42883=CARTESIAN_POINT('',(69.8552073935795,0.,-4.5));
#42884=CARTESIAN_POINT('',(69.8282893962039,-4.95,-4.9));
#42885=CARTESIAN_POINT('Origin',(0.,-0.0500000000000182,0.));
#42886=CARTESIAN_POINT('',(69.3211410212497,-4.95,-9.72519447168091));
#42887=CARTESIAN_POINT('Origin',(0.,-4.95,0.));
#42888=CARTESIAN_POINT('',(69.2643061194721,-4.55,-10.1220500783222));
#42889=CARTESIAN_POINT('Origin',(0.,-0.0500000000000287,0.));
#42890=CARTESIAN_POINT('',(69.2643061194721,-0.75,-10.1220500783222));
#42891=CARTESIAN_POINT('',(69.2643061194721,0.,-10.1220500783222));
#42892=CARTESIAN_POINT('',(67.3931009021123,-0.75,-18.9253784849265));
#42893=CARTESIAN_POINT('Origin',(0.,-0.75,0.));
#42894=CARTESIAN_POINT('',(67.3931009021123,-4.55,-18.9253784849265));
#42895=CARTESIAN_POINT('',(67.3931009021123,0.,-18.9253784849265));
#42896=CARTESIAN_POINT('',(67.2836064512357,-4.95,-19.3110409588722));
#42897=CARTESIAN_POINT('Origin',(0.,-0.0500000000000143,0.));
#42898=CARTESIAN_POINT('',(65.7843261439265,-4.95,-23.9253512782887));
#42899=CARTESIAN_POINT('Origin',(0.,-4.95,0.));
#42900=CARTESIAN_POINT('',(65.6462223009275,-4.55,-24.3017179972366));
#42901=CARTESIAN_POINT('Origin',(0.,-0.049999999999873,0.));
#42902=CARTESIAN_POINT('',(65.6462223009275,-0.75,-24.3017179972366));
#42903=CARTESIAN_POINT('',(65.6462223009275,0.,-24.3017179972366));
#42904=CARTESIAN_POINT('',(61.9855925132453,-0.75,-32.52362711602));
#42905=CARTESIAN_POINT('Origin',(0.,-0.75,0.));
#42906=CARTESIAN_POINT('',(61.9855925132453,-4.55,-32.52362711602));
#42907=CARTESIAN_POINT('',(61.9855925132453,0.,-32.52362711602));
#42908=CARTESIAN_POINT('',(61.7983070417836,-4.95,-32.8780967631862));
#42909=CARTESIAN_POINT('Origin',(0.,-0.0500000000002188,0.));
#42910=CARTESIAN_POINT('',(59.372420545894,-4.95,-37.0798554274623));
#42911=CARTESIAN_POINT('Origin',(0.,-4.95,0.));
#42912=CARTESIAN_POINT('',(59.1590835623084,-4.55,-37.4192842270909));
#42913=CARTESIAN_POINT('Origin',(0.,-0.0499999999999441,0.));
#42914=CARTESIAN_POINT('',(59.1590835623084,-0.75,-37.4192842270909));
#42915=CARTESIAN_POINT('',(59.1590835623084,0.,-37.4192842270909));
#42916=CARTESIAN_POINT('',(53.8690162916761,-0.75,-44.7004371764654));
#42917=CARTESIAN_POINT('Origin',(0.,-0.75,0.));
#42918=CARTESIAN_POINT('',(53.8690162916761,-4.55,-44.7004371764654));
#42919=CARTESIAN_POINT('',(53.8690162916761,0.,-44.7004371764654));
#42920=CARTESIAN_POINT('',(53.6121250734278,-4.95,-45.0082219723368));
#42921=CARTESIAN_POINT('Origin',(0.,-0.0500000000000424,0.));
#42922=CARTESIAN_POINT('',(50.365655269523,-4.95,-48.6137919655685));
#42923=CARTESIAN_POINT('Origin',(0.,-4.95,0.));
#42924=CARTESIAN_POINT('',(50.0864089952379,-4.55,-48.9014481785739));
#42925=CARTESIAN_POINT('Origin',(0.,-0.0499999999999559,0.));
#42926=CARTESIAN_POINT('',(50.0864089952379,-0.75,-48.9014481785739));
#42927=CARTESIAN_POINT('',(50.0864089952379,0.,-48.9014481785739));
#42928=CARTESIAN_POINT('',(43.3981055659414,-0.75,-54.9236236358037));
#42929=CARTESIAN_POINT('Origin',(0.,-0.75,0.));
#42930=CARTESIAN_POINT('',(43.3981055659414,-4.55,-54.9236236358037));
#42931=CARTESIAN_POINT('',(43.3981055659414,0.,-54.9236236358037));
#42932=CARTESIAN_POINT('',(43.0828359798445,-4.95,-55.1712719078853));
#42933=CARTESIAN_POINT('Origin',(0.,-0.050000000000197,0.));
#42934=CARTESIAN_POINT('',(39.1576691766457,-4.95,-58.0230725199241));
#42935=CARTESIAN_POINT('Origin',(0.,-4.95,0.));
#42936=CARTESIAN_POINT('',(38.8247180138197,-4.55,-58.2463841894704));
#42937=CARTESIAN_POINT('Origin',(0.,-0.0499999999998999,0.));
#42938=CARTESIAN_POINT('',(38.8247180138197,-0.75,-58.2463841894704));
#42939=CARTESIAN_POINT('',(38.8247180138197,0.,-58.2463841894704));
#42940=CARTESIAN_POINT('',(31.0304893797598,-0.75,-62.7463841894704));
#42941=CARTESIAN_POINT('Origin',(0.,-0.75,0.));
#42942=CARTESIAN_POINT('',(31.0304893797598,-4.55,-62.7463841894704));
#42943=CARTESIAN_POINT('',(31.0304893797598,0.,-62.7463841894704));
#42944=CARTESIAN_POINT('',(30.6706202195582,-4.95,-62.9230725199241));
#42945=CARTESIAN_POINT('Origin',(0.,-0.0499999999999463,0.));
#42946=CARTESIAN_POINT('',(26.2383050414052,-4.95,-64.8964663795662));
#42947=CARTESIAN_POINT('Origin',(0.,-4.95,0.));
#42948=CARTESIAN_POINT('',(25.8662005535307,-4.55,-65.0456737141259));
#42949=CARTESIAN_POINT('Origin',(0.,-0.0500000000000244,0.));
#42950=CARTESIAN_POINT('',(25.8662005535307,-0.75,-65.0456737141259));
#42951=CARTESIAN_POINT('',(25.8662005535307,0.,-65.0456737141259));
#42952=CARTESIAN_POINT('',(17.3066919068743,-0.75,-67.8268266635004));
#42953=CARTESIAN_POINT('Origin',(0.,-0.75,0.));
#42954=CARTESIAN_POINT('',(17.3066919068743,-4.55,-67.8268266635004));
#42955=CARTESIAN_POINT('',(17.3066919068743,0.,-67.8268266635004));
#42956=CARTESIAN_POINT('',(16.9179511817127,-4.95,-67.9248329244407));
#42957=CARTESIAN_POINT('Origin',(0.,-0.0499999999999975,0.));
#42958=CARTESIAN_POINT('',(12.1722010704987,-4.95,-68.9335732506255));
#42959=CARTESIAN_POINT('Origin',(0.,-4.95,0.));
#42960=CARTESIAN_POINT('',(11.7772060092513,-4.55,-69.002155173702));
#42961=CARTESIAN_POINT('Origin',(0.,-0.0499999999999915,0.));
#42962=CARTESIAN_POINT('',(11.7772060092513,-0.75,-69.002155173702));
#42963=CARTESIAN_POINT('',(11.7772060092513,0.,-69.002155173702));
#42964=CARTESIAN_POINT('',(2.82650895093687,-0.75,-69.9429113431109));
#42965=CARTESIAN_POINT('Origin',(0.,-0.75,0.));
#42966=CARTESIAN_POINT('',(2.82650895093687,-4.55,-69.9429113431109));
#42967=CARTESIAN_POINT('',(2.82650895093687,0.,-69.9429113431109));
#42968=CARTESIAN_POINT('',(2.42588649588965,-4.95,-69.9579521906485));
#42969=CARTESIAN_POINT('Origin',(0.,-0.0499999999999968,0.));
#42970=CARTESIAN_POINT('Origin',(0.,-4.95,0.));
#42971=CARTESIAN_POINT('',(2.42588649588965,4.95,-69.9579521906485));
#42972=CARTESIAN_POINT('Origin',(0.,4.95,0.));
#42973=CARTESIAN_POINT('',(2.82650895093687,4.55,-69.9429113431109));
#42974=CARTESIAN_POINT('Origin',(0.,0.0499999999999799,0.));
#42975=CARTESIAN_POINT('',(2.82650895093687,0.75,-69.9429113431109));
#42976=CARTESIAN_POINT('',(2.82650895093687,0.,-69.9429113431109));
#42977=CARTESIAN_POINT('',(11.7772060092513,0.75,-69.002155173702));
#42978=CARTESIAN_POINT('Origin',(0.,0.75,0.));
#42979=CARTESIAN_POINT('',(11.7772060092513,4.55,-69.002155173702));
#42980=CARTESIAN_POINT('',(11.7772060092513,0.,-69.002155173702));
#42981=CARTESIAN_POINT('',(12.1722010704987,4.95,-68.9335732506255));
#42982=CARTESIAN_POINT('Origin',(0.,0.0499999999999889,0.));
#42983=CARTESIAN_POINT('',(16.9179511817127,4.95,-67.9248329244407));
#42984=CARTESIAN_POINT('Origin',(0.,4.95,0.));
#42985=CARTESIAN_POINT('',(17.3066919068743,4.55,-67.8268266635004));
#42986=CARTESIAN_POINT('Origin',(0.,0.0499999999999752,0.));
#42987=CARTESIAN_POINT('',(17.3066919068743,0.75,-67.8268266635004));
#42988=CARTESIAN_POINT('',(17.3066919068743,0.,-67.8268266635004));
#42989=CARTESIAN_POINT('',(25.8662005535307,0.75,-65.0456737141259));
#42990=CARTESIAN_POINT('Origin',(0.,0.75,0.));
#42991=CARTESIAN_POINT('',(25.8662005535307,4.55,-65.0456737141259));
#42992=CARTESIAN_POINT('',(25.8662005535307,0.,-65.0456737141259));
#42993=CARTESIAN_POINT('',(26.2383050414052,4.95,-64.8964663795662));
#42994=CARTESIAN_POINT('Origin',(0.,0.0500000000000658,0.));
#42995=CARTESIAN_POINT('',(30.6706202195582,4.95,-62.9230725199241));
#42996=CARTESIAN_POINT('Origin',(0.,4.95,0.));
#42997=CARTESIAN_POINT('',(31.0304893797598,4.55,-62.7463841894704));
#42998=CARTESIAN_POINT('Origin',(0.,0.0499999999999612,0.));
#42999=CARTESIAN_POINT('',(31.0304893797598,0.75,-62.7463841894704));
#43000=CARTESIAN_POINT('',(31.0304893797598,0.,-62.7463841894704));
#43001=CARTESIAN_POINT('',(38.8247180138197,0.75,-58.2463841894704));
#43002=CARTESIAN_POINT('Origin',(0.,0.75,0.));
#43003=CARTESIAN_POINT('',(38.8247180138197,4.55,-58.2463841894704));
#43004=CARTESIAN_POINT('',(38.8247180138197,0.,-58.2463841894704));
#43005=CARTESIAN_POINT('',(39.1576691766457,4.95,-58.0230725199241));
#43006=CARTESIAN_POINT('Origin',(0.,0.0499999999999753,0.));
#43007=CARTESIAN_POINT('',(43.0828359798445,4.95,-55.1712719078853));
#43008=CARTESIAN_POINT('Origin',(0.,4.95,0.));
#43009=CARTESIAN_POINT('',(43.3981055659414,4.55,-54.9236236358037));
#43010=CARTESIAN_POINT('Origin',(0.,0.0499999999999174,0.));
#43011=CARTESIAN_POINT('',(43.3981055659414,0.75,-54.9236236358037));
#43012=CARTESIAN_POINT('',(43.3981055659414,0.,-54.9236236358037));
#43013=CARTESIAN_POINT('',(50.0864089952379,0.75,-48.9014481785739));
#43014=CARTESIAN_POINT('Origin',(0.,0.75,0.));
#43015=CARTESIAN_POINT('',(50.0864089952379,4.55,-48.9014481785739));
#43016=CARTESIAN_POINT('',(50.0864089952379,0.,-48.9014481785739));
#43017=CARTESIAN_POINT('',(50.365655269523,4.95,-48.6137919655685));
#43018=CARTESIAN_POINT('Origin',(0.,0.0499999999999987,0.));
#43019=CARTESIAN_POINT('',(53.6121250734278,4.95,-45.0082219723368));
#43020=CARTESIAN_POINT('Origin',(0.,4.95,0.));
#43021=CARTESIAN_POINT('',(53.8690162916761,4.55,-44.7004371764654));
#43022=CARTESIAN_POINT('Origin',(0.,0.0500000000000361,0.));
#43023=CARTESIAN_POINT('',(53.8690162916761,0.75,-44.7004371764654));
#43024=CARTESIAN_POINT('',(53.8690162916761,0.,-44.7004371764654));
#43025=CARTESIAN_POINT('',(59.1590835623084,0.75,-37.4192842270909));
#43026=CARTESIAN_POINT('Origin',(0.,0.75,0.));
#43027=CARTESIAN_POINT('',(59.1590835623084,4.55,-37.4192842270909));
#43028=CARTESIAN_POINT('',(59.1590835623084,0.,-37.4192842270909));
#43029=CARTESIAN_POINT('',(59.372420545894,4.95,-37.0798554274623));
#43030=CARTESIAN_POINT('Origin',(0.,0.0500000000000689,0.));
#43031=CARTESIAN_POINT('',(61.7983070417836,4.95,-32.8780967631862));
#43032=CARTESIAN_POINT('Origin',(0.,4.95,0.));
#43033=CARTESIAN_POINT('',(61.9855925132453,4.55,-32.52362711602));
#43034=CARTESIAN_POINT('Origin',(0.,0.0500000000000205,0.));
#43035=CARTESIAN_POINT('',(61.9855925132453,0.75,-32.52362711602));
#43036=CARTESIAN_POINT('',(61.9855925132453,0.,-32.52362711602));
#43037=CARTESIAN_POINT('',(65.6462223009275,0.75,-24.3017179972366));
#43038=CARTESIAN_POINT('Origin',(0.,0.75,0.));
#43039=CARTESIAN_POINT('',(65.6462223009275,4.55,-24.3017179972366));
#43040=CARTESIAN_POINT('',(65.6462223009275,0.,-24.3017179972366));
#43041=CARTESIAN_POINT('',(65.7843261439265,4.95,-23.9253512782887));
#43042=CARTESIAN_POINT('Origin',(0.,0.0500000000000158,0.));
#43043=CARTESIAN_POINT('',(67.2836064512357,4.95,-19.3110409588722));
#43044=CARTESIAN_POINT('Origin',(0.,4.95,0.));
#43045=CARTESIAN_POINT('',(67.3931009021123,4.55,-18.9253784849265));
#43046=CARTESIAN_POINT('Origin',(0.,0.0499999999999518,0.));
#43047=CARTESIAN_POINT('',(67.3931009021123,0.75,-18.9253784849265));
#43048=CARTESIAN_POINT('',(67.3931009021123,0.,-18.9253784849265));
#43049=CARTESIAN_POINT('',(69.2643061194721,0.75,-10.1220500783222));
#43050=CARTESIAN_POINT('Origin',(0.,0.75,0.));
#43051=CARTESIAN_POINT('',(69.2643061194721,4.55,-10.1220500783222));
#43052=CARTESIAN_POINT('',(69.2643061194721,0.,-10.1220500783222));
#43053=CARTESIAN_POINT('',(69.3211410212497,4.95,-9.72519447168092));
#43054=CARTESIAN_POINT('Origin',(0.,0.0499999999999783,0.));
#43055=CARTESIAN_POINT('',(69.8282893962039,4.95,-4.9));
#43056=CARTESIAN_POINT('Origin',(0.,4.95,0.));
#43057=CARTESIAN_POINT('',(69.8552073935795,4.55,-4.5));
#43058=CARTESIAN_POINT('Origin',(0.,0.0499999999999932,0.));
#43059=CARTESIAN_POINT('',(69.8552073935795,0.75,-4.5));
#43060=CARTESIAN_POINT('',(69.8552073935795,0.,-4.5));
#43061=CARTESIAN_POINT('',(69.8552073935795,0.75,4.5));
#43062=CARTESIAN_POINT('Origin',(0.,0.75,0.));
#43063=CARTESIAN_POINT('',(69.8552073935795,4.55,4.5));
#43064=CARTESIAN_POINT('',(69.8552073935795,0.,4.5));
#43065=CARTESIAN_POINT('',(69.8282893962039,4.95,4.9));
#43066=CARTESIAN_POINT('Origin',(0.,0.0499999999999932,0.));
#43067=CARTESIAN_POINT('',(69.3211410212497,4.95,9.72519447168096));
#43068=CARTESIAN_POINT('Origin',(0.,4.95,0.));
#43069=CARTESIAN_POINT('',(69.2643061194721,4.55,10.1220500783223));
#43070=CARTESIAN_POINT('Origin',(0.,0.0499999999999797,0.));
#43071=CARTESIAN_POINT('',(69.2643061194721,0.75,10.1220500783223));
#43072=CARTESIAN_POINT('',(69.2643061194721,0.,10.1220500783223));
#43073=CARTESIAN_POINT('',(67.3931009021122,0.75,18.9253784849265));
#43074=CARTESIAN_POINT('Origin',(0.,0.75,0.));
#43075=CARTESIAN_POINT('',(67.3931009021122,4.55,18.9253784849265));
#43076=CARTESIAN_POINT('',(67.3931009021122,0.,18.9253784849265));
#43077=CARTESIAN_POINT('',(67.2836064512356,4.95,19.3110409588723));
#43078=CARTESIAN_POINT('Origin',(0.,0.0499999999999877,0.));
#43079=CARTESIAN_POINT('',(65.7843261439265,4.95,23.9253512782888));
#43080=CARTESIAN_POINT('Origin',(0.,4.95,0.));
#43081=CARTESIAN_POINT('',(65.6462223009274,4.55,24.3017179972367));
#43082=CARTESIAN_POINT('Origin',(0.,0.0499999999999846,0.));
#43083=CARTESIAN_POINT('',(65.6462223009274,0.75,24.3017179972367));
#43084=CARTESIAN_POINT('',(65.6462223009274,0.,24.3017179972367));
#43085=CARTESIAN_POINT('',(61.9855925132452,0.75,32.5236271160201));
#43086=CARTESIAN_POINT('Origin',(0.,0.75,0.));
#43087=CARTESIAN_POINT('',(61.9855925132452,4.55,32.5236271160201));
#43088=CARTESIAN_POINT('',(61.9855925132452,0.,32.5236271160201));
#43089=CARTESIAN_POINT('',(61.7983070417836,4.95,32.8780967631863));
#43090=CARTESIAN_POINT('Origin',(0.,0.0500000000000143,0.));
#43091=CARTESIAN_POINT('',(59.372420545894,4.95,37.0798554274623));
#43092=CARTESIAN_POINT('Origin',(0.,4.95,0.));
#43093=CARTESIAN_POINT('',(59.1590835623084,4.55,37.4192842270909));
#43094=CARTESIAN_POINT('Origin',(0.,0.0500000000000002,0.));
#43095=CARTESIAN_POINT('',(59.1590835623084,0.75,37.4192842270909));
#43096=CARTESIAN_POINT('',(59.1590835623084,0.,37.4192842270909));
#43097=CARTESIAN_POINT('',(53.8690162916761,0.75,44.7004371764654));
#43098=CARTESIAN_POINT('Origin',(0.,0.75,0.));
#43099=CARTESIAN_POINT('',(53.8690162916761,4.55,44.7004371764654));
#43100=CARTESIAN_POINT('',(53.8690162916761,0.,44.7004371764654));
#43101=CARTESIAN_POINT('',(53.6121250734277,4.95,45.0082219723368));
#43102=CARTESIAN_POINT('Origin',(0.,0.0499999999999736,0.));
#43103=CARTESIAN_POINT('',(50.3656552695229,4.95,48.6137919655685));
#43104=CARTESIAN_POINT('Origin',(0.,4.95,0.));
#43105=CARTESIAN_POINT('',(50.0864089952379,4.55,48.901448178574));
#43106=CARTESIAN_POINT('Origin',(0.,0.0499999999999143,0.));
#43107=CARTESIAN_POINT('',(50.0864089952379,0.75,48.901448178574));
#43108=CARTESIAN_POINT('',(50.0864089952379,0.,48.901448178574));
#43109=CARTESIAN_POINT('',(43.3981055659413,0.75,54.9236236358037));
#43110=CARTESIAN_POINT('Origin',(0.,0.75,0.));
#43111=CARTESIAN_POINT('',(43.3981055659413,4.55,54.9236236358037));
#43112=CARTESIAN_POINT('',(43.3981055659413,0.,54.9236236358037));
#43113=CARTESIAN_POINT('',(43.0828359798445,4.95,55.1712719078853));
#43114=CARTESIAN_POINT('Origin',(0.,0.0499999999999924,0.));
#43115=CARTESIAN_POINT('',(39.1576691766456,4.95,58.0230725199241));
#43116=CARTESIAN_POINT('Origin',(0.,4.95,0.));
#43117=CARTESIAN_POINT('',(38.8247180138197,4.55,58.2463841894704));
#43118=CARTESIAN_POINT('Origin',(0.,0.0499999999999674,0.));
#43119=CARTESIAN_POINT('',(38.8247180138197,0.75,58.2463841894704));
#43120=CARTESIAN_POINT('',(38.8247180138197,0.,58.2463841894704));
#43121=CARTESIAN_POINT('',(31.0304893797597,0.75,62.7463841894704));
#43122=CARTESIAN_POINT('Origin',(0.,0.75,0.));
#43123=CARTESIAN_POINT('',(31.0304893797597,4.55,62.7463841894704));
#43124=CARTESIAN_POINT('',(31.0304893797597,0.,62.7463841894704));
#43125=CARTESIAN_POINT('',(30.6706202195581,4.95,62.9230725199241));
#43126=CARTESIAN_POINT('Origin',(0.,0.0499999999999924,0.));
#43127=CARTESIAN_POINT('',(26.2383050414052,4.95,64.8964663795662));
#43128=CARTESIAN_POINT('Origin',(0.,4.95,0.));
#43129=CARTESIAN_POINT('',(25.8662005535307,4.55,65.0456737141259));
#43130=CARTESIAN_POINT('Origin',(0.,0.0500000000000315,0.));
#43131=CARTESIAN_POINT('',(25.8662005535307,0.75,65.0456737141259));
#43132=CARTESIAN_POINT('',(25.8662005535307,0.,65.0456737141259));
#43133=CARTESIAN_POINT('',(17.3066919068743,0.75,67.8268266635004));
#43134=CARTESIAN_POINT('Origin',(0.,0.75,0.));
#43135=CARTESIAN_POINT('',(17.3066919068743,4.55,67.8268266635004));
#43136=CARTESIAN_POINT('',(17.3066919068743,0.,67.8268266635004));
#43137=CARTESIAN_POINT('',(16.9179511817127,4.95,67.9248329244407));
#43138=CARTESIAN_POINT('Origin',(0.,0.0500000000000018,0.));
#43139=CARTESIAN_POINT('',(12.1722010704987,4.95,68.9335732506255));
#43140=CARTESIAN_POINT('Origin',(0.,4.95,0.));
#43141=CARTESIAN_POINT('',(11.7772060092513,4.55,69.0021551737021));
#43142=CARTESIAN_POINT('Origin',(0.,0.0499999999999881,0.));
#43143=CARTESIAN_POINT('',(11.7772060092513,0.75,69.0021551737021));
#43144=CARTESIAN_POINT('',(11.7772060092513,0.,69.0021551737021));
#43145=CARTESIAN_POINT('',(2.82650895093682,0.75,69.9429113431109));
#43146=CARTESIAN_POINT('Origin',(0.,0.75,0.));
#43147=CARTESIAN_POINT('',(2.82650895093682,4.55,69.9429113431109));
#43148=CARTESIAN_POINT('',(2.82650895093682,0.,69.9429113431109));
#43149=CARTESIAN_POINT('',(2.4258864958896,4.95,69.9579521906485));
#43150=CARTESIAN_POINT('Origin',(0.,0.0499999999999979,0.));
#43151=CARTESIAN_POINT('',(-2.42588649588969,4.95,69.9579521906485));
#43152=CARTESIAN_POINT('Origin',(0.,4.95,0.));
#43153=CARTESIAN_POINT('',(-2.82650895093691,4.55,69.9429113431109));
#43154=CARTESIAN_POINT('Origin',(0.,0.0499999999999881,0.));
#43155=CARTESIAN_POINT('',(-2.82650895093691,0.75,69.9429113431109));
#43156=CARTESIAN_POINT('',(-2.82650895093691,0.,69.9429113431109));
#43157=CARTESIAN_POINT('',(-11.7772060092514,0.75,69.002155173702));
#43158=CARTESIAN_POINT('Origin',(0.,0.75,0.));
#43159=CARTESIAN_POINT('',(-11.7772060092514,4.55,69.002155173702));
#43160=CARTESIAN_POINT('',(-11.7772060092514,0.,69.002155173702));
#43161=CARTESIAN_POINT('',(-12.1722010704988,4.95,68.9335732506255));
#43162=CARTESIAN_POINT('Origin',(0.,0.0499999999999768,0.));
#43163=CARTESIAN_POINT('',(-16.9179511817127,4.95,67.9248329244407));
#43164=CARTESIAN_POINT('Origin',(0.,4.95,0.));
#43165=CARTESIAN_POINT('',(-17.3066919068743,4.55,67.8268266635004));
#43166=CARTESIAN_POINT('Origin',(0.,0.0500000000000018,0.));
#43167=CARTESIAN_POINT('',(-17.3066919068743,0.75,67.8268266635004));
#43168=CARTESIAN_POINT('',(-17.3066919068743,0.,67.8268266635004));
#43169=CARTESIAN_POINT('',(-25.8662005535307,0.75,65.0456737141259));
#43170=CARTESIAN_POINT('Origin',(0.,0.75,0.));
#43171=CARTESIAN_POINT('',(-25.8662005535307,4.55,65.0456737141259));
#43172=CARTESIAN_POINT('',(-25.8662005535307,0.,65.0456737141259));
#43173=CARTESIAN_POINT('',(-26.2383050414052,4.95,64.8964663795662));
#43174=CARTESIAN_POINT('Origin',(0.,0.0500000000000455,0.));
#43175=CARTESIAN_POINT('',(-30.6706202195582,4.95,62.9230725199241));
#43176=CARTESIAN_POINT('Origin',(0.,4.95,0.));
#43177=CARTESIAN_POINT('',(-31.0304893797598,4.55,62.7463841894704));
#43178=CARTESIAN_POINT('Origin',(0.,0.0499999999999643,0.));
#43179=CARTESIAN_POINT('',(-31.0304893797598,0.75,62.7463841894704));
#43180=CARTESIAN_POINT('',(-31.0304893797598,0.,62.7463841894704));
#43181=CARTESIAN_POINT('',(-38.8247180138197,0.75,58.2463841894704));
#43182=CARTESIAN_POINT('Origin',(0.,0.75,0.));
#43183=CARTESIAN_POINT('',(-38.8247180138197,4.55,58.2463841894704));
#43184=CARTESIAN_POINT('',(-38.8247180138197,0.,58.2463841894704));
#43185=CARTESIAN_POINT('',(-39.1576691766457,4.95,58.0230725199241));
#43186=CARTESIAN_POINT('Origin',(0.,0.0500000000000048,0.));
#43187=CARTESIAN_POINT('',(-43.0828359798445,4.95,55.1712719078853));
#43188=CARTESIAN_POINT('Origin',(0.,4.95,0.));
#43189=CARTESIAN_POINT('',(-43.3981055659414,4.55,54.9236236358036));
#43190=CARTESIAN_POINT('Origin',(0.,0.0499999999999487,0.));
#43191=CARTESIAN_POINT('',(-43.3981055659414,0.75,54.9236236358036));
#43192=CARTESIAN_POINT('',(-43.3981055659414,0.,54.9236236358036));
#43193=CARTESIAN_POINT('',(-50.0864089952379,0.75,48.9014481785739));
#43194=CARTESIAN_POINT('Origin',(0.,0.75,0.));
#43195=CARTESIAN_POINT('',(-50.0864089952379,4.55,48.9014481785739));
#43196=CARTESIAN_POINT('',(-50.0864089952379,0.,48.9014481785739));
#43197=CARTESIAN_POINT('',(-50.365655269523,4.95,48.6137919655685));
#43198=CARTESIAN_POINT('Origin',(0.,0.0499999999999987,0.));
#43199=CARTESIAN_POINT('',(-53.6121250734278,4.95,45.0082219723368));
#43200=CARTESIAN_POINT('Origin',(0.,4.95,0.));
#43201=CARTESIAN_POINT('',(-53.8690162916761,4.55,44.7004371764654));
#43202=CARTESIAN_POINT('Origin',(0.,0.0500000000000923,0.));
#43203=CARTESIAN_POINT('',(-53.8690162916761,0.75,44.7004371764654));
#43204=CARTESIAN_POINT('',(-53.8690162916761,0.,44.7004371764654));
#43205=CARTESIAN_POINT('',(-59.1590835623084,0.75,37.4192842270909));
#43206=CARTESIAN_POINT('Origin',(0.,0.75,0.));
#43207=CARTESIAN_POINT('',(-59.1590835623084,4.55,37.4192842270909));
#43208=CARTESIAN_POINT('',(-59.1590835623084,0.,37.4192842270909));
#43209=CARTESIAN_POINT('',(-59.372420545894,4.95,37.0798554274623));
#43210=CARTESIAN_POINT('Origin',(0.,0.0499999999999955,0.));
#43211=CARTESIAN_POINT('',(-61.7983070417837,4.95,32.8780967631862));
#43212=CARTESIAN_POINT('Origin',(0.,4.95,0.));
#43213=CARTESIAN_POINT('',(-61.9855925132453,4.55,32.52362711602));
#43214=CARTESIAN_POINT('Origin',(0.,0.0500000000000143,0.));
#43215=CARTESIAN_POINT('',(-61.9855925132453,0.75,32.52362711602));
#43216=CARTESIAN_POINT('',(-61.9855925132453,0.,32.52362711602));
#43217=CARTESIAN_POINT('',(-65.6462223009275,0.75,24.3017179972366));
#43218=CARTESIAN_POINT('Origin',(0.,0.75,0.));
#43219=CARTESIAN_POINT('',(-65.6462223009275,4.55,24.3017179972366));
#43220=CARTESIAN_POINT('',(-65.6462223009275,0.,24.3017179972366));
#43221=CARTESIAN_POINT('',(-65.7843261439265,4.95,23.9253512782887));
#43222=CARTESIAN_POINT('Origin',(0.,0.0500000000000877,0.));
#43223=CARTESIAN_POINT('',(-67.2836064512357,4.95,19.3110409588722));
#43224=CARTESIAN_POINT('Origin',(0.,4.95,0.));
#43225=CARTESIAN_POINT('',(-67.3931009021123,4.55,18.9253784849265));
#43226=CARTESIAN_POINT('Origin',(0.,0.0499999999999909,0.));
#43227=CARTESIAN_POINT('',(-67.3931009021123,0.75,18.9253784849265));
#43228=CARTESIAN_POINT('',(-67.3931009021123,0.,18.9253784849265));
#43229=CARTESIAN_POINT('',(-69.2643061194721,0.75,10.1220500783222));
#43230=CARTESIAN_POINT('Origin',(0.,0.75,0.));
#43231=CARTESIAN_POINT('',(-69.2643061194721,4.55,10.1220500783222));
#43232=CARTESIAN_POINT('',(-69.2643061194721,0.,10.1220500783222));
#43233=CARTESIAN_POINT('',(-69.3211410212497,4.95,9.7251944716809));
#43234=CARTESIAN_POINT('Origin',(0.,0.0499999999999944,0.));
#43235=CARTESIAN_POINT('',(-69.8282893962039,4.95,4.89999999999999));
#43236=CARTESIAN_POINT('Origin',(0.,4.95,0.));
#43237=CARTESIAN_POINT('',(-69.8552073935795,4.55,4.49999999999999));
#43238=CARTESIAN_POINT('Origin',(0.,0.0499999999999932,0.));
#43239=CARTESIAN_POINT('',(-69.8552073935795,0.75,4.49999999999999));
#43240=CARTESIAN_POINT('',(-69.8552073935795,0.,4.49999999999999));
#43241=CARTESIAN_POINT('',(-69.8552073935795,0.75,-4.50000000000001));
#43242=CARTESIAN_POINT('Origin',(0.,0.75,0.));
#43243=CARTESIAN_POINT('',(-69.8552073935795,4.55,-4.50000000000001));
#43244=CARTESIAN_POINT('',(-69.8552073935795,0.,-4.50000000000001));
#43245=CARTESIAN_POINT('',(-69.8282893962039,4.95,-4.90000000000001));
#43246=CARTESIAN_POINT('Origin',(0.,0.0499999999999932,0.));
#43247=CARTESIAN_POINT('',(-69.3211410212497,4.95,-9.72519447168095));
#43248=CARTESIAN_POINT('Origin',(0.,4.95,0.));
#43249=CARTESIAN_POINT('',(-69.2643061194721,4.55,-10.1220500783223));
#43250=CARTESIAN_POINT('Origin',(0.,0.0499999999999889,0.));
#43251=CARTESIAN_POINT('',(-69.2643061194721,0.75,-10.1220500783223));
#43252=CARTESIAN_POINT('',(-69.2643061194721,0.,-10.1220500783223));
#43253=CARTESIAN_POINT('',(-67.3931009021122,0.75,-18.9253784849265));
#43254=CARTESIAN_POINT('Origin',(0.,0.75,0.));
#43255=CARTESIAN_POINT('',(-67.3931009021122,4.55,-18.9253784849265));
#43256=CARTESIAN_POINT('',(-67.3931009021122,0.,-18.9253784849265));
#43257=CARTESIAN_POINT('',(-67.2836064512356,4.95,-19.3110409588722));
#43258=CARTESIAN_POINT('Origin',(0.,0.0500000000000143,0.));
#43259=CARTESIAN_POINT('',(-65.7843261439265,4.95,-23.9253512782887));
#43260=CARTESIAN_POINT('Origin',(0.,4.95,0.));
#43261=CARTESIAN_POINT('',(-65.6462223009274,4.55,-24.3017179972367));
#43262=CARTESIAN_POINT('Origin',(0.,0.0499999999999854,0.));
#43263=CARTESIAN_POINT('',(-65.6462223009275,0.75,-24.3017179972367));
#43264=CARTESIAN_POINT('',(-65.6462223009274,0.,-24.3017179972367));
#43265=CARTESIAN_POINT('',(-61.9855925132453,0.75,-32.5236271160201));
#43266=CARTESIAN_POINT('Origin',(0.,0.75,0.));
#43267=CARTESIAN_POINT('',(-61.9855925132453,4.55,-32.5236271160201));
#43268=CARTESIAN_POINT('',(-61.9855925132453,0.,-32.5236271160201));
#43269=CARTESIAN_POINT('',(-61.7983070417836,4.95,-32.8780967631862));
#43270=CARTESIAN_POINT('Origin',(0.,0.0499999999999737,0.));
#43271=CARTESIAN_POINT('',(-59.372420545894,4.95,-37.0798554274623));
#43272=CARTESIAN_POINT('Origin',(0.,4.95,0.));
#43273=CARTESIAN_POINT('',(-59.1590835623084,4.55,-37.4192842270909));
#43274=CARTESIAN_POINT('Origin',(0.,0.0499999999999986,0.));
#43275=CARTESIAN_POINT('',(-59.1590835623084,0.75,-37.4192842270909));
#43276=CARTESIAN_POINT('',(-59.1590835623084,0.,-37.4192842270909));
#43277=CARTESIAN_POINT('',(-53.8690162916761,0.75,-44.7004371764654));
#43278=CARTESIAN_POINT('Origin',(0.,0.75,0.));
#43279=CARTESIAN_POINT('',(-53.8690162916761,4.55,-44.7004371764654));
#43280=CARTESIAN_POINT('',(-53.8690162916761,0.,-44.7004371764654));
#43281=CARTESIAN_POINT('',(-53.6121250734277,4.95,-45.0082219723368));
#43282=CARTESIAN_POINT('Origin',(0.,0.0500000000000955,0.));
#43283=CARTESIAN_POINT('',(-50.3656552695229,4.95,-48.6137919655685));
#43284=CARTESIAN_POINT('Origin',(0.,4.95,0.));
#43285=CARTESIAN_POINT('',(-50.0864089952379,4.55,-48.901448178574));
#43286=CARTESIAN_POINT('Origin',(0.,0.0499999999999581,0.));
#43287=CARTESIAN_POINT('',(-50.0864089952379,0.75,-48.901448178574));
#43288=CARTESIAN_POINT('',(-50.0864089952379,0.,-48.901448178574));
#43289=CARTESIAN_POINT('',(-43.3981055659413,0.75,-54.9236236358037));
#43290=CARTESIAN_POINT('Origin',(0.,0.75,0.));
#43291=CARTESIAN_POINT('',(-43.3981055659413,4.55,-54.9236236358037));
#43292=CARTESIAN_POINT('',(-43.3981055659413,0.,-54.9236236358037));
#43293=CARTESIAN_POINT('',(-43.0828359798445,4.95,-55.1712719078853));
#43294=CARTESIAN_POINT('Origin',(0.,0.0499999999999987,0.));
#43295=CARTESIAN_POINT('',(-39.1576691766457,4.95,-58.0230725199241));
#43296=CARTESIAN_POINT('Origin',(0.,4.95,0.));
#43297=CARTESIAN_POINT('',(-38.8247180138197,4.55,-58.2463841894704));
#43298=CARTESIAN_POINT('Origin',(0.,0.0499999999999831,0.));
#43299=CARTESIAN_POINT('',(-38.8247180138197,0.75,-58.2463841894704));
#43300=CARTESIAN_POINT('',(-38.8247180138197,0.,-58.2463841894704));
#43301=CARTESIAN_POINT('Origin',(0.,0.75,0.));
#43302=CARTESIAN_POINT('Origin',(-11.8060173724113,4.75,-21.1256658124263));
#43303=CARTESIAN_POINT('',(-21.8937230027002,4.55,-52.8196449541365));
#43304=CARTESIAN_POINT('',(-11.6158060691523,4.55,-21.1874692113013));
#43305=CARTESIAN_POINT('',(-22.1505388114683,4.95,-52.3156155498685));
#43306=CARTESIAN_POINT('',(-11.9962286756703,4.95,-21.0638624135513));
#43307=CARTESIAN_POINT('',(-22.1505388114683,4.95,-52.3156155498685));
#43308=CARTESIAN_POINT('Origin',(-16.8832207126948,4.75,-54.2373633913317));
#43309=CARTESIAN_POINT('',(-12.8301849517758,4.95,-55.343982094743));
#43310=CARTESIAN_POINT('',(-16.8214173138198,4.95,-54.0471520880726));
#43311=CARTESIAN_POINT('',(-13.3342143560438,4.55,-55.600797903511));
#43312=CARTESIAN_POINT('',(-12.8301849517758,4.95,-55.343982094743));
#43313=CARTESIAN_POINT('',(-16.9450241115698,4.55,-54.4275746945907));
#43314=CARTESIAN_POINT('Origin',(-5.02920507986149,4.75,-30.6878211736169));
#43315=CARTESIAN_POINT('',(-4.83899377660246,4.95,-30.7496245724919));
#43316=CARTESIAN_POINT('',(-5.21941638312053,4.55,-30.6260177747419));
#43317=CARTESIAN_POINT('Origin',(-21.8937230027002,4.95,-52.8196449541365));
#43318=CARTESIAN_POINT('',(-21.8937230027002,0.75,-52.8196449541365));
#43319=CARTESIAN_POINT('',(-21.8937230027002,4.95,-52.8196449541365));
#43320=CARTESIAN_POINT('',(-21.8937230027002,0.75,-52.8196449541365));
#43321=CARTESIAN_POINT('Origin',(-13.3342143560438,4.95,-55.600797903511));
#43322=CARTESIAN_POINT('',(-13.3342143560438,0.75,-55.600797903511));
#43323=CARTESIAN_POINT('',(-13.3342143560438,4.95,-55.600797903511));
#43324=CARTESIAN_POINT('',(-13.3342143560438,0.75,-55.600797903511));
#43325=CARTESIAN_POINT('Origin',(-17.6604522772931,4.95,-68.9155891316432));
#43326=CARTESIAN_POINT('',(-17.6604522772931,0.75,-68.9155891316432));
#43327=CARTESIAN_POINT('Origin',(-7.13301510508756,4.75,-22.9022758698015));
#43328=CARTESIAN_POINT('',(-10.4334709354135,4.55,-56.2173699512871));
#43329=CARTESIAN_POINT('',(-6.93411072601391,4.55,-22.923181562455));
#43330=CARTESIAN_POINT('',(-10.7894683082537,4.95,-55.7777498078328));
#43331=CARTESIAN_POINT('',(-7.33191948416122,4.95,-22.881370177148));
#43332=CARTESIAN_POINT('',(-10.7894683082537,4.95,-55.7777498078328));
#43333=CARTESIAN_POINT('Origin',(-4.21984145529554,4.75,-56.6693470701065));
#43334=CARTESIAN_POINT('',(-1.04315373364464,4.95,-56.8021287478558));
#43335=CARTESIAN_POINT('',(-4.19893576264201,4.95,-56.4704426910328));
#43336=CARTESIAN_POINT('',(-1.48277387709901,4.55,-57.158126120696));
#43337=CARTESIAN_POINT('',(-1.04315373364464,4.95,-56.8021287478558));
#43338=CARTESIAN_POINT('',(-4.24074714794907,4.55,-56.8682514491801));
#43339=CARTESIAN_POINT('Origin',(1.48379146850063,4.75,-30.8464966920953));
#43340=CARTESIAN_POINT('',(1.68269584757429,4.95,-30.8674023847489));
#43341=CARTESIAN_POINT('',(1.28488708942698,4.55,-30.8255909994418));
#43342=CARTESIAN_POINT('Origin',(-10.4334709354135,4.95,-56.2173699512871));
#43343=CARTESIAN_POINT('',(-10.4334709354135,0.75,-56.2173699512871));
#43344=CARTESIAN_POINT('',(-10.4334709354135,4.95,-56.2173699512871));
#43345=CARTESIAN_POINT('',(-10.4334709354135,0.75,-56.2173699512871));
#43346=CARTESIAN_POINT('Origin',(-1.48277387709901,4.95,-57.158126120696));
#43347=CARTESIAN_POINT('',(-1.48277387709901,0.75,-57.158126120696));
#43348=CARTESIAN_POINT('',(-1.48277387709901,4.95,-57.158126120696));
#43349=CARTESIAN_POINT('',(-1.48277387709901,0.75,-57.158126120696));
#43350=CARTESIAN_POINT('Origin',(-2.94617236284616,4.95,-71.0814326558519));
#43351=CARTESIAN_POINT('',(-2.94617236284616,0.75,-71.0814326558519));
#43352=CARTESIAN_POINT('Origin',(-2.2154907113742,4.75,-23.8848434245174));
#43353=CARTESIAN_POINT('',(1.48277387709903,4.55,-57.158126120696));
#43354=CARTESIAN_POINT('',(-2.01658633230054,4.55,-23.8639377318639));
#43355=CARTESIAN_POINT('',(1.04315373364466,4.95,-56.8021287478558));
#43356=CARTESIAN_POINT('',(-2.41439509044785,4.95,-23.9057491171709));
#43357=CARTESIAN_POINT('',(1.04315373364466,4.95,-56.8021287478558));
#43358=CARTESIAN_POINT('Origin',(8.69518998445279,4.75,-56.198968985402));
#43359=CARTESIAN_POINT('',(10.7894683082537,4.95,-55.7777498078327));
#43360=CARTESIAN_POINT('',(8.67428429179926,4.95,-56.0000646063284));
#43361=CARTESIAN_POINT('',(10.4334709354135,4.55,-56.2173699512871));
#43362=CARTESIAN_POINT('',(10.7894683082537,4.95,-55.7777498078327));
#43363=CARTESIAN_POINT('',(8.71609567710632,4.55,-56.3978733644757));
#43364=CARTESIAN_POINT('Origin',(7.86471434796115,4.75,-29.8639291373794));
#43365=CARTESIAN_POINT('',(8.0636187270348,4.95,-29.8430234447259));
#43366=CARTESIAN_POINT('',(7.66580996888749,4.55,-29.8848348300329));
#43367=CARTESIAN_POINT('Origin',(1.48277387709903,4.95,-57.158126120696));
#43368=CARTESIAN_POINT('',(1.48277387709903,0.75,-57.158126120696));
#43369=CARTESIAN_POINT('',(1.48277387709903,4.95,-57.158126120696));
#43370=CARTESIAN_POINT('',(1.48277387709903,0.75,-57.158126120696));
#43371=CARTESIAN_POINT('Origin',(10.4334709354135,4.95,-56.2173699512871));
#43372=CARTESIAN_POINT('',(10.4334709354135,0.75,-56.2173699512871));
#43373=CARTESIAN_POINT('',(10.4334709354135,4.95,-56.2173699512871));
#43374=CARTESIAN_POINT('',(10.4334709354135,0.75,-56.2173699512871));
#43375=CARTESIAN_POINT('Origin',(11.8968694211606,4.95,-70.140676486443));
#43376=CARTESIAN_POINT('',(11.8968694211606,0.75,-70.140676486443));
#43377=CARTESIAN_POINT('Origin',(2.86608611923687,4.75,-24.0304255595508));
#43378=CARTESIAN_POINT('',(13.3342143560438,4.55,-55.600797903511));
#43379=CARTESIAN_POINT('',(3.0562974224959,4.55,-23.9686221606758));
#43380=CARTESIAN_POINT('',(12.8301849517758,4.95,-55.343982094743));
#43381=CARTESIAN_POINT('',(2.67587481597784,4.95,-24.0922289584258));
#43382=CARTESIAN_POINT('',(12.8301849517758,4.95,-55.343982094743));
#43383=CARTESIAN_POINT('Origin',(21.162975036023,4.75,-52.8467869166444));
#43384=CARTESIAN_POINT('',(22.1505388114683,4.95,-52.3156155498685));
#43385=CARTESIAN_POINT('',(21.101171637148,4.95,-52.6565756133854));
#43386=CARTESIAN_POINT('',(21.8937230027002,4.55,-52.8196449541365));
#43387=CARTESIAN_POINT('',(24.714060081258,8.94277798681721,-47.2844217746935));
#43388=CARTESIAN_POINT('',(21.224778434898,4.55,-53.0369982199034));
#43389=CARTESIAN_POINT('Origin',(13.3342143560438,4.95,-55.600797903511));
#43390=CARTESIAN_POINT('',(13.3342143560438,0.75,-55.600797903511));
#43391=CARTESIAN_POINT('',(13.3342143560438,4.95,-55.600797903511));
#43392=CARTESIAN_POINT('',(13.3342143560438,0.75,-55.600797903511));
#43393=CARTESIAN_POINT('Origin',(21.8937230027002,4.95,-52.8196449541365));
#43394=CARTESIAN_POINT('',(21.8937230027002,0.75,-52.8196449541365));
#43395=CARTESIAN_POINT('',(21.8937230027002,4.95,-52.8196449541365));
#43396=CARTESIAN_POINT('',(21.8937230027002,0.75,-52.8196449541365));
#43397=CARTESIAN_POINT('Origin',(13.9691363330359,4.75,-27.7830614264924));
#43398=CARTESIAN_POINT('',(13.7789250297769,4.55,-27.8448648253674));
#43399=CARTESIAN_POINT('',(14.159347636295,4.95,-27.7212580276174));
#43400=CARTESIAN_POINT('Origin',(0.,4.95,10.01));
#43401=CARTESIAN_POINT('',(-32.5435244785437,4.95,-46.5670378541992));
#43402=CARTESIAN_POINT('',(-28.5186714144556,4.95,-48.8907878541992));
#43403=CARTESIAN_POINT('',(-16.3262959055732,4.95,-18.4779740078565));
#43404=CARTESIAN_POINT('',(-34.2313826750721,4.95,-45.3407370931789));
#43405=CARTESIAN_POINT('',(-17.6239358377411,4.95,-26.8962987962786));
#43406=CARTESIAN_POINT('',(-41.5142019647506,4.95,-38.7832571508621));
#43407=CARTESIAN_POINT('',(-38.6895075057463,4.95,-41.3266234656553));
#43408=CARTESIAN_POINT('',(-20.2228408829076,4.95,-15.13680507562));
#43409=CARTESIAN_POINT('',(-42.9102141453889,4.95,-37.2328285521912));
#43410=CARTESIAN_POINT('',(-23.4599366320489,4.95,-23.1013747572434));
#43411=CARTESIAN_POINT('',(-48.6705096178551,4.95,-29.3044620073167));
#43412=CARTESIAN_POINT('',(-46.8478639959926,4.95,-31.8131184886743));
#43413=CARTESIAN_POINT('',(-23.5571131438905,4.95,-11.0585114463215));
#43414=CARTESIAN_POINT('',(-49.7136633514998,4.95,-27.497666740539));
#43415=CARTESIAN_POINT('',(-28.5781342694837,4.95,-18.0875229140527));
#43416=CARTESIAN_POINT('',(-53.6996824536426,4.95,-18.5449212556416));
#43417=CARTESIAN_POINT('',(-52.6512353814078,4.95,-20.8997719353731));
#43418=CARTESIAN_POINT('',(-26.1693351681284,4.95,-6.28762092762461));
#43419=CARTESIAN_POINT('',(-54.3443869165264,4.95,-16.5607249438808));
#43420=CARTESIAN_POINT('',(-32.6876140917459,4.95,-11.9574357753767));
#43421=CARTESIAN_POINT('',(-56.3819214865404,4.95,-6.97487845668955));
#43422=CARTESIAN_POINT('',(-55.9132113464906,4.95,-9.17998629418566));
#43423=CARTESIAN_POINT('',(-27.8781154566233,4.95,-0.916207452461114));
#43424=CARTESIAN_POINT('',(-56.6,4.95,-4.90000000000001));
#43425=CARTESIAN_POINT('',(-35.5,4.95,-4.9));
#43426=CARTESIAN_POINT('',(-56.6,4.95,4.89999999999999));
#43427=CARTESIAN_POINT('',(-56.6,4.95,2.75499999999999));
#43428=CARTESIAN_POINT('',(-28.5,4.95,4.9));
#43429=CARTESIAN_POINT('',(-56.3819214865404,4.95,6.97487845668952));
#43430=CARTESIAN_POINT('',(-36.7608655603543,4.95,2.80429427268419));
#43431=CARTESIAN_POINT('',(-54.3443869165264,4.95,16.5607249438808));
#43432=CARTESIAN_POINT('',(-54.8130970565762,4.95,14.3556171063847));
#43433=CARTESIAN_POINT('',(-27.8762977852036,4.95,10.9347589241512));
#43434=CARTESIAN_POINT('',(-53.6996824536427,4.95,18.5449212556415));
#43435=CARTESIAN_POINT('',(-36.2835932231409,4.95,10.7907787443291));
#43436=CARTESIAN_POINT('',(-49.7136633514998,4.95,27.497666740539));
#43437=CARTESIAN_POINT('',(-50.7621104237346,4.95,25.1428160608075));
#43438=CARTESIAN_POINT('',(-25.9027559174999,4.95,16.896367727696));
#43439=CARTESIAN_POINT('',(-48.6705096178552,4.95,29.3044620073167));
#43440=CARTESIAN_POINT('',(-33.9802699685724,4.95,18.6313781555222));
#43441=CARTESIAN_POINT('',(-42.9102141453889,4.95,37.2328285521912));
#43442=CARTESIAN_POINT('',(-44.7328597672515,4.95,34.7241720708337));
#43443=CARTESIAN_POINT('',(-22.5568555354815,4.95,22.4452479343494));
#43444=CARTESIAN_POINT('',(-41.5142019647506,4.95,38.7832571508621));
#43445=CARTESIAN_POINT('',(-29.8843372137378,4.95,25.8669838126164));
#43446=CARTESIAN_POINT('',(-34.2313826750722,4.95,45.3407370931789));
#43447=CARTESIAN_POINT('',(-37.0560771340764,4.95,42.7973707783858));
#43448=CARTESIAN_POINT('',(-17.9176036795473,4.95,27.2224499765914));
#43449=CARTESIAN_POINT('',(-32.5435244785438,4.95,46.5670378541992));
#43450=CARTESIAN_POINT('',(-24.1607530515143,4.95,32.0476518343475));
#43451=CARTESIAN_POINT('',(-24.0564755214563,4.95,51.4670378541992));
#43452=CARTESIAN_POINT('',(-28.0813285855444,4.95,49.1432878541992));
#43453=CARTESIAN_POINT('',(-12.1737040944268,4.95,30.8854740078565));
#43454=CARTESIAN_POINT('',(-22.1505388114683,4.95,52.3156155498684));
#43455=CARTESIAN_POINT('',(-17.1012128240188,4.95,36.775388084464));
#43456=CARTESIAN_POINT('',(-12.8301849517758,4.95,55.3439820947429));
#43457=CARTESIAN_POINT('',(-18.1593064494242,4.95,53.6124455565388));
#43458=CARTESIAN_POINT('',(-5.61774000370167,4.95,33.1463590152724));
#43459=CARTESIAN_POINT('',(-10.7894683082538,4.95,55.7777498078328));
#43460=CARTESIAN_POINT('',(-9.10421673957771,4.95,39.7436521863985));
#43461=CARTESIAN_POINT('',(-1.04315373364469,4.95,56.8021287478558));
#43462=CARTESIAN_POINT('',(-7.6336862792564,4.95,56.1094358646557));
#43463=CARTESIAN_POINT('',(1.37379707790495,4.95,33.8063778588436));
#43464=CARTESIAN_POINT('',(1.04315373364462,4.95,56.8021287478558));
#43465=CARTESIAN_POINT('',(-0.64209783503142,4.95,40.7680311264215));
#43466=CARTESIAN_POINT('',(10.7894683082537,4.95,55.7777498078328));
#43467=CARTESIAN_POINT('',(3.1583377500991,4.95,56.5798139493601));
#43468=CARTESIAN_POINT('',(8.37251749670409,4.95,32.7819989188206));
#43469=CARTESIAN_POINT('',(12.8301849517758,4.95,55.3439820947429));
#43470=CARTESIAN_POINT('',(7.78085896432628,4.95,39.8037546293385));
#43471=CARTESIAN_POINT('',(22.1505388114683,4.95,52.3156155498684));
#43472=CARTESIAN_POINT('',(13.879552126096,4.95,55.003022031226));
#43473=CARTESIAN_POINT('',(14.9380938633942,4.95,30.1179924703979));
#43474=CARTESIAN_POINT('',(24.0564755214562,4.95,51.4670378541992));
#43475=CARTESIAN_POINT('',(15.6737040944268,4.95,36.9476518343476));
#43476=CARTESIAN_POINT('',(32.5435244785437,4.95,46.5670378541992));
#43477=CARTESIAN_POINT('',(24.1842142685144,4.95,51.3932878541992));
#43478=CARTESIAN_POINT('',(20.6607530515143,4.95,25.9854740078565));
#43479=CARTESIAN_POINT('',(34.2313826750721,4.95,45.340737093179));
#43480=CARTESIAN_POINT('',(22.6015179240593,4.95,32.4244637549332));
#43481=CARTESIAN_POINT('',(41.5142019647506,4.95,38.7832571508621));
#43482=CARTESIAN_POINT('',(33.7119254194281,4.95,45.8084585070007));
#43483=CARTESIAN_POINT('',(25.2004229692258,4.95,20.6649700342747));
#43484=CARTESIAN_POINT('',(42.9102141453889,4.95,37.2328285521913));
#43485=CARTESIAN_POINT('',(28.2199744961061,4.95,26.5597447003967));
#43486=CARTESIAN_POINT('',(48.6705096178552,4.95,29.3044620073168));
#43487=CARTESIAN_POINT('',(42.0878261319353,4.95,38.3647485455209));
#43488=CARTESIAN_POINT('',(28.3171510079477,4.95,14.5168813894749));
#43489=CARTESIAN_POINT('',(49.7136633514998,4.95,27.4976667405391));
#43490=CARTESIAN_POINT('',(32.2975741209981,4.95,19.7435242292266));
#43491=CARTESIAN_POINT('',(53.6996824536426,4.95,18.5449212556416));
#43492=CARTESIAN_POINT('',(48.9317955298934,4.95,29.2537706201992));
#43493=CARTESIAN_POINT('',(29.8887750196427,4.95,7.94362224279855));
#43494=CARTESIAN_POINT('',(54.3443869165264,4.95,16.5607249438809));
#43495=CARTESIAN_POINT('',(34.7233309903403,4.95,12.3901407598755));
#43496=CARTESIAN_POINT('',(56.3819214865404,4.95,6.97487845668956));
#43497=CARTESIAN_POINT('',(53.8774944478963,4.95,18.7572813096869));
#43498=CARTESIAN_POINT('',(29.9138323552177,4.95,1.3489124369599));
#43499=CARTESIAN_POINT('',(56.6,4.95,4.9));
#43500=CARTESIAN_POINT('',(35.5,4.95,4.9));
#43501=CARTESIAN_POINT('',(56.6,4.95,-4.9));
#43502=CARTESIAN_POINT('',(56.6,4.95,7.255));
#43503=CARTESIAN_POINT('',(28.5,4.95,-4.9));
#43504=CARTESIAN_POINT('',(56.3819214865404,4.95,-6.97487845668953));
#43505=CARTESIAN_POINT('',(34.7251486617599,4.95,-2.37158928818542));
#43506=CARTESIAN_POINT('',(54.3443869165264,4.95,-16.5607249438808));
#43507=CARTESIAN_POINT('',(56.8488139551706,4.95,-4.77832209088351));
#43508=CARTESIAN_POINT('',(25.8405808866093,4.95,-10.5020539396524));
#43509=CARTESIAN_POINT('',(53.6996824536426,4.95,-18.5449212556415));
#43510=CARTESIAN_POINT('',(32.5641533716266,4.95,-9.13477742915521));
#43511=CARTESIAN_POINT('',(49.7136633514998,4.95,-27.497666740539));
#43512=CARTESIAN_POINT('',(54.4815502752489,4.95,-16.7888173759814));
#43513=CARTESIAN_POINT('',(22.1833160659855,4.95,-15.2403664125221));
#43514=CARTESIAN_POINT('',(48.6705096178552,4.95,-29.3044620073167));
#43515=CARTESIAN_POINT('',(29.2202321045151,4.95,-15.1730082123688));
#43516=CARTESIAN_POINT('',(42.9102141453889,4.95,-37.2328285521912));
#43517=CARTESIAN_POINT('',(49.4928976313087,4.95,-28.172542013987));
#43518=CARTESIAN_POINT('',(17.7968176714243,4.95,-18.986877991196));
#43519=CARTESIAN_POINT('',(41.5142019647506,4.95,-38.7832571508621));
#43520=CARTESIAN_POINT('',(24.9067551274196,4.95,-20.3388188539618));
#43521=CARTESIAN_POINT('',(34.2313826750722,4.95,-45.3407370931789));
#43522=CARTESIAN_POINT('',(42.0336592203946,4.95,-38.3155357370404));
#43523=CARTESIAN_POINT('',(12.9400215932291,4.95,-21.6942850179368));
#43524=CARTESIAN_POINT('',(32.5435244785438,4.95,-46.5670378541992));
#43525=CARTESIAN_POINT('',(19.8262959055732,4.95,-24.5401518343476));
#43526=CARTESIAN_POINT('',(24.0564755214563,4.95,-51.4670378541992));
#43527=CARTESIAN_POINT('',(32.4157857314856,4.95,-46.6407878541992));
#43528=CARTESIAN_POINT('',(7.8392469484857,4.95,-23.3779740078565));
#43529=CARTESIAN_POINT('',(-9.56543778402222,4.95,-2.95));
#43530=CARTESIAN_POINT('',(-12.4,4.95,-2.95));
#43531=CARTESIAN_POINT('',(6.,4.95,-2.95));
#43532=CARTESIAN_POINT('',(9.56543778402222,4.95,-2.95));
#43533=CARTESIAN_POINT('Origin',(0.,4.95,0.));
#43534=CARTESIAN_POINT('',(12.4,4.95,-2.95));
#43535=CARTESIAN_POINT('',(6.,4.95,-2.95));
#43536=CARTESIAN_POINT('',(12.4,4.95,2.95));
#43537=CARTESIAN_POINT('',(12.4,4.95,6.28));
#43538=CARTESIAN_POINT('',(9.56543778402222,4.95,2.95));
#43539=CARTESIAN_POINT('',(-6.,4.95,2.95));
#43540=CARTESIAN_POINT('',(-9.56543778402222,4.95,2.95));
#43541=CARTESIAN_POINT('Origin',(0.,4.95,0.));
#43542=CARTESIAN_POINT('',(-12.4,4.95,2.95));
#43543=CARTESIAN_POINT('',(-6.,4.95,2.95));
#43544=CARTESIAN_POINT('',(-12.4,4.95,3.73));
#43545=CARTESIAN_POINT('Origin',(8.01245202924258,4.75,-23.2779740078565));
#43546=CARTESIAN_POINT('',(24.60288568297,4.55,-51.613448015713));
#43547=CARTESIAN_POINT('',(8.18565710999947,4.55,-23.1779740078565));
#43548=CARTESIAN_POINT('',(24.0564755214563,4.95,-51.4670378541992));
#43549=CARTESIAN_POINT('Origin',(32.5157857314856,4.75,-46.8139929349561));
#43550=CARTESIAN_POINT('',(32.39711431703,4.55,-47.113448015713));
#43551=CARTESIAN_POINT('',(32.5435244785438,4.95,-46.5670378541992));
#43552=CARTESIAN_POINT('',(32.6157857314856,4.55,-46.987198015713));
#43553=CARTESIAN_POINT('Origin',(19.6530908248163,4.75,-24.6401518343476));
#43554=CARTESIAN_POINT('',(19.4798857440594,4.55,-24.7401518343476));
#43555=CARTESIAN_POINT('Origin',(13.0886505583246,4.75,-21.5604588966651));
#43556=CARTESIAN_POINT('',(34.7962928478066,4.55,-45.3703427808263));
#43557=CARTESIAN_POINT('',(13.2372795234201,4.55,-21.4266327753933));
#43558=CARTESIAN_POINT('',(34.2313826750722,4.95,-45.3407370931789));
#43559=CARTESIAN_POINT('Origin',(42.1674853416664,4.75,-38.4641647021359));
#43560=CARTESIAN_POINT('',(41.4845962771032,4.55,-39.3481673235966));
#43561=CARTESIAN_POINT('',(41.5142019647506,4.95,-38.7832571508621));
#43562=CARTESIAN_POINT('',(42.3013114629382,4.55,-38.6127936672313));
#43563=CARTESIAN_POINT('Origin',(24.7581261623241,4.75,-20.4726449752336));
#43564=CARTESIAN_POINT('',(24.6094971972286,4.55,-20.6064710965053));
#43565=CARTESIAN_POINT('Origin',(17.9143747218828,4.75,-18.825074592321));
#43566=CARTESIAN_POINT('',(43.4689350440559,4.55,-37.1443358553582));
#43567=CARTESIAN_POINT('',(18.0319317723412,4.55,-18.6632711934461));
#43568=CARTESIAN_POINT('',(42.9102141453889,4.95,-37.2328285521912));
#43569=CARTESIAN_POINT('Origin',(49.6547010301837,4.75,-28.2900990644455));
#43570=CARTESIAN_POINT('',(48.7590023146881,4.55,-29.8631829059837));
#43571=CARTESIAN_POINT('',(48.6705096178552,4.95,-29.3044620073167));
#43572=CARTESIAN_POINT('',(49.8165044290587,4.55,-28.407656114904));
#43573=CARTESIAN_POINT('Origin',(29.1026750540566,4.75,-15.3348116112438));
#43574=CARTESIAN_POINT('',(28.9851180035981,4.55,-15.4966150101188));
#43575=CARTESIAN_POINT('Origin',(22.2646633946007,4.75,-15.0576573209936));
#43576=CARTESIAN_POINT('',(50.2417761917872,4.55,-27.2949432147123));
#43577=CARTESIAN_POINT('',(22.3460107232159,4.55,-14.8749482294651));
#43578=CARTESIAN_POINT('',(49.7136633514998,4.95,-27.497666740539));
#43579=CARTESIAN_POINT('Origin',(54.6642593667775,4.75,-16.8701647045966));
#43580=CARTESIAN_POINT('',(53.9024059794694,4.55,-19.0730340959289));
#43581=CARTESIAN_POINT('',(53.6996824536426,4.95,-18.5449212556415));
#43582=CARTESIAN_POINT('',(54.846968458306,4.55,-16.9515120332117));
#43583=CARTESIAN_POINT('Origin',(32.4828060430114,4.75,-9.31748652068373));
#43584=CARTESIAN_POINT('',(32.4014587143963,4.55,-9.50019561221225));
#43585=CARTESIAN_POINT('Origin',(25.8821632247728,4.75,-10.3064244195056));
#43586=CARTESIAN_POINT('',(54.818810633147,4.55,-16.2526305799144));
#43587=CARTESIAN_POINT('',(25.9237455629364,4.55,-10.1107948993589));
#43588=CARTESIAN_POINT('',(54.3443869165264,4.95,-16.5607249438808));
#43589=CARTESIAN_POINT('Origin',(57.0444434753173,4.75,-4.81990442904706));
#43590=CARTESIAN_POINT('',(56.6900158505068,4.55,-7.44930217331016));
#43591=CARTESIAN_POINT('',(56.3819214865404,4.95,-6.97487845668953));
#43592=CARTESIAN_POINT('',(57.2400729954641,4.55,-4.86148676721061));
#43593=CARTESIAN_POINT('Origin',(34.6835663235964,4.75,-2.56721880833218));
#43594=CARTESIAN_POINT('',(34.6419839854328,4.55,-2.76284832847894));
#43595=CARTESIAN_POINT('Origin',(28.5,4.75,-4.7));
#43596=CARTESIAN_POINT('',(57.,4.55,-4.5));
#43597=CARTESIAN_POINT('',(28.5,4.55,-4.5));
#43598=CARTESIAN_POINT('',(56.6,4.95,-4.9));
#43599=CARTESIAN_POINT('Origin',(56.8,4.75,7.255));
#43600=CARTESIAN_POINT('',(57.,4.55,4.5));
#43601=CARTESIAN_POINT('',(56.6,4.95,4.9));
#43602=CARTESIAN_POINT('',(57.,4.55,7.255));
#43603=CARTESIAN_POINT('Origin',(35.5,4.75,4.7));
#43604=CARTESIAN_POINT('',(35.5,4.55,4.5));
#43605=CARTESIAN_POINT('Origin',(-28.6186714144556,4.75,-49.0639929349561));
#43606=CARTESIAN_POINT('',(-32.39711431703,4.55,-47.113448015713));
#43607=CARTESIAN_POINT('',(-28.7186714144556,4.55,-49.237198015713));
#43608=CARTESIAN_POINT('',(-34.1898431262531,9.44782619099021,-40.4228930154996));
#43609=CARTESIAN_POINT('Origin',(-24.60288568297,4.95,-51.613448015713));
#43610=CARTESIAN_POINT('',(-32.39711431703,0.75,-47.113448015713));
#43611=CARTESIAN_POINT('',(-24.60288568297,0.75,-51.613448015713));
#43612=CARTESIAN_POINT('',(-32.39711431703,4.95,-47.113448015713));
#43613=CARTESIAN_POINT('Origin',(-16.1530908248163,4.75,-18.5779740078565));
#43614=CARTESIAN_POINT('',(-15.9798857440594,4.55,-18.6779740078565));
#43615=CARTESIAN_POINT('Origin',(-20.0742119178121,4.75,-15.2706311968918));
#43616=CARTESIAN_POINT('',(-41.4845962771032,4.55,-39.3481673235966));
#43617=CARTESIAN_POINT('',(-19.9255829527166,4.55,-15.4044573181636));
#43618=CARTESIAN_POINT('',(-41.5142019647506,4.95,-38.7832571508621));
#43619=CARTESIAN_POINT('Origin',(-38.8233336270181,4.75,-41.4752524307507));
#43620=CARTESIAN_POINT('',(-34.7962928478066,4.55,-45.3703427808263));
#43621=CARTESIAN_POINT('',(-38.9571597482899,4.55,-41.6238813958462));
#43622=CARTESIAN_POINT('',(-34.2313826750721,4.95,-45.3407370931789));
#43623=CARTESIAN_POINT('Origin',(-17.7725648028366,4.75,-26.7624726750068));
#43624=CARTESIAN_POINT('',(-17.9211937679321,4.55,-26.6286465537351));
#43625=CARTESIAN_POINT('Origin',(-41.4845962771032,4.95,-39.3481673235966));
#43626=CARTESIAN_POINT('',(-41.4845962771032,0.75,-39.3481673235966));
#43627=CARTESIAN_POINT('',(-41.4845962771032,4.95,-39.3481673235966));
#43628=CARTESIAN_POINT('',(-41.4845962771032,0.75,-39.3481673235966));
#43629=CARTESIAN_POINT('Origin',(-34.7962928478066,4.95,-45.3703427808263));
#43630=CARTESIAN_POINT('',(-34.7962928478066,0.75,-45.3703427808263));
#43631=CARTESIAN_POINT('',(-34.7962928478066,4.95,-45.3703427808263));
#43632=CARTESIAN_POINT('',(-34.7962928478066,0.75,-45.3703427808263));
#43633=CARTESIAN_POINT('Origin',(-44.1641213368306,4.95,-55.7743703375099));
#43634=CARTESIAN_POINT('',(-44.1641213368306,0.75,-55.7743703375099));
#43635=CARTESIAN_POINT('Origin',(-23.439556093432,4.75,-11.2203148451965));
#43636=CARTESIAN_POINT('',(-48.7590023146881,4.55,-29.8631829059837));
#43637=CARTESIAN_POINT('',(-23.3219990429735,4.55,-11.3821182440715));
#43638=CARTESIAN_POINT('',(-48.6705096178551,4.95,-29.3044620073167));
#43639=CARTESIAN_POINT('Origin',(-47.0096673948676,4.75,-31.9306755391328));
#43640=CARTESIAN_POINT('',(-43.4689350440559,4.55,-37.1443358553582));
#43641=CARTESIAN_POINT('',(-47.1714707937426,4.55,-32.0482325895913));
#43642=CARTESIAN_POINT('',(-42.9102141453889,4.95,-37.2328285521912));
#43643=CARTESIAN_POINT('Origin',(-23.5774936825074,4.75,-22.9395713583684));
#43644=CARTESIAN_POINT('',(-23.6950507329659,4.55,-22.7777679594934));
#43645=CARTESIAN_POINT('Origin',(-48.7590023146881,4.95,-29.8631829059837));
#43646=CARTESIAN_POINT('',(-48.7590023146881,0.75,-29.8631829059837));
#43647=CARTESIAN_POINT('',(-48.7590023146881,4.95,-29.8631829059837));
#43648=CARTESIAN_POINT('',(-48.7590023146881,0.75,-29.8631829059837));
#43649=CARTESIAN_POINT('Origin',(-43.4689350440559,4.95,-37.1443358553582));
#43650=CARTESIAN_POINT('',(-43.4689350440559,0.75,-37.1443358553582));
#43651=CARTESIAN_POINT('',(-43.4689350440559,4.95,-37.1443358553582));
#43652=CARTESIAN_POINT('',(-43.4689350440559,0.75,-37.1443358553582));
#43653=CARTESIAN_POINT('Origin',(-54.7951729653051,4.95,-45.3733293874529));
#43654=CARTESIAN_POINT('',(-54.7951729653051,0.75,-45.3733293874529));
#43655=CARTESIAN_POINT('Origin',(-26.0879878395132,4.75,-6.47033001915313));
#43656=CARTESIAN_POINT('',(-53.9024059794693,4.55,-19.0730340959289));
#43657=CARTESIAN_POINT('',(-26.006640510898,4.55,-6.65303911068165));
#43658=CARTESIAN_POINT('',(-53.6996824536426,4.95,-18.5449212556416));
#43659=CARTESIAN_POINT('Origin',(-52.8339444729364,4.75,-20.9811192639883));
#43660=CARTESIAN_POINT('',(-50.2417761917871,4.55,-27.2949432147123));
#43661=CARTESIAN_POINT('',(-53.0166535644649,4.55,-21.0624665926034));
#43662=CARTESIAN_POINT('',(-49.7136633514998,4.95,-27.497666740539));
#43663=CARTESIAN_POINT('Origin',(-28.6594815980989,4.75,-17.9048138225242));
#43664=CARTESIAN_POINT('',(-28.740828926714,4.55,-17.7221047309957));
#43665=CARTESIAN_POINT('Origin',(-53.9024059794693,4.95,-19.0730340959289));
#43666=CARTESIAN_POINT('',(-53.9024059794693,0.75,-19.0730340959289));
#43667=CARTESIAN_POINT('',(-53.9024059794693,4.95,-19.0730340959289));
#43668=CARTESIAN_POINT('',(-53.9024059794693,0.75,-19.0730340959289));
#43669=CARTESIAN_POINT('Origin',(-50.2417761917871,4.95,-27.2949432147123));
#43670=CARTESIAN_POINT('',(-50.2417761917871,0.75,-27.2949432147123));
#43671=CARTESIAN_POINT('',(-50.2417761917871,4.95,-27.2949432147123));
#43672=CARTESIAN_POINT('',(-50.2417761917871,0.75,-27.2949432147123));
#43673=CARTESIAN_POINT('Origin',(-63.0314125987836,4.95,-32.9892562177735));
#43674=CARTESIAN_POINT('',(-63.0314125987836,0.75,-32.9892562177735));
#43675=CARTESIAN_POINT('Origin',(-27.8365331184597,4.75,-1.11183697260787));
#43676=CARTESIAN_POINT('',(-56.6900158505068,4.55,-7.44930217331018));
#43677=CARTESIAN_POINT('',(-27.7949507802962,4.55,-1.30746649275464));
#43678=CARTESIAN_POINT('',(-56.3819214865404,4.95,-6.97487845668955));
#43679=CARTESIAN_POINT('Origin',(-56.1088408666374,4.75,-9.22156863234921));
#43680=CARTESIAN_POINT('',(-54.818810633147,4.55,-16.2526305799144));
#43681=CARTESIAN_POINT('',(-56.3044703867841,4.55,-9.26315097051276));
#43682=CARTESIAN_POINT('',(-54.3443869165264,4.95,-16.5607249438808));
#43683=CARTESIAN_POINT('Origin',(-32.7291964299094,4.75,-11.76180625523));
#43684=CARTESIAN_POINT('',(-32.770778768073,4.55,-11.5661767350832));
#43685=CARTESIAN_POINT('Origin',(-56.6900158505068,4.95,-7.44930217331018));
#43686=CARTESIAN_POINT('',(-56.6900158505068,0.75,-7.44930217331018));
#43687=CARTESIAN_POINT('',(-56.6900158505068,4.95,-7.44930217331018));
#43688=CARTESIAN_POINT('',(-56.6900158505068,0.75,-7.44930217331018));
#43689=CARTESIAN_POINT('Origin',(-54.818810633147,4.95,-16.2526305799144));
#43690=CARTESIAN_POINT('',(-54.818810633147,0.75,-16.2526305799144));
#43691=CARTESIAN_POINT('',(-54.818810633147,4.95,-16.2526305799144));
#43692=CARTESIAN_POINT('',(-54.818810633147,0.75,-16.2526305799144));
#43693=CARTESIAN_POINT('Origin',(-68.5128770434203,4.95,-19.1633942513631));
#43694=CARTESIAN_POINT('',(-68.5128770434203,0.75,-19.1633942513631));
#43695=CARTESIAN_POINT('Origin',(-28.5,4.75,4.7));
#43696=CARTESIAN_POINT('',(-57.,4.55,4.49999999999999));
#43697=CARTESIAN_POINT('',(-28.5,4.55,4.5));
#43698=CARTESIAN_POINT('',(-56.6,4.95,4.89999999999999));
#43699=CARTESIAN_POINT('Origin',(-56.8,4.75,2.75499999999999));
#43700=CARTESIAN_POINT('',(-57.,4.55,-4.50000000000001));
#43701=CARTESIAN_POINT('',(-57.,4.55,2.75499999999999));
#43702=CARTESIAN_POINT('',(-56.6,4.95,-4.90000000000001));
#43703=CARTESIAN_POINT('Origin',(-35.5,4.75,-4.7));
#43704=CARTESIAN_POINT('',(-35.5,4.55,-4.5));
#43705=CARTESIAN_POINT('Origin',(-57.,4.95,4.49999999999999));
#43706=CARTESIAN_POINT('',(-57.,0.75,4.49999999999999));
#43707=CARTESIAN_POINT('',(-57.,4.95,4.49999999999999));
#43708=CARTESIAN_POINT('',(-57.,0.75,4.49999999999999));
#43709=CARTESIAN_POINT('Origin',(-57.,4.95,-4.50000000000001));
#43710=CARTESIAN_POINT('',(-57.,0.75,-4.50000000000001));
#43711=CARTESIAN_POINT('',(-57.,4.95,-4.50000000000001));
#43712=CARTESIAN_POINT('',(-57.,0.75,-4.50000000000001));
#43713=CARTESIAN_POINT('Origin',(-71.,4.95,-4.50000000000001));
#43714=CARTESIAN_POINT('',(-71.,0.75,-4.50000000000001));
#43715=CARTESIAN_POINT('Origin',(-27.9178801233672,4.75,10.7391294040044));
#43716=CARTESIAN_POINT('',(-54.818810633147,4.55,16.2526305799144));
#43717=CARTESIAN_POINT('',(-27.9594624615307,4.55,10.5434998838576));
#43718=CARTESIAN_POINT('',(-54.3443869165264,4.95,16.5607249438808));
#43719=CARTESIAN_POINT('Origin',(-55.0087265767229,4.75,14.3971994445483));
#43720=CARTESIAN_POINT('',(-56.6900158505068,4.55,7.44930217331014));
#43721=CARTESIAN_POINT('',(-55.2043560968697,4.55,14.4387817827118));
#43722=CARTESIAN_POINT('',(-56.3819214865404,4.95,6.97487845668952));
#43723=CARTESIAN_POINT('Origin',(-36.7192832221907,4.75,2.99992379283095));
#43724=CARTESIAN_POINT('',(-36.6777008840272,4.55,3.19555331297771));
#43725=CARTESIAN_POINT('Origin',(-54.818810633147,4.95,16.2526305799144));
#43726=CARTESIAN_POINT('',(-54.818810633147,0.75,16.2526305799144));
#43727=CARTESIAN_POINT('',(-54.818810633147,4.95,16.2526305799144));
#43728=CARTESIAN_POINT('',(-54.818810633147,0.75,16.2526305799144));
#43729=CARTESIAN_POINT('Origin',(-56.6900158505068,4.95,7.44930217331014));
#43730=CARTESIAN_POINT('',(-56.6900158505068,0.75,7.44930217331014));
#43731=CARTESIAN_POINT('',(-56.6900158505068,4.95,7.44930217331014));
#43732=CARTESIAN_POINT('',(-56.6900158505068,0.75,7.44930217331014));
#43733=CARTESIAN_POINT('Origin',(-70.3840822607801,4.95,10.3600658447588));
#43734=CARTESIAN_POINT('',(-70.3840822607801,0.75,10.3600658447588));
#43735=CARTESIAN_POINT('Origin',(-36.2022458945258,4.75,10.9734878358576));
#43736=CARTESIAN_POINT('',(-53.9024059794694,4.55,19.0730340959289));
#43737=CARTESIAN_POINT('',(-36.1208985659106,4.55,11.1561969273861));
#43738=CARTESIAN_POINT('',(-52.7669863049298,6.79033134765063,16.1151647179474));
#43739=CARTESIAN_POINT('Origin',(-66.6920423864658,4.95,24.7673470989901));
#43740=CARTESIAN_POINT('',(-53.9024059794694,0.75,19.0730340959289));
#43741=CARTESIAN_POINT('',(-66.6920423864658,0.75,24.7673470989901));
#43742=CARTESIAN_POINT('',(-53.9024059794694,4.95,19.0730340959289));
#43743=CARTESIAN_POINT('Origin',(-25.984103246115,4.75,16.7136586361675));
#43744=CARTESIAN_POINT('',(-50.2417761917872,4.55,27.2949432147123));
#43745=CARTESIAN_POINT('',(-26.0654505747302,4.55,16.530949544639));
#43746=CARTESIAN_POINT('',(-49.7136633514998,4.95,27.497666740539));
#43747=CARTESIAN_POINT('Origin',(-50.9448195152631,4.75,25.2241633894226));
#43748=CARTESIAN_POINT('',(-51.1275286067916,4.55,25.3055107180378));
#43749=CARTESIAN_POINT('Origin',(-50.2417761917872,4.95,27.2949432147123));
#43750=CARTESIAN_POINT('',(-50.2417761917872,0.75,27.2949432147123));
#43751=CARTESIAN_POINT('',(-50.2417761917872,4.95,27.2949432147123));
#43752=CARTESIAN_POINT('',(-50.2417761917872,0.75,27.2949432147123));
#43753=CARTESIAN_POINT('Origin',(-53.9024059794694,4.95,19.0730340959289));
#43754=CARTESIAN_POINT('',(-53.9024059794694,0.75,19.0730340959289));
#43755=CARTESIAN_POINT('Origin',(-22.67441258594,4.75,22.2834445354744));
#43756=CARTESIAN_POINT('',(-43.4689350440559,4.55,37.1443358553582));
#43757=CARTESIAN_POINT('',(-22.7919696363985,4.55,22.1216411365994));
#43758=CARTESIAN_POINT('',(-42.9102141453889,4.95,37.2328285521912));
#43759=CARTESIAN_POINT('Origin',(-44.8946631661265,4.75,34.8417291212921));
#43760=CARTESIAN_POINT('',(-48.7590023146881,4.55,29.8631829059837));
#43761=CARTESIAN_POINT('',(-45.0564665650015,4.55,34.9592861717506));
#43762=CARTESIAN_POINT('',(-48.6705096178552,4.95,29.3044620073167));
#43763=CARTESIAN_POINT('Origin',(-33.8627129181139,4.75,18.7931815543972));
#43764=CARTESIAN_POINT('',(-33.7451558676554,4.55,18.9549849532722));
#43765=CARTESIAN_POINT('Origin',(-43.4689350440559,4.95,37.1443358553582));
#43766=CARTESIAN_POINT('',(-43.4689350440559,0.75,37.1443358553582));
#43767=CARTESIAN_POINT('',(-43.4689350440559,4.95,37.1443358553582));
#43768=CARTESIAN_POINT('',(-43.4689350440559,0.75,37.1443358553582));
#43769=CARTESIAN_POINT('Origin',(-48.7590023146881,4.95,29.8631829059837));
#43770=CARTESIAN_POINT('',(-48.7590023146881,0.75,29.8631829059837));
#43771=CARTESIAN_POINT('',(-48.7590023146881,4.95,29.8631829059837));
#43772=CARTESIAN_POINT('',(-48.7590023146881,0.75,29.8631829059837));
#43773=CARTESIAN_POINT('Origin',(-60.0852402359374,4.95,38.0921764380783));
#43774=CARTESIAN_POINT('',(-60.0852402359374,0.75,38.0921764380783));
#43775=CARTESIAN_POINT('Origin',(-18.0662326446428,4.75,27.0886238553197));
#43776=CARTESIAN_POINT('',(-34.7962928478067,4.55,45.3703427808263));
#43777=CARTESIAN_POINT('',(-18.2148616097383,4.55,26.9547977340479));
#43778=CARTESIAN_POINT('',(-34.2313826750722,4.95,45.3407370931789));
#43779=CARTESIAN_POINT('Origin',(-37.1899032553482,4.75,42.9459997434813));
#43780=CARTESIAN_POINT('',(-41.4845962771032,4.55,39.3481673235966));
#43781=CARTESIAN_POINT('',(-37.32372937662,4.55,43.0946287085767));
#43782=CARTESIAN_POINT('',(-41.5142019647506,4.95,38.7832571508621));
#43783=CARTESIAN_POINT('Origin',(-29.7357082486423,4.75,26.0008099338882));
#43784=CARTESIAN_POINT('',(-29.5870792835468,4.55,26.1346360551599));
#43785=CARTESIAN_POINT('Origin',(-34.7962928478067,4.95,45.3703427808263));
#43786=CARTESIAN_POINT('',(-34.7962928478067,0.75,45.3703427808263));
#43787=CARTESIAN_POINT('',(-34.7962928478067,4.95,45.3703427808263));
#43788=CARTESIAN_POINT('',(-34.7962928478067,0.75,45.3703427808263));
#43789=CARTESIAN_POINT('Origin',(-41.4845962771032,4.95,39.3481673235966));
#43790=CARTESIAN_POINT('',(-41.4845962771032,0.75,39.3481673235966));
#43791=CARTESIAN_POINT('',(-41.4845962771032,4.95,39.3481673235966));
#43792=CARTESIAN_POINT('',(-41.4845962771032,0.75,39.3481673235966));
#43793=CARTESIAN_POINT('Origin',(-50.8524247661272,4.95,49.7521948802801));
#43794=CARTESIAN_POINT('',(-50.8524247661272,0.75,49.7521948802801));
#43795=CARTESIAN_POINT('Origin',(-12.3469091751837,4.75,30.7854740078565));
#43796=CARTESIAN_POINT('',(-24.6028856829701,4.55,51.613448015713));
#43797=CARTESIAN_POINT('',(-12.5201142559406,4.55,30.6854740078565));
#43798=CARTESIAN_POINT('',(-24.0564755214563,4.95,51.4670378541992));
#43799=CARTESIAN_POINT('Origin',(-28.1813285855445,4.75,49.3164929349561));
#43800=CARTESIAN_POINT('',(-32.39711431703,4.55,47.113448015713));
#43801=CARTESIAN_POINT('',(-28.2813285855445,4.55,49.489698015713));
#43802=CARTESIAN_POINT('',(-32.5435244785438,4.95,46.5670378541992));
#43803=CARTESIAN_POINT('Origin',(-23.9875479707574,4.75,32.1476518343475));
#43804=CARTESIAN_POINT('',(-23.8143428900005,4.55,32.2476518343475));
#43805=CARTESIAN_POINT('Origin',(-24.6028856829701,4.95,51.613448015713));
#43806=CARTESIAN_POINT('',(-24.6028856829701,0.75,51.613448015713));
#43807=CARTESIAN_POINT('',(-24.6028856829701,4.95,51.613448015713));
#43808=CARTESIAN_POINT('',(-24.6028856829701,0.75,51.613448015713));
#43809=CARTESIAN_POINT('Origin',(-32.39711431703,4.95,47.113448015713));
#43810=CARTESIAN_POINT('',(-32.39711431703,0.75,47.113448015713));
#43811=CARTESIAN_POINT('',(-32.39711431703,4.95,47.113448015713));
#43812=CARTESIAN_POINT('',(-32.39711431703,0.75,47.113448015713));
#43813=CARTESIAN_POINT('Origin',(-39.39711431703,4.95,59.2378036686951));
#43814=CARTESIAN_POINT('',(-39.39711431703,0.75,59.2378036686951));
#43815=CARTESIAN_POINT('Origin',(-5.8079513069607,4.75,33.0845556163974));
#43816=CARTESIAN_POINT('',(-13.3342143560438,4.55,55.600797903511));
#43817=CARTESIAN_POINT('',(-5.99816261021973,4.55,33.0227522175225));
#43818=CARTESIAN_POINT('',(-12.8301849517758,4.95,55.3439820947429));
#43819=CARTESIAN_POINT('Origin',(-18.2211098482992,4.75,53.8026568597978));
#43820=CARTESIAN_POINT('',(-21.8937230027002,4.55,52.8196449541365));
#43821=CARTESIAN_POINT('',(-18.2829132471742,4.55,53.9928681630568));
#43822=CARTESIAN_POINT('',(-22.1505388114683,4.95,52.3156155498684));
#43823=CARTESIAN_POINT('Origin',(-16.9110015207598,4.75,36.837191483339));
#43824=CARTESIAN_POINT('',(-16.7207902175007,4.55,36.898994882214));
#43825=CARTESIAN_POINT('Origin',(-13.3342143560438,4.95,55.600797903511));
#43826=CARTESIAN_POINT('',(-13.3342143560438,0.75,55.600797903511));
#43827=CARTESIAN_POINT('',(-13.3342143560438,4.95,55.600797903511));
#43828=CARTESIAN_POINT('',(-13.3342143560438,0.75,55.600797903511));
#43829=CARTESIAN_POINT('Origin',(-21.8937230027002,4.95,52.8196449541365));
#43830=CARTESIAN_POINT('',(-21.8937230027002,0.75,52.8196449541365));
#43831=CARTESIAN_POINT('',(-21.8937230027002,4.95,52.8196449541365));
#43832=CARTESIAN_POINT('',(-21.8937230027002,0.75,52.8196449541365));
#43833=CARTESIAN_POINT('Origin',(-26.2199609239495,4.95,66.1344361822686));
#43834=CARTESIAN_POINT('',(-26.2199609239495,0.75,66.1344361822686));
#43835=CARTESIAN_POINT('Origin',(1.17489269883129,4.75,33.7854721661901));
#43836=CARTESIAN_POINT('',(-1.48277387709906,4.55,57.158126120696));
#43837=CARTESIAN_POINT('',(0.975988319757637,4.55,33.7645664735366));
#43838=CARTESIAN_POINT('',(-1.04315373364469,4.95,56.8021287478558));
#43839=CARTESIAN_POINT('Origin',(-7.65459197190993,4.75,56.3083402437293));
#43840=CARTESIAN_POINT('',(-10.4334709354135,4.55,56.2173699512871));
#43841=CARTESIAN_POINT('',(-7.67549766456346,4.55,56.507244622803));
#43842=CARTESIAN_POINT('',(-10.7894683082538,4.95,55.7777498078328));
#43843=CARTESIAN_POINT('Origin',(-8.90531236050406,4.75,39.7645578790521));
#43844=CARTESIAN_POINT('',(-8.7064079814304,4.55,39.7854635717056));
#43845=CARTESIAN_POINT('Origin',(-1.48277387709906,4.95,57.158126120696));
#43846=CARTESIAN_POINT('',(-1.48277387709906,0.75,57.158126120696));
#43847=CARTESIAN_POINT('',(-1.48277387709906,4.95,57.158126120696));
#43848=CARTESIAN_POINT('',(-1.48277387709906,0.75,57.158126120696));
#43849=CARTESIAN_POINT('Origin',(-10.4334709354135,4.95,56.2173699512871));
#43850=CARTESIAN_POINT('',(-10.4334709354135,0.75,56.2173699512871));
#43851=CARTESIAN_POINT('',(-10.4334709354135,4.95,56.2173699512871));
#43852=CARTESIAN_POINT('',(-10.4334709354135,0.75,56.2173699512871));
#43853=CARTESIAN_POINT('Origin',(-11.8968694211607,4.95,70.140676486443));
#43854=CARTESIAN_POINT('',(-11.8968694211607,0.75,70.140676486443));
#43855=CARTESIAN_POINT('Origin',(8.17361311763044,4.75,32.8029046114742));
#43856=CARTESIAN_POINT('',(10.4334709354135,4.55,56.2173699512871));
#43857=CARTESIAN_POINT('',(7.97470873855678,4.55,32.8238103041277));
#43858=CARTESIAN_POINT('',(10.7894683082537,4.95,55.7777498078328));
#43859=CARTESIAN_POINT('Origin',(3.17924344275264,4.75,56.7787183284338));
#43860=CARTESIAN_POINT('',(1.48277387709899,4.55,57.158126120696));
#43861=CARTESIAN_POINT('',(3.20014913540617,4.55,56.9776227075075));
#43862=CARTESIAN_POINT('',(1.04315373364462,4.95,56.8021287478558));
#43863=CARTESIAN_POINT('Origin',(-0.443193455957765,4.75,40.747125433768));
#43864=CARTESIAN_POINT('',(-0.24428907688411,4.55,40.7262197411145));
#43865=CARTESIAN_POINT('Origin',(10.4334709354135,4.95,56.2173699512871));
#43866=CARTESIAN_POINT('',(10.4334709354135,0.75,56.2173699512871));
#43867=CARTESIAN_POINT('',(10.4334709354135,4.95,56.2173699512871));
#43868=CARTESIAN_POINT('',(10.4334709354135,0.75,56.2173699512871));
#43869=CARTESIAN_POINT('Origin',(1.48277387709899,4.95,57.158126120696));
#43870=CARTESIAN_POINT('',(1.48277387709899,0.75,57.158126120696));
#43871=CARTESIAN_POINT('',(1.48277387709899,4.95,57.158126120696));
#43872=CARTESIAN_POINT('',(1.48277387709899,0.75,57.158126120696));
#43873=CARTESIAN_POINT('Origin',(2.94617236284613,4.95,71.0814326558519));
#43874=CARTESIAN_POINT('',(2.94617236284613,0.75,71.0814326558519));
#43875=CARTESIAN_POINT('Origin',(14.7478825601351,4.75,30.1797958692729));
#43876=CARTESIAN_POINT('',(21.8937230027002,4.55,52.8196449541365));
#43877=CARTESIAN_POINT('',(14.5576712568761,4.55,30.2415992681479));
#43878=CARTESIAN_POINT('',(22.1505388114683,4.95,52.3156155498684));
#43879=CARTESIAN_POINT('Origin',(13.941355524971,4.75,55.193233334485));
#43880=CARTESIAN_POINT('',(13.3342143560438,4.55,55.600797903511));
#43881=CARTESIAN_POINT('',(14.003158923846,4.55,55.3834446377441));
#43882=CARTESIAN_POINT('',(12.8301849517758,4.95,55.3439820947429));
#43883=CARTESIAN_POINT('Origin',(7.97107026758531,4.75,39.7419512304635));
#43884=CARTESIAN_POINT('',(8.16128157084435,4.55,39.6801478315885));
#43885=CARTESIAN_POINT('Origin',(21.8937230027002,4.95,52.8196449541365));
#43886=CARTESIAN_POINT('',(21.8937230027002,0.75,52.8196449541365));
#43887=CARTESIAN_POINT('',(21.8937230027002,4.95,52.8196449541365));
#43888=CARTESIAN_POINT('',(21.8937230027002,0.75,52.8196449541365));
#43889=CARTESIAN_POINT('Origin',(13.3342143560438,4.95,55.600797903511));
#43890=CARTESIAN_POINT('',(13.3342143560438,0.75,55.600797903511));
#43891=CARTESIAN_POINT('',(13.3342143560438,4.95,55.600797903511));
#43892=CARTESIAN_POINT('',(13.3342143560438,0.75,55.600797903511));
#43893=CARTESIAN_POINT('Origin',(17.6604522772931,4.95,68.9155891316432));
#43894=CARTESIAN_POINT('',(17.6604522772931,0.75,68.9155891316432));
#43895=CARTESIAN_POINT('Origin',(20.4875479707574,4.75,26.0854740078565));
#43896=CARTESIAN_POINT('',(32.3971143170299,4.55,47.113448015713));
#43897=CARTESIAN_POINT('',(20.3143428900005,4.55,26.1854740078565));
#43898=CARTESIAN_POINT('',(32.5435244785437,4.95,46.5670378541992));
#43899=CARTESIAN_POINT('Origin',(24.2842142685144,4.75,51.5664929349561));
#43900=CARTESIAN_POINT('',(24.60288568297,4.55,51.613448015713));
#43901=CARTESIAN_POINT('',(24.3842142685144,4.55,51.739698015713));
#43902=CARTESIAN_POINT('',(24.0564755214562,4.95,51.4670378541992));
#43903=CARTESIAN_POINT('Origin',(15.8469091751837,4.75,36.8476518343476));
#43904=CARTESIAN_POINT('',(16.0201142559406,4.55,36.7476518343476));
#43905=CARTESIAN_POINT('Origin',(32.3971143170299,4.95,47.113448015713));
#43906=CARTESIAN_POINT('',(32.3971143170299,0.75,47.113448015713));
#43907=CARTESIAN_POINT('',(32.3971143170299,4.95,47.113448015713));
#43908=CARTESIAN_POINT('',(32.3971143170299,0.75,47.113448015713));
#43909=CARTESIAN_POINT('Origin',(24.60288568297,4.95,51.613448015713));
#43910=CARTESIAN_POINT('',(24.60288568297,0.75,51.613448015713));
#43911=CARTESIAN_POINT('',(24.60288568297,4.95,51.613448015713));
#43912=CARTESIAN_POINT('',(24.60288568297,0.75,51.613448015713));
#43913=CARTESIAN_POINT('Origin',(31.60288568297,4.95,63.7378036686952));
#43914=CARTESIAN_POINT('',(31.60288568297,0.75,63.7378036686952));
#43915=CARTESIAN_POINT('Origin',(25.0517940041303,4.75,20.7987961555464));
#43916=CARTESIAN_POINT('',(41.4845962771032,4.55,39.3481673235966));
#43917=CARTESIAN_POINT('',(24.9031650390348,4.55,20.9326222768182));
#43918=CARTESIAN_POINT('',(41.5142019647506,4.95,38.7832571508621));
#43919=CARTESIAN_POINT('Origin',(33.8457515406999,4.75,45.9570874720961));
#43920=CARTESIAN_POINT('',(34.7962928478066,4.55,45.3703427808264));
#43921=CARTESIAN_POINT('',(33.9795776619717,4.55,46.1057164371916));
#43922=CARTESIAN_POINT('',(34.2313826750721,4.95,45.340737093179));
#43923=CARTESIAN_POINT('Origin',(22.7501468891548,4.75,32.2906376336614));
#43924=CARTESIAN_POINT('',(22.8987758542503,4.55,32.1568115123897));
#43925=CARTESIAN_POINT('Origin',(41.4845962771032,4.95,39.3481673235966));
#43926=CARTESIAN_POINT('',(41.4845962771032,0.75,39.3481673235966));
#43927=CARTESIAN_POINT('',(41.4845962771032,4.95,39.3481673235966));
#43928=CARTESIAN_POINT('',(41.4845962771032,0.75,39.3481673235966));
#43929=CARTESIAN_POINT('Origin',(34.7962928478066,4.95,45.3703427808264));
#43930=CARTESIAN_POINT('',(34.7962928478066,0.75,45.3703427808264));
#43931=CARTESIAN_POINT('',(34.7962928478066,4.95,45.3703427808264));
#43932=CARTESIAN_POINT('',(34.7962928478066,0.75,45.3703427808264));
#43933=CARTESIAN_POINT('Origin',(44.1641213368306,4.95,55.7743703375099));
#43934=CARTESIAN_POINT('',(44.1641213368306,0.75,55.7743703375099));
#43935=CARTESIAN_POINT('Origin',(28.1995939574892,4.75,14.6786847883499));
#43936=CARTESIAN_POINT('',(48.7590023146881,4.55,29.8631829059837));
#43937=CARTESIAN_POINT('',(28.0820369070308,4.55,14.8404881872249));
#43938=CARTESIAN_POINT('',(48.6705096178552,4.95,29.3044620073168));
#43939=CARTESIAN_POINT('Origin',(42.2496295308103,4.75,38.4823055959794));
#43940=CARTESIAN_POINT('',(43.4689350440559,4.55,37.1443358553582));
#43941=CARTESIAN_POINT('',(42.4114329296853,4.55,38.5998626464379));
#43942=CARTESIAN_POINT('',(42.9102141453889,4.95,37.2328285521912));
#43943=CARTESIAN_POINT('Origin',(28.3375315465646,4.75,26.3979413015218));
#43944=CARTESIAN_POINT('',(28.4550885970231,4.55,26.2361379026468));
#43945=CARTESIAN_POINT('Origin',(48.7590023146881,4.95,29.8631829059837));
#43946=CARTESIAN_POINT('',(48.7590023146881,0.75,29.8631829059837));
#43947=CARTESIAN_POINT('',(48.7590023146881,4.95,29.8631829059837));
#43948=CARTESIAN_POINT('',(48.7590023146881,0.75,29.8631829059837));
#43949=CARTESIAN_POINT('Origin',(43.4689350440559,4.95,37.1443358553582));
#43950=CARTESIAN_POINT('',(43.4689350440559,0.75,37.1443358553582));
#43951=CARTESIAN_POINT('',(43.4689350440559,4.95,37.1443358553582));
#43952=CARTESIAN_POINT('',(43.4689350440559,0.75,37.1443358553582));
#43953=CARTESIAN_POINT('Origin',(54.7951729653051,4.95,45.3733293874529));
#43954=CARTESIAN_POINT('',(54.7951729653051,0.75,45.3733293874529));
#43955=CARTESIAN_POINT('Origin',(29.8074276910276,4.75,8.12633133432707));
#43956=CARTESIAN_POINT('',(53.9024059794693,4.55,19.0730340959289));
#43957=CARTESIAN_POINT('',(29.7260803624124,4.55,8.30904042585558));
#43958=CARTESIAN_POINT('',(53.6996824536426,4.95,18.5449212556416));
#43959=CARTESIAN_POINT('Origin',(49.114504621422,4.75,29.3351179488144));
#43960=CARTESIAN_POINT('',(50.2417761917871,4.55,27.2949432147124));
#43961=CARTESIAN_POINT('',(49.2972137129505,4.55,29.4164652774295));
#43962=CARTESIAN_POINT('',(49.7136633514998,4.95,27.4976667405391));
#43963=CARTESIAN_POINT('Origin',(32.3789214496132,4.75,19.5608151376981));
#43964=CARTESIAN_POINT('',(32.4602687782284,4.55,19.3781060461696));
#43965=CARTESIAN_POINT('Origin',(53.9024059794693,4.95,19.0730340959289));
#43966=CARTESIAN_POINT('',(53.9024059794693,0.75,19.0730340959289));
#43967=CARTESIAN_POINT('',(53.9024059794693,4.95,19.0730340959289));
#43968=CARTESIAN_POINT('',(53.9024059794693,0.75,19.0730340959289));
#43969=CARTESIAN_POINT('Origin',(50.2417761917871,4.95,27.2949432147124));
#43970=CARTESIAN_POINT('',(50.2417761917871,0.75,27.2949432147124));
#43971=CARTESIAN_POINT('',(50.2417761917871,4.95,27.2949432147124));
#43972=CARTESIAN_POINT('',(50.2417761917871,0.75,27.2949432147124));
#43973=CARTESIAN_POINT('Origin',(63.0314125987835,4.95,32.9892562177736));
#43974=CARTESIAN_POINT('',(63.0314125987835,0.75,32.9892562177736));
#43975=CARTESIAN_POINT('Origin',(29.8722500170541,4.75,1.54454195710666));
#43976=CARTESIAN_POINT('',(56.6900158505068,4.55,7.44930217331019));
#43977=CARTESIAN_POINT('',(29.8306676788906,4.55,1.74017147725342));
#43978=CARTESIAN_POINT('',(56.3819214865404,4.95,6.97487845668956));
#43979=CARTESIAN_POINT('Origin',(54.073123968043,4.75,18.7988636478504));
#43980=CARTESIAN_POINT('',(54.818810633147,4.55,16.2526305799144));
#43981=CARTESIAN_POINT('',(54.2687534881898,4.55,18.840445986014));
#43982=CARTESIAN_POINT('',(54.3443869165264,4.95,16.5607249438809));
#43983=CARTESIAN_POINT('Origin',(34.7649133285038,4.75,12.1945112397288));
#43984=CARTESIAN_POINT('',(34.8064956666674,4.55,11.998881719582));
#43985=CARTESIAN_POINT('Origin',(56.6900158505068,4.95,7.44930217331019));
#43986=CARTESIAN_POINT('',(56.6900158505068,0.75,7.44930217331019));
#43987=CARTESIAN_POINT('',(56.6900158505068,4.95,7.44930217331019));
#43988=CARTESIAN_POINT('',(56.6900158505068,0.75,7.44930217331019));
#43989=CARTESIAN_POINT('Origin',(54.818810633147,4.95,16.2526305799144));
#43990=CARTESIAN_POINT('',(54.818810633147,0.75,16.2526305799144));
#43991=CARTESIAN_POINT('',(54.818810633147,4.95,16.2526305799144));
#43992=CARTESIAN_POINT('',(54.818810633147,0.75,16.2526305799144));
#43993=CARTESIAN_POINT('Origin',(68.5128770434203,4.95,19.1633942513631));
#43994=CARTESIAN_POINT('',(68.5128770434203,0.75,19.1633942513631));
#43995=CARTESIAN_POINT('Origin',(56.8,-4.75,32.75));
#43996=CARTESIAN_POINT('',(56.6,-4.95,4.9));
#43997=CARTESIAN_POINT('',(56.6,-4.95,-4.9));
#43998=CARTESIAN_POINT('',(56.6,-4.95,32.75));
#43999=CARTESIAN_POINT('',(57.,-4.55,-4.5));
#44000=CARTESIAN_POINT('',(59.4916666666667,-2.05833333333331,-2.0083333333333));
#44001=CARTESIAN_POINT('',(57.,-4.55,4.5));
#44002=CARTESIAN_POINT('',(57.,-4.55,32.75));
#44003=CARTESIAN_POINT('',(57.,-4.55,4.5));
#44004=CARTESIAN_POINT('Origin',(28.5,-4.75,4.7));
#44005=CARTESIAN_POINT('',(28.5,-4.55,4.5));
#44006=CARTESIAN_POINT('',(28.5,-4.95,4.9));
#44007=CARTESIAN_POINT('Origin',(0.,-4.95,70.));
#44008=CARTESIAN_POINT('',(35.5,-4.95,-4.9));
#44009=CARTESIAN_POINT('',(56.3819214865404,-4.95,6.97487845668957));
#44010=CARTESIAN_POINT('',(42.8608983648836,-4.95,4.10089627168932));
#44011=CARTESIAN_POINT('',(54.3443869165264,-4.95,16.5607249438808));
#44012=CARTESIAN_POINT('',(48.7130642520468,-4.95,43.0540151073797));
#44013=CARTESIAN_POINT('',(33.976330589733,-4.95,12.2313609231563));
#44014=CARTESIAN_POINT('',(53.6996824536426,-4.95,18.5449212556416));
#44015=CARTESIAN_POINT('',(47.4289077432382,-4.95,15.7529924754622));
#44016=CARTESIAN_POINT('',(49.7136633514998,-4.95,27.4976667405391));
#44017=CARTESIAN_POINT('',(39.6167959036373,-4.95,50.1756023296745));
#44018=CARTESIAN_POINT('',(37.0480704375971,-4.95,21.8585814588291));
#44019=CARTESIAN_POINT('',(48.6705096178552,-4.95,29.3044620073168));
#44020=CARTESIAN_POINT('',(48.2437400717089,-4.95,28.994395782384));
#44021=CARTESIAN_POINT('',(42.9102141453889,-4.95,37.2328285521913));
#44022=CARTESIAN_POINT('',(30.4693896641149,-4.95,54.3561544439719));
#44023=CARTESIAN_POINT('',(36.8203256386181,-4.95,32.8082655612112));
#44024=CARTESIAN_POINT('',(41.5142019647506,-4.95,38.7832571508621));
#44025=CARTESIAN_POINT('',(44.7996793395235,-4.95,42.4321494404731));
#44026=CARTESIAN_POINT('',(34.2313826750721,-4.95,45.3407370931789));
#44027=CARTESIAN_POINT('',(22.1407350082907,-4.95,56.2272051505292));
#44028=CARTESIAN_POINT('',(32.832945805333,-4.95,43.7876156044481));
#44029=CARTESIAN_POINT('',(32.5435244785437,-4.95,46.5670378541993));
#44030=CARTESIAN_POINT('',(37.1489690447714,-4.95,54.5439018343476));
#44031=CARTESIAN_POINT('',(24.0564755214562,-4.95,51.4670378541992));
#44032=CARTESIAN_POINT('',(15.0931125922873,-4.95,56.6420378541992));
#44033=CARTESIAN_POINT('',(25.1619200876839,-4.95,53.3817240078565));
#44034=CARTESIAN_POINT('',(22.1505388114683,-4.95,52.3156155498685));
#44035=CARTESIAN_POINT('',(25.9165221452752,-4.95,63.9061204576023));
#44036=CARTESIAN_POINT('',(12.8301849517758,-4.95,55.3439820947429));
#44037=CARTESIAN_POINT('',(9.34399712816784,-4.95,56.4767131834005));
#44038=CARTESIAN_POINT('',(14.433049324958,-4.95,60.2770913884107));
#44039=CARTESIAN_POINT('',(10.7894683082537,-4.95,55.7777498078328));
#44040=CARTESIAN_POINT('',(12.222372322617,-4.95,69.4109208284038));
#44041=CARTESIAN_POINT('',(1.04315373364462,-4.95,56.8021287478558));
#44042=CARTESIAN_POINT('',(4.515530696217,-4.95,56.4371672226504));
#44043=CARTESIAN_POINT('',(1.74435850513434,-4.95,63.4736465008489));
#44044=CARTESIAN_POINT('',(-1.04315373364469,-4.95,56.8021287478558));
#44045=CARTESIAN_POINT('',(-2.476057748008,-4.95,70.4352997684268));
#44046=CARTESIAN_POINT('',(-10.7894683082538,-4.95,55.7777498078328));
#44047=CARTESIAN_POINT('',(-0.040182167059801,-4.95,56.9075453073549));
#44048=CARTESIAN_POINT('',(-11.4906730797435,-4.95,62.4492675608259));
#44049=CARTESIAN_POINT('',(-12.8301849517758,-4.95,55.3439820947429));
#44050=CARTESIAN_POINT('',(-16.5961682855827,-4.95,66.9344870024768));
#44051=CARTESIAN_POINT('',(-22.1505388114683,-4.95,52.3156155498685));
#44052=CARTESIAN_POINT('',(-5.06424280483965,-4.95,57.8672896580878));
#44053=CARTESIAN_POINT('',(-23.7534031846505,-4.95,57.2487248435362));
#44054=CARTESIAN_POINT('',(-24.0564755214563,-4.95,51.4670378541992));
#44055=CARTESIAN_POINT('',(-28.6619200876839,-4.95,59.4439018343476));
#44056=CARTESIAN_POINT('',(-32.5435244785438,-4.95,46.5670378541992));
#44057=CARTESIAN_POINT('',(-11.1959982752574,-4.95,58.8920378541992));
#44058=CARTESIAN_POINT('',(-33.6489690447714,-4.95,48.4817240078565));
#44059=CARTESIAN_POINT('',(-34.2313826750722,-4.95,45.3407370931789));
#44060=CARTESIAN_POINT('',(-37.516860049845,-4.95,48.9896293827898));
#44061=CARTESIAN_POINT('',(-41.5142019647506,-4.95,38.7832571508621));
#44062=CARTESIAN_POINT('',(-18.7965832936425,-4.95,59.238292879144));
#44063=CARTESIAN_POINT('',(-40.1157650950115,-4.95,37.2301356621313));
#44064=CARTESIAN_POINT('',(-42.9102141453889,-4.95,37.2328285521912));
#44065=CARTESIAN_POINT('',(-42.4834445992427,-4.95,36.9227623272584));
#44066=CARTESIAN_POINT('',(-48.6705096178552,-4.95,29.3044620073167));
#44067=CARTESIAN_POINT('',(-27.8243560287988,-4.95,57.9967309186592));
#44068=CARTESIAN_POINT('',(-42.5806211110843,-4.95,24.8798990163367));
#44069=CARTESIAN_POINT('',(-49.7136633514998,-4.95,27.497666740539));
#44070=CARTESIAN_POINT('',(-43.4428886410953,-4.95,24.7057379603596));
#44071=CARTESIAN_POINT('',(-53.6996824536427,-4.95,18.5449212556415));
#44072=CARTESIAN_POINT('',(-37.7864810097963,-4.95,54.2865568890662));
#44073=CARTESIAN_POINT('',(-41.0340895397399,-4.95,12.9058359739315));
#44074=CARTESIAN_POINT('',(-54.3443869165264,-4.95,16.5607249438808));
#44075=CARTESIAN_POINT('',(-40.8233637948696,-4.95,13.6867427588806));
#44076=CARTESIAN_POINT('',(-56.3819214865404,-4.95,6.97487845668952));
#44077=CARTESIAN_POINT('',(-47.777461643367,-4.95,47.4556793106817));
#44078=CARTESIAN_POINT('',(-36.013865159747,-4.95,2.64551443596496));
#44079=CARTESIAN_POINT('',(-56.6,-4.95,4.9));
#44080=CARTESIAN_POINT('',(-35.5,-4.95,4.9));
#44081=CARTESIAN_POINT('',(-56.6,-4.95,-4.90000000000001));
#44082=CARTESIAN_POINT('',(-56.6,-4.95,37.25));
#44083=CARTESIAN_POINT('',(-28.5,-4.95,-4.90000000000001));
#44084=CARTESIAN_POINT('',(-56.3819214865404,-4.95,-6.97487845668956));
#44085=CARTESIAN_POINT('',(-28.6251158572306,-4.95,-1.07498728918034));
#44086=CARTESIAN_POINT('',(-54.3443869165264,-4.95,-16.5607249438809));
#44087=CARTESIAN_POINT('',(-62.9488467596999,-4.95,23.9200759101114));
#44088=CARTESIAN_POINT('',(-19.7405480820799,-4.95,-9.20545194064731));
#44089=CARTESIAN_POINT('',(-53.6996824536426,-4.95,-18.5449212556416));
#44090=CARTESIAN_POINT('',(-21.4188388515293,-4.95,-4.17256369802218));
#44091=CARTESIAN_POINT('',(-49.7136633514998,-4.95,-27.497666740539));
#44092=CARTESIAN_POINT('',(-65.6268647953462,-4.95,8.24396889288556));
#44093=CARTESIAN_POINT('',(-11.0380015458883,-4.95,-10.2781526813891));
#44094=CARTESIAN_POINT('',(-48.6705096178552,-4.95,-29.3044620073167));
#44095=CARTESIAN_POINT('',(-14.9567620013786,-4.95,-4.80999058550712));
#44096=CARTESIAN_POINT('',(-42.9102141453889,-4.95,-37.2328285521912));
#44097=CARTESIAN_POINT('',(-63.7563677344453,-4.95,-8.54055964084878));
#44098=CARTESIAN_POINT('',(-3.53334756828769,-4.95,-8.6238603643343));
#44099=CARTESIAN_POINT('',(-41.5142019647506,-4.95,-38.7832571508621));
#44100=CARTESIAN_POINT('',(-9.9914130016339,-4.95,-3.77365322610516));
#44101=CARTESIAN_POINT('',(-34.2313826750721,-4.95,-45.3407370931789));
#44102=CARTESIAN_POINT('',(-56.9490013461803,-4.95,-24.885701364897));
#44103=CARTESIAN_POINT('',(1.97532053255655,-4.95,-5.12911939008019));
#44104=CARTESIAN_POINT('',(-32.5435244785437,-4.95,-46.5670378541993));
#44105=CARTESIAN_POINT('',(-6.83807991231607,-4.95,-2.04390183434758));
#44106=CARTESIAN_POINT('',(-24.0564755214562,-4.95,-51.4670378541992));
#44107=CARTESIAN_POINT('',(-45.4040017247427,-4.95,-39.1420378541993));
#44108=CARTESIAN_POINT('',(5.14896904477143,-4.95,-0.881724007856505));
#44109=CARTESIAN_POINT('',(-22.1505388114683,-4.95,-52.3156155498685));
#44110=CARTESIAN_POINT('',(-5.34403831503861,-4.95,-0.590525654479128));
#44111=CARTESIAN_POINT('',(-12.8301849517758,-4.95,-55.3439820947429));
#44112=CARTESIAN_POINT('',(-29.9164809584044,-4.95,-49.7923079865237));
#44113=CARTESIAN_POINT('',(6.13943450527853,-4.95,3.03850341471246));
#44114=CARTESIAN_POINT('',(-10.7894683082537,-4.95,-55.7777498078328));
#44115=CARTESIAN_POINT('',(-4.94546314399545,-4.95,-0.175754802720606));
#44116=CARTESIAN_POINT('',(-1.04315373364464,-4.95,-56.8021287478558));
#44117=CARTESIAN_POINT('',(-11.7924398748386,-4.95,-55.6723332483337));
#44118=CARTESIAN_POINT('',(5.5325506734872,-4.95,5.76151952483431));
#44119=CARTESIAN_POINT('',(1.04315373364466,-4.95,-56.8021287478558));
#44120=CARTESIAN_POINT('',(-4.80085143061363,-4.95,-1.20013374274361));
#44121=CARTESIAN_POINT('',(10.7894683082537,-4.95,-55.7777498078327));
#44122=CARTESIAN_POINT('',(7.31709134568138,-4.95,-56.1427113330381));
#44123=CARTESIAN_POINT('',(4.21376390112187,-4.95,6.78589846485731));
#44124=CARTESIAN_POINT('',(12.8301849517758,-4.95,-55.343982094743));
#44125=CARTESIAN_POINT('',(-3.9763155446539,-4.95,-3.61889219935362));
#44126=CARTESIAN_POINT('',(22.1505388114683,-4.95,-52.3156155498685));
#44127=CARTESIAN_POINT('',(25.6367266350762,-4.95,-51.1828844612109));
#44128=CARTESIAN_POINT('',(3.18091935441398,-4.95,6.06686995958694));
#44129=CARTESIAN_POINT('',(24.0564755214563,-4.95,-51.4670378541992));
#44130=CARTESIAN_POINT('',(-1.64896904477142,-4.95,-6.94390183434757));
#44131=CARTESIAN_POINT('',(32.5435244785437,-4.95,-46.5670378541992));
#44132=CARTESIAN_POINT('',(41.5068874077127,-4.95,-41.3920378541992));
#44133=CARTESIAN_POINT('',(3.33807991231607,-4.95,4.01827599214349));
#44134=CARTESIAN_POINT('',(34.2313826750722,-4.95,-45.3407370931789));
#44135=CARTESIAN_POINT('',(2.70859371195544,-4.95,-10.331133168422));
#44136=CARTESIAN_POINT('',(41.5142019647506,-4.95,-38.7832571508621));
#44137=CARTESIAN_POINT('',(53.604849631532,-4.95,-27.8967890935119));
#44138=CARTESIAN_POINT('',(5.30749875712191,-4.95,1.42836055223659));
#44139=CARTESIAN_POINT('',(42.9102141453889,-4.95,-37.2328285521912));
#44140=CARTESIAN_POINT('',(9.19646652891232,-4.95,-12.7383571303816));
#44141=CARTESIAN_POINT('',(48.6705096178551,-4.95,-29.3044620073167));
#44142=CARTESIAN_POINT('',(61.1113340991292,-4.95,-12.181136115536));
#44143=CARTESIAN_POINT('',(9.29364304075393,-4.95,-0.695493819459823));
#44144=CARTESIAN_POINT('',(49.7136633514998,-4.95,-27.4976667405391));
#44145=CARTESIAN_POINT('',(17.4328197493865,-4.95,-13.1253091829197));
#44146=CARTESIAN_POINT('',(53.6996824536427,-4.95,-18.5449212556416));
#44147=CARTESIAN_POINT('',(63.7965499015051,-4.95,4.13301433349386));
#44148=CARTESIAN_POINT('',(15.0240206480311,-4.95,-1.32540719649159));
#44149=CARTESIAN_POINT('',(54.3443869165264,-4.95,-16.5607249438808));
#44150=CARTESIAN_POINT('',(26.5875812872166,-4.95,-10.6608337763716));
#44151=CARTESIAN_POINT('',(56.3819214865404,-4.95,-6.97487845668953));
#44152=CARTESIAN_POINT('',(62.01324415102,-4.95,19.5184117068093));
#44153=CARTESIAN_POINT('',(21.778082652094,-4.95,0.380394546543994));
#44154=CARTESIAN_POINT('',(-12.4,-4.95,-2.95));
#44155=CARTESIAN_POINT('',(-9.56543778402222,-4.95,-2.95));
#44156=CARTESIAN_POINT('',(6.,-4.95,-2.95));
#44157=CARTESIAN_POINT('',(-12.4,-4.95,2.95));
#44158=CARTESIAN_POINT('',(-12.4,-4.95,33.725));
#44159=CARTESIAN_POINT('',(-9.56543778402222,-4.95,2.95));
#44160=CARTESIAN_POINT('',(-6.,-4.95,2.95));
#44161=CARTESIAN_POINT('',(9.56543778402222,-4.95,2.95));
#44162=CARTESIAN_POINT('Origin',(0.,-4.95,0.));
#44163=CARTESIAN_POINT('',(12.4,-4.95,2.95));
#44164=CARTESIAN_POINT('',(-6.,-4.95,2.95));
#44165=CARTESIAN_POINT('',(12.4,-4.95,-2.95));
#44166=CARTESIAN_POINT('',(12.4,-4.95,36.275));
#44167=CARTESIAN_POINT('',(9.56543778402222,-4.95,-2.95));
#44168=CARTESIAN_POINT('',(6.,-4.95,-2.95));
#44169=CARTESIAN_POINT('Origin',(0.,-4.95,0.));
#44170=CARTESIAN_POINT('Origin',(35.5,-4.75,-4.7));
#44171=CARTESIAN_POINT('',(35.5,-4.55,-4.5));
#44172=CARTESIAN_POINT('Origin',(62.2088736711667,-4.75,19.4768293686457));
#44173=CARTESIAN_POINT('',(54.818810633147,-4.55,-16.2526305799144));
#44174=CARTESIAN_POINT('',(54.3443869165264,-4.95,-16.5607249438808));
#44175=CARTESIAN_POINT('',(56.6900158505068,-4.55,-7.44930217331016));
#44176=CARTESIAN_POINT('',(62.4045031913135,-4.55,19.4352470304822));
#44177=CARTESIAN_POINT('',(56.6900158505068,-4.55,-7.44930217331016));
#44178=CARTESIAN_POINT('Origin',(26.6291636253801,-4.75,-10.4652042562249));
#44179=CARTESIAN_POINT('',(26.6707459635437,-4.55,-10.2695747360781));
#44180=CARTESIAN_POINT('Origin',(21.7365003139304,-4.75,0.184765026397232));
#44181=CARTESIAN_POINT('',(21.6949179757669,-4.55,-0.0108644937495309));
#44182=CARTESIAN_POINT('Origin',(63.9792589930336,-4.75,4.05166700487871));
#44183=CARTESIAN_POINT('',(50.2417761917872,-4.55,-27.2949432147123));
#44184=CARTESIAN_POINT('',(49.7136633514998,-4.95,-27.4976667405391));
#44185=CARTESIAN_POINT('',(53.9024059794694,-4.55,-19.0730340959289));
#44186=CARTESIAN_POINT('',(64.1619680845621,-4.55,3.97031967626356));
#44187=CARTESIAN_POINT('',(53.9024059794694,-4.55,-19.0730340959289));
#44188=CARTESIAN_POINT('Origin',(17.5141670780017,-4.75,-12.9426000913912));
#44189=CARTESIAN_POINT('',(17.5955144066168,-4.55,-12.7598909998626));
#44190=CARTESIAN_POINT('Origin',(14.942673319416,-4.75,-1.50811628802011));
#44191=CARTESIAN_POINT('',(14.8613259908008,-4.55,-1.69082537954862));
#44192=CARTESIAN_POINT('Origin',(53.9024059794694,-4.95,-19.0730340959289));
#44193=CARTESIAN_POINT('',(53.9024059794694,-0.75,-19.0730340959289));
#44194=CARTESIAN_POINT('',(53.9024059794694,-4.95,-19.0730340959289));
#44195=CARTESIAN_POINT('',(66.6920423864658,-0.75,-24.7673470989901));
#44196=CARTESIAN_POINT('Origin',(50.2417761917872,-4.95,-27.2949432147123));
#44197=CARTESIAN_POINT('',(50.2417761917872,-0.75,-27.2949432147123));
#44198=CARTESIAN_POINT('',(50.2417761917872,-4.95,-27.2949432147123));
#44199=CARTESIAN_POINT('',(53.9024059794694,-0.75,-19.0730340959289));
#44200=CARTESIAN_POINT('Origin',(61.2731374980041,-4.75,-12.2986931659945));
#44201=CARTESIAN_POINT('',(43.4689350440559,-4.55,-37.1443358553582));
#44202=CARTESIAN_POINT('',(42.9102141453889,-4.95,-37.2328285521912));
#44203=CARTESIAN_POINT('',(48.7590023146881,-4.55,-29.8631829059837));
#44204=CARTESIAN_POINT('',(61.4349408968791,-4.55,-12.416250216453));
#44205=CARTESIAN_POINT('',(48.7590023146881,-4.55,-29.8631829059837));
#44206=CARTESIAN_POINT('Origin',(9.31402357937082,-4.75,-12.5765537315066));
#44207=CARTESIAN_POINT('',(9.43158062982931,-4.55,-12.4147503326316));
#44208=CARTESIAN_POINT('Origin',(9.17608599029544,-4.75,-0.85729721833481));
#44209=CARTESIAN_POINT('',(9.05852893983695,-4.55,-1.0191006172098));
#44210=CARTESIAN_POINT('Origin',(53.7386757528038,-4.75,-28.0454180586074));
#44211=CARTESIAN_POINT('',(34.7962928478066,-4.55,-45.3703427808263));
#44212=CARTESIAN_POINT('',(34.2313826750721,-4.95,-45.3407370931789));
#44213=CARTESIAN_POINT('',(41.4845962771032,-4.55,-39.3481673235966));
#44214=CARTESIAN_POINT('',(53.8725018740756,-4.55,-28.1940470237028));
#44215=CARTESIAN_POINT('',(41.4845962771032,-4.55,-39.3481673235966));
#44216=CARTESIAN_POINT('Origin',(2.85722267705093,-4.75,-10.1973070471502));
#44217=CARTESIAN_POINT('',(3.00585164214641,-4.55,-10.0634809258784));
#44218=CARTESIAN_POINT('Origin',(5.15886979202643,-4.75,1.29453443096482));
#44219=CARTESIAN_POINT('',(5.01024082693095,-4.55,1.16070830969305));
#44220=CARTESIAN_POINT('Origin',(41.4845962771032,-4.95,-39.3481673235966));
#44221=CARTESIAN_POINT('',(41.4845962771032,-0.75,-39.3481673235966));
#44222=CARTESIAN_POINT('',(41.4845962771032,-4.95,-39.3481673235966));
#44223=CARTESIAN_POINT('',(50.8524247661272,-0.75,-49.7521948802801));
#44224=CARTESIAN_POINT('Origin',(34.7962928478066,-4.95,-45.3703427808263));
#44225=CARTESIAN_POINT('',(34.7962928478066,-0.75,-45.3703427808263));
#44226=CARTESIAN_POINT('',(34.7962928478066,-4.95,-45.3703427808263));
#44227=CARTESIAN_POINT('',(41.4845962771032,-0.75,-39.3481673235966));
#44228=CARTESIAN_POINT('Origin',(41.6068874077127,-4.75,-41.5652429349561));
#44229=CARTESIAN_POINT('',(24.60288568297,-4.55,-51.613448015713));
#44230=CARTESIAN_POINT('',(24.0564755214563,-4.95,-51.4670378541992));
#44231=CARTESIAN_POINT('',(32.39711431703,-4.55,-47.113448015713));
#44232=CARTESIAN_POINT('',(41.7068874077127,-4.55,-41.738448015713));
#44233=CARTESIAN_POINT('',(32.39711431703,-4.55,-47.113448015713));
#44234=CARTESIAN_POINT('Origin',(-1.47576396401454,-4.75,-6.84390183434757));
#44235=CARTESIAN_POINT('',(-1.30255888325765,-4.55,-6.74390183434757));
#44236=CARTESIAN_POINT('Origin',(3.16487483155919,-4.75,3.91827599214349));
#44237=CARTESIAN_POINT('',(2.9916697508023,-4.55,3.8182759921435));
#44238=CARTESIAN_POINT('Origin',(25.6985300339512,-4.75,-51.3730957644699));
#44239=CARTESIAN_POINT('',(13.3342143560438,-4.55,-55.600797903511));
#44240=CARTESIAN_POINT('',(12.8301849517758,-4.95,-55.343982094743));
#44241=CARTESIAN_POINT('',(21.8937230027002,-4.55,-52.8196449541365));
#44242=CARTESIAN_POINT('',(25.7603334328262,-4.55,-51.563307067729));
#44243=CARTESIAN_POINT('',(21.8937230027002,-4.55,-52.8196449541365));
#44244=CARTESIAN_POINT('Origin',(-3.78610424139487,-4.75,-3.55708880047863));
#44245=CARTESIAN_POINT('',(-3.59589293813584,-4.55,-3.49528540160364));
#44246=CARTESIAN_POINT('Origin',(2.99070805115495,-4.75,6.00506656071195));
#44247=CARTESIAN_POINT('',(2.80049674789591,-4.55,5.94326316183696));
#44248=CARTESIAN_POINT('Origin',(21.8937230027002,-4.95,-52.8196449541365));
#44249=CARTESIAN_POINT('',(21.8937230027002,-0.75,-52.8196449541365));
#44250=CARTESIAN_POINT('',(21.8937230027002,-4.95,-52.8196449541365));
#44251=CARTESIAN_POINT('',(26.2199609239495,-0.75,-66.1344361822686));
#44252=CARTESIAN_POINT('Origin',(13.3342143560438,-4.95,-55.600797903511));
#44253=CARTESIAN_POINT('',(13.3342143560438,-0.75,-55.600797903511));
#44254=CARTESIAN_POINT('',(13.3342143560438,-4.95,-55.600797903511));
#44255=CARTESIAN_POINT('',(21.8937230027002,-0.75,-52.8196449541365));
#44256=CARTESIAN_POINT('Origin',(4.01485952204822,-4.75,6.76499277220378));
#44257=CARTESIAN_POINT('',(10.4334709354135,-4.55,-56.2173699512871));
#44258=CARTESIAN_POINT('',(19.4842239220056,-14.7194604253764,-45.0406208236431));
#44259=CARTESIAN_POINT('',(3.81595514297456,-4.55,6.74408707955025));
#44260=CARTESIAN_POINT('Origin',(7.33799703833491,-4.75,-56.3416157121117));
#44261=CARTESIAN_POINT('',(1.48277387709903,-4.55,-57.158126120696));
#44262=CARTESIAN_POINT('',(7.35890273098844,-4.55,-56.5405200911854));
#44263=CARTESIAN_POINT('',(1.04315373364466,-4.95,-56.8021287478558));
#44264=CARTESIAN_POINT('Origin',(-4.60194705153997,-4.75,-1.17922805009007));
#44265=CARTESIAN_POINT('',(-4.40304267246632,-4.55,-1.15832235743654));
#44266=CARTESIAN_POINT('Origin',(-11.8133455674921,-4.75,-55.8712376274073));
#44267=CARTESIAN_POINT('',(-10.4334709354135,-4.55,-56.2173699512871));
#44268=CARTESIAN_POINT('',(-10.7894683082537,-4.95,-55.7777498078328));
#44269=CARTESIAN_POINT('',(-1.48277387709901,-4.55,-57.158126120696));
#44270=CARTESIAN_POINT('',(-11.8342512601456,-4.55,-56.070142006481));
#44271=CARTESIAN_POINT('',(-1.48277387709901,-4.55,-57.158126120696));
#44272=CARTESIAN_POINT('Origin',(-4.74655876492179,-4.75,-0.196660495374136));
#44273=CARTESIAN_POINT('',(-4.54765438584814,-4.55,-0.217566188027667));
#44274=CARTESIAN_POINT('Origin',(5.33364629441355,-4.75,5.78242521748784));
#44275=CARTESIAN_POINT('',(5.13474191533989,-4.55,5.80333091014137));
#44276=CARTESIAN_POINT('Origin',(-29.9782843572794,-4.75,-49.9825192897827));
#44277=CARTESIAN_POINT('',(-21.8937230027002,-4.55,-52.8196449541365));
#44278=CARTESIAN_POINT('',(-22.1505388114683,-4.95,-52.3156155498685));
#44279=CARTESIAN_POINT('',(-13.3342143560438,-4.55,-55.600797903511));
#44280=CARTESIAN_POINT('',(-30.0400877561544,-4.55,-50.1727305930417));
#44281=CARTESIAN_POINT('',(-13.3342143560438,-4.55,-55.600797903511));
#44282=CARTESIAN_POINT('Origin',(-5.15382701177957,-4.75,-0.652329053354118));
#44283=CARTESIAN_POINT('',(-4.96361570852054,-4.55,-0.714132452229108));
#44284=CARTESIAN_POINT('Origin',(5.9492232020195,-4.75,3.10030681358745));
#44285=CARTESIAN_POINT('',(5.75901189876047,-4.55,3.16211021246244));
#44286=CARTESIAN_POINT('Origin',(-13.3342143560438,-4.95,-55.600797903511));
#44287=CARTESIAN_POINT('',(-13.3342143560438,-0.75,-55.600797903511));
#44288=CARTESIAN_POINT('',(-13.3342143560438,-4.95,-55.600797903511));
#44289=CARTESIAN_POINT('',(-17.6604522772931,-0.75,-68.9155891316432));
#44290=CARTESIAN_POINT('Origin',(-21.8937230027002,-4.95,-52.8196449541365));
#44291=CARTESIAN_POINT('',(-21.8937230027002,-0.75,-52.8196449541365));
#44292=CARTESIAN_POINT('',(-21.8937230027002,-4.95,-52.8196449541365));
#44293=CARTESIAN_POINT('',(-13.3342143560438,-0.75,-55.600797903511));
#44294=CARTESIAN_POINT('Origin',(-45.5040017247427,-4.75,-39.3152429349561));
#44295=CARTESIAN_POINT('',(-32.39711431703,-4.55,-47.113448015713));
#44296=CARTESIAN_POINT('',(-32.5435244785437,-4.95,-46.5670378541992));
#44297=CARTESIAN_POINT('',(-24.60288568297,-4.55,-51.613448015713));
#44298=CARTESIAN_POINT('',(-45.6040017247427,-4.55,-39.488448015713));
#44299=CARTESIAN_POINT('',(-24.60288568297,-4.55,-51.613448015713));
#44300=CARTESIAN_POINT('Origin',(-6.66487483155918,-4.75,-2.14390183434758));
#44301=CARTESIAN_POINT('',(-6.49166975080229,-4.55,-2.24390183434758));
#44302=CARTESIAN_POINT('Origin',(4.97576396401454,-4.75,-0.781724007856504));
#44303=CARTESIAN_POINT('',(4.80255888325765,-4.55,-0.681724007856502));
#44304=CARTESIAN_POINT('Origin',(-57.082827467452,-4.75,-25.0343303299925));
#44305=CARTESIAN_POINT('',(-41.4845962771032,-4.55,-39.3481673235966));
#44306=CARTESIAN_POINT('',(-41.5142019647506,-4.95,-38.7832571508621));
#44307=CARTESIAN_POINT('',(-34.7962928478066,-4.55,-45.3703427808263));
#44308=CARTESIAN_POINT('',(-57.2166535887238,-4.55,-25.182959295088));
#44309=CARTESIAN_POINT('',(-34.7962928478066,-4.55,-45.3703427808263));
#44310=CARTESIAN_POINT('Origin',(-9.84278403653842,-4.75,-3.90747934737692));
#44311=CARTESIAN_POINT('',(-9.69415507144295,-4.55,-4.04130546864869));
#44312=CARTESIAN_POINT('Origin',(1.82669156746108,-4.75,-4.99529326880842));
#44313=CARTESIAN_POINT('',(1.6780626023656,-4.55,-4.86146714753665));
#44314=CARTESIAN_POINT('Origin',(-34.7962928478066,-4.95,-45.3703427808263));
#44315=CARTESIAN_POINT('',(-34.7962928478066,-0.75,-45.3703427808263));
#44316=CARTESIAN_POINT('',(-34.7962928478066,-4.95,-45.3703427808263));
#44317=CARTESIAN_POINT('',(-44.1641213368306,-0.75,-55.7743703375099));
#44318=CARTESIAN_POINT('Origin',(-41.4845962771032,-4.95,-39.3481673235966));
#44319=CARTESIAN_POINT('',(-41.4845962771032,-0.75,-39.3481673235966));
#44320=CARTESIAN_POINT('',(-41.4845962771032,-4.95,-39.3481673235966));
#44321=CARTESIAN_POINT('',(-34.7962928478066,-0.75,-45.3703427808263));
#44322=CARTESIAN_POINT('Origin',(-63.9181711333203,-4.75,-8.65811669130728));
#44323=CARTESIAN_POINT('',(-48.7590023146881,-4.55,-29.8631829059837));
#44324=CARTESIAN_POINT('',(-48.6705096178552,-4.95,-29.3044620073167));
#44325=CARTESIAN_POINT('',(-43.4689350440559,-4.55,-37.1443358553582));
#44326=CARTESIAN_POINT('',(-64.0799745321953,-4.55,-8.77567374176577));
#44327=CARTESIAN_POINT('',(-43.4689350440559,-4.55,-37.1443358553582));
#44328=CARTESIAN_POINT('Origin',(-14.8392049509201,-4.75,-4.97179398438211));
#44329=CARTESIAN_POINT('',(-14.7216479004616,-4.55,-5.1335973832571));
#44330=CARTESIAN_POINT('Origin',(-3.65090461874619,-4.75,-8.46205696545931));
#44331=CARTESIAN_POINT('',(-3.76846166920468,-4.55,-8.30025356658432));
#44332=CARTESIAN_POINT('Origin',(-65.8095738868747,-4.75,8.1626215642704));
#44333=CARTESIAN_POINT('',(-53.9024059794693,-4.55,-19.0730340959289));
#44334=CARTESIAN_POINT('',(-53.6996824536426,-4.95,-18.5449212556416));
#44335=CARTESIAN_POINT('',(-50.2417761917871,-4.55,-27.2949432147123));
#44336=CARTESIAN_POINT('',(-65.9922829784032,-4.55,8.08127423565524));
#44337=CARTESIAN_POINT('',(-50.2417761917871,-4.55,-27.2949432147123));
#44338=CARTESIAN_POINT('Origin',(-21.3374915229142,-4.75,-4.3552727895507));
#44339=CARTESIAN_POINT('',(-21.256144194299,-4.55,-4.53798188107922));
#44340=CARTESIAN_POINT('Origin',(-11.1193488745035,-4.75,-10.0954435898605));
#44341=CARTESIAN_POINT('',(-11.2006962031186,-4.55,-9.91273449833203));
#44342=CARTESIAN_POINT('Origin',(-50.2417761917871,-4.95,-27.2949432147123));
#44343=CARTESIAN_POINT('',(-50.2417761917871,-0.75,-27.2949432147123));
#44344=CARTESIAN_POINT('',(-50.2417761917871,-4.95,-27.2949432147123));
#44345=CARTESIAN_POINT('',(-63.0314125987836,-0.75,-32.9892562177735));
#44346=CARTESIAN_POINT('Origin',(-53.9024059794693,-4.95,-19.0730340959289));
#44347=CARTESIAN_POINT('',(-53.9024059794693,-0.75,-19.0730340959289));
#44348=CARTESIAN_POINT('',(-53.9024059794693,-4.95,-19.0730340959289));
#44349=CARTESIAN_POINT('',(-50.2417761917871,-0.75,-27.2949432147123));
#44350=CARTESIAN_POINT('Origin',(-63.1444762798466,-4.75,23.8784935719478));
#44351=CARTESIAN_POINT('',(-56.6900158505068,-4.55,-7.44930217331018));
#44352=CARTESIAN_POINT('',(-56.3819214865404,-4.95,-6.97487845668956));
#44353=CARTESIAN_POINT('',(-54.818810633147,-4.55,-16.2526305799144));
#44354=CARTESIAN_POINT('',(-63.3401057999934,-4.55,23.8369112337843));
#44355=CARTESIAN_POINT('',(-54.818810633147,-4.55,-16.2526305799144));
#44356=CARTESIAN_POINT('Origin',(-28.5835335190671,-4.75,-1.27061680932709));
#44357=CARTESIAN_POINT('',(-28.5419511809035,-4.55,-1.46624632947385));
#44358=CARTESIAN_POINT('Origin',(-19.7821304202435,-4.75,-9.00982242050055));
#44359=CARTESIAN_POINT('',(-19.823712758407,-4.55,-8.81419290035379));
#44360=CARTESIAN_POINT('Origin',(-56.8,-4.75,37.25));
#44361=CARTESIAN_POINT('',(-57.,-4.55,4.49999999999999));
#44362=CARTESIAN_POINT('',(-56.6,-4.95,4.9));
#44363=CARTESIAN_POINT('',(-57.,-4.55,-4.50000000000001));
#44364=CARTESIAN_POINT('',(-57.,-4.55,37.25));
#44365=CARTESIAN_POINT('',(-57.,-4.55,-4.50000000000001));
#44366=CARTESIAN_POINT('Origin',(-35.5,-4.75,4.7));
#44367=CARTESIAN_POINT('',(-35.5,-4.55,4.5));
#44368=CARTESIAN_POINT('Origin',(-28.5,-4.75,-4.70000000000001));
#44369=CARTESIAN_POINT('',(-28.5,-4.55,-4.5));
#44370=CARTESIAN_POINT('Origin',(-57.,-4.95,-4.50000000000001));
#44371=CARTESIAN_POINT('',(-57.,-0.75,-4.50000000000001));
#44372=CARTESIAN_POINT('',(-57.,-4.95,-4.50000000000001));
#44373=CARTESIAN_POINT('',(-71.,-0.75,-4.50000000000001));
#44374=CARTESIAN_POINT('Origin',(-57.,-4.95,4.49999999999999));
#44375=CARTESIAN_POINT('',(-57.,-0.75,4.49999999999999));
#44376=CARTESIAN_POINT('',(-57.,-4.95,4.49999999999999));
#44377=CARTESIAN_POINT('',(-57.,-0.75,-4.50000000000001));
#44378=CARTESIAN_POINT('Origin',(-47.9730911635137,-4.75,47.4972616488453));
#44379=CARTESIAN_POINT('',(-54.818810633147,-4.55,16.2526305799144));
#44380=CARTESIAN_POINT('',(-54.3443869165264,-4.95,16.5607249438808));
#44381=CARTESIAN_POINT('',(-56.6900158505068,-4.55,7.44930217331014));
#44382=CARTESIAN_POINT('',(-48.1687206836605,-4.55,47.5388439870088));
#44383=CARTESIAN_POINT('',(-56.6900158505068,-4.55,7.44930217331014));
#44384=CARTESIAN_POINT('Origin',(-40.8649461330331,-4.75,13.4911132387338));
#44385=CARTESIAN_POINT('',(-40.9065284711967,-4.55,13.2954837185871));
#44386=CARTESIAN_POINT('Origin',(-35.9722828215834,-4.75,2.84114395611173));
#44387=CARTESIAN_POINT('',(-35.9307004834199,-4.55,3.03677347625849));
#44388=CARTESIAN_POINT('Origin',(-37.9691901013248,-4.75,54.3679042176813));
#44389=CARTESIAN_POINT('',(-50.2417761917872,-4.55,27.2949432147123));
#44390=CARTESIAN_POINT('',(-49.7136633514998,-4.95,27.497666740539));
#44391=CARTESIAN_POINT('',(-53.9024059794694,-4.55,19.0730340959289));
#44392=CARTESIAN_POINT('',(-38.1518991928533,-4.55,54.4492515462965));
#44393=CARTESIAN_POINT('',(-53.9024059794694,-4.55,19.0730340959289));
#44394=CARTESIAN_POINT('Origin',(-43.5242359697105,-4.75,24.5230288688311));
#44395=CARTESIAN_POINT('',(-43.6055832983256,-4.55,24.3403197773026));
#44396=CARTESIAN_POINT('Origin',(-40.9527422111248,-4.75,13.08854506546));
#44397=CARTESIAN_POINT('',(-40.8713948825096,-4.55,13.2712541569886));
#44398=CARTESIAN_POINT('Origin',(-53.9024059794694,-4.95,19.0730340959289));
#44399=CARTESIAN_POINT('',(-53.9024059794694,-0.75,19.0730340959289));
#44400=CARTESIAN_POINT('',(-53.9024059794694,-4.95,19.0730340959289));
#44401=CARTESIAN_POINT('',(-66.6920423864658,-0.75,24.7673470989901));
#44402=CARTESIAN_POINT('Origin',(-50.2417761917872,-4.95,27.2949432147123));
#44403=CARTESIAN_POINT('',(-50.2417761917872,-0.75,27.2949432147123));
#44404=CARTESIAN_POINT('',(-50.2417761917872,-4.95,27.2949432147123));
#44405=CARTESIAN_POINT('',(-53.9024059794694,-0.75,19.0730340959289));
#44406=CARTESIAN_POINT('Origin',(-27.9861594276738,-4.75,58.1142879691177));
#44407=CARTESIAN_POINT('',(-43.4689350440559,-4.55,37.1443358553582));
#44408=CARTESIAN_POINT('',(-42.9102141453889,-4.95,37.2328285521912));
#44409=CARTESIAN_POINT('',(-48.7590023146881,-4.55,29.8631829059837));
#44410=CARTESIAN_POINT('',(-28.1479628265488,-4.55,58.2318450195762));
#44411=CARTESIAN_POINT('',(-48.7590023146881,-4.55,29.8631829059837));
#44412=CARTESIAN_POINT('Origin',(-42.6010016497012,-4.75,36.7609589283835));
#44413=CARTESIAN_POINT('',(-42.7185587001597,-4.55,36.5991555295085));
#44414=CARTESIAN_POINT('Origin',(-42.4630640606258,-4.75,25.0417024152116));
#44415=CARTESIAN_POINT('',(-42.3455070101673,-4.55,25.2035058140866));
#44416=CARTESIAN_POINT('Origin',(-18.9304094149142,-4.75,59.3869218442395));
#44417=CARTESIAN_POINT('',(-34.7962928478067,-4.55,45.3703427808263));
#44418=CARTESIAN_POINT('',(-34.2313826750722,-4.95,45.3407370931789));
#44419=CARTESIAN_POINT('',(-41.4845962771032,-4.55,39.3481673235966));
#44420=CARTESIAN_POINT('',(-19.064235536186,-4.55,59.535550809335));
#44421=CARTESIAN_POINT('',(-41.4845962771032,-4.55,39.3481673235966));
#44422=CARTESIAN_POINT('Origin',(-37.6654890149405,-4.75,48.855803261518));
#44423=CARTESIAN_POINT('',(-37.814117980036,-4.55,48.7219771402463));
#44424=CARTESIAN_POINT('Origin',(-39.967136129916,-4.75,37.363961783403));
#44425=CARTESIAN_POINT('',(-39.8185071648205,-4.55,37.4977879046748));
#44426=CARTESIAN_POINT('Origin',(-41.4845962771032,-4.95,39.3481673235966));
#44427=CARTESIAN_POINT('',(-41.4845962771032,-0.75,39.3481673235966));
#44428=CARTESIAN_POINT('',(-41.4845962771032,-4.95,39.3481673235966));
#44429=CARTESIAN_POINT('',(-50.8524247661272,-0.75,49.7521948802801));
#44430=CARTESIAN_POINT('Origin',(-34.7962928478067,-4.95,45.3703427808263));
#44431=CARTESIAN_POINT('',(-34.7962928478067,-0.75,45.3703427808263));
#44432=CARTESIAN_POINT('',(-34.7962928478067,-4.95,45.3703427808263));
#44433=CARTESIAN_POINT('',(-41.4845962771032,-0.75,39.3481673235966));
#44434=CARTESIAN_POINT('Origin',(-11.2959982752574,-4.75,59.0652429349561));
#44435=CARTESIAN_POINT('',(-24.6028856829701,-4.55,51.613448015713));
#44436=CARTESIAN_POINT('',(-22.9547507919904,-5.75651847792408,51.1718316026574));
#44437=CARTESIAN_POINT('',(-32.39711431703,-4.55,47.113448015713));
#44438=CARTESIAN_POINT('',(-11.3959982752574,-4.55,59.238448015713));
#44439=CARTESIAN_POINT('',(-32.39711431703,-4.55,47.113448015713));
#44440=CARTESIAN_POINT('Origin',(-33.4757639640146,-4.75,48.5817240078565));
#44441=CARTESIAN_POINT('',(-33.3025588832577,-4.55,48.6817240078565));
#44442=CARTESIAN_POINT('Origin',(-28.8351251684408,-4.75,59.3439018343476));
#44443=CARTESIAN_POINT('',(-29.0083302491977,-4.55,59.2439018343476));
#44444=CARTESIAN_POINT('Origin',(-5.12604620371464,-4.75,58.0575009613468));
#44445=CARTESIAN_POINT('',(-13.3342143560438,-4.55,55.600797903511));
#44446=CARTESIAN_POINT('',(-12.8301849517758,-4.95,55.3439820947429));
#44447=CARTESIAN_POINT('',(-21.8937230027002,-4.55,52.8196449541365));
#44448=CARTESIAN_POINT('',(-5.18784960258963,-4.55,58.2477122646058));
#44449=CARTESIAN_POINT('',(-21.8937230027002,-4.55,52.8196449541365));
#44450=CARTESIAN_POINT('Origin',(-16.7863795888417,-4.75,66.8726836036018));
#44451=CARTESIAN_POINT('',(-16.9765908921007,-4.55,66.8108802047268));
#44452=CARTESIAN_POINT('Origin',(-23.5631918813915,-4.75,57.3105282424112));
#44453=CARTESIAN_POINT('',(-23.3729805781325,-4.55,57.3723316412862));
#44454=CARTESIAN_POINT('Origin',(-0.0610878597133323,-4.75,57.1064496864285));
#44455=CARTESIAN_POINT('',(-1.48277387709906,-4.55,57.158126120696));
#44456=CARTESIAN_POINT('',(-1.04315373364469,-4.95,56.8021287478558));
#44457=CARTESIAN_POINT('',(-10.4334709354135,-4.55,56.2173699512871));
#44458=CARTESIAN_POINT('',(-0.0819935523668635,-4.55,57.3053540655022));
#44459=CARTESIAN_POINT('',(-10.4334709354135,-4.55,56.2173699512871));
#44460=CARTESIAN_POINT('Origin',(-2.67496212708166,-4.75,70.4143940757733));
#44461=CARTESIAN_POINT('',(-2.87386650615531,-4.55,70.3934883831197));
#44462=CARTESIAN_POINT('Origin',(-11.2917687006698,-4.75,62.4701732534794));
#44463=CARTESIAN_POINT('',(-11.0928643215962,-4.55,62.4910789461329));
#44464=CARTESIAN_POINT('Origin',(-10.4334709354135,-4.95,56.2173699512871));
#44465=CARTESIAN_POINT('',(-10.4334709354135,-0.75,56.2173699512871));
#44466=CARTESIAN_POINT('',(-10.4334709354135,-4.95,56.2173699512871));
#44467=CARTESIAN_POINT('',(-11.8968694211607,-0.75,70.140676486443));
#44468=CARTESIAN_POINT('Origin',(-1.48277387709906,-4.95,57.158126120696));
#44469=CARTESIAN_POINT('',(-1.48277387709906,-0.75,57.158126120696));
#44470=CARTESIAN_POINT('',(-1.48277387709906,-4.95,57.158126120696));
#44471=CARTESIAN_POINT('',(-10.4334709354135,-0.75,56.2173699512871));
#44472=CARTESIAN_POINT('Origin',(4.53643638887053,-4.75,56.6360716017241));
#44473=CARTESIAN_POINT('',(10.4334709354135,-4.55,56.2173699512871));
#44474=CARTESIAN_POINT('',(10.7894683082537,-4.95,55.7777498078328));
#44475=CARTESIAN_POINT('',(1.48277387709899,-4.55,57.158126120696));
#44476=CARTESIAN_POINT('',(4.55734208152406,-4.55,56.8349759807978));
#44477=CARTESIAN_POINT('',(1.48277387709899,-4.55,57.158126120696));
#44478=CARTESIAN_POINT('Origin',(12.0234679435433,-4.75,69.4318265210573));
#44479=CARTESIAN_POINT('',(11.8245635644697,-4.55,69.4527322137109));
#44480=CARTESIAN_POINT('Origin',(1.943262884208,-4.75,63.4527408081954));
#44481=CARTESIAN_POINT('',(2.14216726328165,-4.55,63.4318351155418));
#44482=CARTESIAN_POINT('Origin',(9.40580052704283,-4.75,56.6669244866595));
#44483=CARTESIAN_POINT('',(21.8937230027002,-4.55,52.8196449541365));
#44484=CARTESIAN_POINT('',(22.1505388114683,-4.95,52.3156155498685));
#44485=CARTESIAN_POINT('',(13.3342143560438,-4.55,55.600797903511));
#44486=CARTESIAN_POINT('',(9.46760392591782,-4.55,56.8571357899185));
#44487=CARTESIAN_POINT('',(13.3342143560438,-4.55,55.600797903511));
#44488=CARTESIAN_POINT('Origin',(25.7263108420161,-4.75,63.9679238564773));
#44489=CARTESIAN_POINT('',(25.5360995387571,-4.55,64.0297272553523));
#44490=CARTESIAN_POINT('Origin',(14.6232606282171,-4.75,60.2152879895357));
#44491=CARTESIAN_POINT('',(14.8134719314761,-4.55,60.1534845906607));
#44492=CARTESIAN_POINT('Origin',(13.3342143560438,-4.95,55.600797903511));
#44493=CARTESIAN_POINT('',(13.3342143560438,-0.75,55.600797903511));
#44494=CARTESIAN_POINT('',(13.3342143560438,-4.95,55.600797903511));
#44495=CARTESIAN_POINT('',(17.6604522772931,-0.75,68.9155891316432));
#44496=CARTESIAN_POINT('Origin',(21.8937230027002,-4.95,52.8196449541365));
#44497=CARTESIAN_POINT('',(21.8937230027002,-0.75,52.8196449541365));
#44498=CARTESIAN_POINT('',(21.8937230027002,-4.95,52.8196449541365));
#44499=CARTESIAN_POINT('',(13.3342143560438,-0.75,55.600797903511));
#44500=CARTESIAN_POINT('Origin',(15.1931125922873,-4.75,56.8152429349561));
#44501=CARTESIAN_POINT('',(32.3971143170299,-4.55,47.113448015713));
#44502=CARTESIAN_POINT('',(32.5435244785437,-4.95,46.5670378541993));
#44503=CARTESIAN_POINT('',(24.60288568297,-4.55,51.613448015713));
#44504=CARTESIAN_POINT('',(15.2931125922873,-4.55,56.988448015713));
#44505=CARTESIAN_POINT('',(24.60288568297,-4.55,51.613448015713));
#44506=CARTESIAN_POINT('Origin',(36.9757639640145,-4.75,54.6439018343476));
#44507=CARTESIAN_POINT('',(36.8025588832576,-4.55,54.7439018343476));
#44508=CARTESIAN_POINT('Origin',(25.3351251684408,-4.75,53.2817240078565));
#44509=CARTESIAN_POINT('',(25.5083302491977,-4.55,53.1817240078565));
#44510=CARTESIAN_POINT('Origin',(22.2745611295625,-4.75,56.3758341156246));
#44511=CARTESIAN_POINT('',(41.4845962771032,-4.55,39.3481673235966));
#44512=CARTESIAN_POINT('',(41.5142019647506,-4.95,38.7832571508621));
#44513=CARTESIAN_POINT('',(34.7962928478066,-4.55,45.3703427808264));
#44514=CARTESIAN_POINT('',(22.4083872508343,-4.55,56.5244630807201));
#44515=CARTESIAN_POINT('',(34.7962928478066,-4.55,45.3703427808264));
#44516=CARTESIAN_POINT('Origin',(44.651050374428,-4.75,42.5659755617448));
#44517=CARTESIAN_POINT('',(44.5024214093325,-4.55,42.6998016830166));
#44518=CARTESIAN_POINT('Origin',(32.9815747704285,-4.75,43.6537894831763));
#44519=CARTESIAN_POINT('',(33.130203735524,-4.55,43.5199633619046));
#44520=CARTESIAN_POINT('Origin',(34.7962928478066,-4.95,45.3703427808264));
#44521=CARTESIAN_POINT('',(34.7962928478066,-0.75,45.3703427808264));
#44522=CARTESIAN_POINT('',(34.7962928478066,-4.95,45.3703427808264));
#44523=CARTESIAN_POINT('',(44.1641213368306,-0.75,55.7743703375099));
#44524=CARTESIAN_POINT('Origin',(41.4845962771032,-4.95,39.3481673235966));
#44525=CARTESIAN_POINT('',(41.4845962771032,-0.75,39.3481673235966));
#44526=CARTESIAN_POINT('',(41.4845962771032,-4.95,39.3481673235966));
#44527=CARTESIAN_POINT('',(34.7962928478066,-0.75,45.3703427808264));
#44528=CARTESIAN_POINT('Origin',(36.9378826890766,-4.75,32.6464621623362));
#44529=CARTESIAN_POINT('',(43.4689350440559,-4.55,37.1443358553582));
#44530=CARTESIAN_POINT('',(36.416687466477,-9.59885182881449,38.2613021409633));
#44531=CARTESIAN_POINT('',(37.0554397395351,-4.55,32.4846587634612));
#44532=CARTESIAN_POINT('Origin',(30.6311930629899,-4.75,54.4737114944304));
#44533=CARTESIAN_POINT('',(48.7590023146881,-4.55,29.8631829059837));
#44534=CARTESIAN_POINT('',(30.7929964618649,-4.55,54.5912685448889));
#44535=CARTESIAN_POINT('',(48.6705096178552,-4.95,29.3044620073168));
#44536=CARTESIAN_POINT('Origin',(48.1261830212504,-4.75,29.156199181259));
#44537=CARTESIAN_POINT('',(48.0086259707919,-4.55,29.318002580134));
#44538=CARTESIAN_POINT('Origin',(39.7995049951658,-4.75,50.2569496582896));
#44539=CARTESIAN_POINT('',(53.9024059794693,-4.55,19.0730340959289));
#44540=CARTESIAN_POINT('',(53.6996824536426,-4.95,18.5449212556416));
#44541=CARTESIAN_POINT('',(50.2417761917871,-4.55,27.2949432147124));
#44542=CARTESIAN_POINT('',(39.9822140866944,-4.55,50.3382969869048));
#44543=CARTESIAN_POINT('',(50.2417761917871,-4.55,27.2949432147124));
#44544=CARTESIAN_POINT('Origin',(47.347560414623,-4.75,15.9357015669907));
#44545=CARTESIAN_POINT('',(47.2662130860078,-4.55,16.1184106585192));
#44546=CARTESIAN_POINT('Origin',(37.1294177662123,-4.75,21.6758723673006));
#44547=CARTESIAN_POINT('',(37.2107650948274,-4.55,21.493163275772));
#44548=CARTESIAN_POINT('Origin',(48.9086937721936,-4.75,43.0955974455432));
#44549=CARTESIAN_POINT('',(56.6900158505068,-4.55,7.44930217331019));
#44550=CARTESIAN_POINT('',(56.3819214865404,-4.95,6.97487845668957));
#44551=CARTESIAN_POINT('',(54.818810633147,-4.55,16.2526305799144));
#44552=CARTESIAN_POINT('',(49.1043232923404,-4.55,43.1371797837068));
#44553=CARTESIAN_POINT('',(54.818810633147,-4.55,16.2526305799144));
#44554=CARTESIAN_POINT('Origin',(42.8193160267201,-4.75,4.29652579183608));
#44555=CARTESIAN_POINT('',(42.7777336885565,-4.55,4.49215531198284));
#44556=CARTESIAN_POINT('Origin',(34.0179129278965,-4.75,12.0357314030095));
#44557=CARTESIAN_POINT('',(34.0594952660601,-4.55,11.8401018828628));
#44558=CARTESIAN_POINT('Origin',(54.818810633147,-4.95,16.2526305799144));
#44559=CARTESIAN_POINT('',(54.818810633147,-0.75,16.2526305799144));
#44560=CARTESIAN_POINT('',(54.818810633147,-4.95,16.2526305799144));
#44561=CARTESIAN_POINT('',(68.5128770434203,-0.75,19.1633942513631));
#44562=CARTESIAN_POINT('Origin',(56.6900158505068,-4.95,7.44930217331019));
#44563=CARTESIAN_POINT('',(56.6900158505068,-0.75,7.44930217331019));
#44564=CARTESIAN_POINT('',(56.6900158505068,-4.95,7.44930217331019));
#44565=CARTESIAN_POINT('',(54.818810633147,-0.75,16.2526305799144));
#44566=CARTESIAN_POINT('Origin',(-12.2,4.75,3.73));
#44567=CARTESIAN_POINT('',(-12.,4.55,2.55));
#44568=CARTESIAN_POINT('',(-12.4,4.95,2.95));
#44569=CARTESIAN_POINT('',(-12.,4.55,-2.55));
#44570=CARTESIAN_POINT('',(-12.,4.55,3.73));
#44571=CARTESIAN_POINT('',(-12.,4.55,-2.55));
#44572=CARTESIAN_POINT('Origin',(-6.,4.75,2.75));
#44573=CARTESIAN_POINT('',(-9.67975206294045,4.55,2.55));
#44574=CARTESIAN_POINT('Origin',(0.,1.99999999999999,0.));
#44575=CARTESIAN_POINT('',(-6.,4.55,2.55));
#44576=CARTESIAN_POINT('Origin',(6.,4.75,-2.75));
#44577=CARTESIAN_POINT('',(-9.67975206294045,4.55,-2.55));
#44578=CARTESIAN_POINT('',(6.,4.55,-2.55));
#44579=CARTESIAN_POINT('Origin',(0.,1.99999999999999,0.));
#44580=CARTESIAN_POINT('Origin',(12.,-4.95,-2.55));
#44581=CARTESIAN_POINT('',(-12.,-4.55,-2.55));
#44582=CARTESIAN_POINT('',(-12.,-4.95,-2.55));
#44583=CARTESIAN_POINT('',(-9.67975206294045,-4.55,-2.55));
#44584=CARTESIAN_POINT('',(6.,-4.55,-2.55));
#44585=CARTESIAN_POINT('',(-9.67975206294045,0.,-2.55));
#44586=CARTESIAN_POINT('Origin',(-12.,-4.95,-2.55));
#44587=CARTESIAN_POINT('',(-12.,-4.55,2.55));
#44588=CARTESIAN_POINT('',(-12.,-4.95,2.55));
#44589=CARTESIAN_POINT('',(-12.,-4.55,33.725));
#44590=CARTESIAN_POINT('Origin',(-12.,-4.95,2.55));
#44591=CARTESIAN_POINT('',(-9.67975206294045,-4.55,2.55));
#44592=CARTESIAN_POINT('',(-9.67975206294045,0.,2.55));
#44593=CARTESIAN_POINT('',(-6.,-4.55,2.55));
#44594=CARTESIAN_POINT('Origin',(0.,0.,0.));
#44595=CARTESIAN_POINT('',(9.67975206294045,4.55,2.55));
#44596=CARTESIAN_POINT('Origin',(0.,1.99999999999999,0.));
#44597=CARTESIAN_POINT('',(9.67975206294045,-4.55,2.55));
#44598=CARTESIAN_POINT('',(9.67975206294045,0.,2.55));
#44599=CARTESIAN_POINT('Origin',(0.,-1.99999999999999,0.));
#44600=CARTESIAN_POINT('Origin',(0.,-1.99999999999999,0.));
#44601=CARTESIAN_POINT('Origin',(-12.2,-4.75,33.725));
#44602=CARTESIAN_POINT('',(-12.,-4.55,2.55));
#44603=CARTESIAN_POINT('',(-12.4,-4.95,-2.95));
#44604=CARTESIAN_POINT('Origin',(-6.,-4.75,2.75));
#44605=CARTESIAN_POINT('Origin',(6.,-4.75,-2.75));
#44606=CARTESIAN_POINT('Origin',(0.,-1.99999999999999,0.));
#44607=CARTESIAN_POINT('Origin',(6.,-4.75,-2.75));
#44608=CARTESIAN_POINT('',(12.,-4.55,-2.55));
#44609=CARTESIAN_POINT('',(9.67975206294045,-4.55,-2.55));
#44610=CARTESIAN_POINT('',(6.,-4.55,-2.55));
#44611=CARTESIAN_POINT('Origin',(0.,-1.99999999999999,0.));
#44612=CARTESIAN_POINT('',(12.4,-4.95,-2.95));
#44613=CARTESIAN_POINT('Origin',(12.2,-4.75,36.275));
#44614=CARTESIAN_POINT('',(12.,-4.55,2.55));
#44615=CARTESIAN_POINT('',(12.4,-4.95,2.95));
#44616=CARTESIAN_POINT('',(12.,-4.55,36.275));
#44617=CARTESIAN_POINT('Origin',(-6.,-4.75,2.75));
#44618=CARTESIAN_POINT('',(-6.,-4.55,2.55));
#44619=CARTESIAN_POINT('Origin',(12.,-4.95,-2.55));
#44620=CARTESIAN_POINT('',(12.,4.55,-2.55));
#44621=CARTESIAN_POINT('',(12.,-4.95,-2.55));
#44622=CARTESIAN_POINT('',(9.67975206294045,4.55,-2.55));
#44623=CARTESIAN_POINT('',(6.,4.55,-2.55));
#44624=CARTESIAN_POINT('',(9.67975206294045,0.,-2.55));
#44625=CARTESIAN_POINT('Origin',(12.,-4.95,2.55));
#44626=CARTESIAN_POINT('',(12.,4.55,2.55));
#44627=CARTESIAN_POINT('',(12.,-4.95,2.55));
#44628=CARTESIAN_POINT('',(12.,4.55,6.28));
#44629=CARTESIAN_POINT('Origin',(-12.,-4.95,2.55));
#44630=CARTESIAN_POINT('',(-6.,4.55,2.55));
#44631=CARTESIAN_POINT('Origin',(6.,4.75,-2.75));
#44632=CARTESIAN_POINT('Origin',(0.,1.99999999999999,0.));
#44633=CARTESIAN_POINT('',(12.,4.55,-2.55));
#44634=CARTESIAN_POINT('Origin',(12.2,4.75,6.28));
#44635=CARTESIAN_POINT('',(12.,4.55,2.55));
#44636=CARTESIAN_POINT('Origin',(-6.,4.75,2.75));
#44637=CARTESIAN_POINT('Origin',(62.6014464469636,0.75,13.3063482123366));
#44638=CARTESIAN_POINT('Origin',(70.3840822607801,-4.95,10.3600658447588));
#44639=CARTESIAN_POINT('',(56.6900158505068,-0.75,7.44930217331019));
#44640=CARTESIAN_POINT('Origin',(62.6014464469636,-0.75,13.3063482123366));
#44641=CARTESIAN_POINT('Origin',(58.4669092891264,0.75,26.0311451568513));
#44642=CARTESIAN_POINT('Origin',(53.9024059794693,-4.95,19.0730340959289));
#44643=CARTESIAN_POINT('',(53.9024059794693,-0.75,19.0730340959289));
#44644=CARTESIAN_POINT('',(53.9024059794693,-4.95,19.0730340959289));
#44645=CARTESIAN_POINT('',(50.2417761917871,-0.75,27.2949432147124));
#44646=CARTESIAN_POINT('',(50.2417761917871,-0.75,27.2949432147124));
#44647=CARTESIAN_POINT('',(50.2417761917871,-4.95,27.2949432147124));
#44648=CARTESIAN_POINT('Origin',(66.6920423864657,-4.95,24.7673470989902));
#44649=CARTESIAN_POINT('',(53.9024059794693,-0.75,19.0730340959289));
#44650=CARTESIAN_POINT('Origin',(50.2417761917871,-4.95,27.2949432147124));
#44651=CARTESIAN_POINT('',(63.0314125987835,-0.75,32.9892562177736));
#44652=CARTESIAN_POINT('Origin',(58.4669092891264,-0.75,26.0311451568513));
#44653=CARTESIAN_POINT('Origin',(51.7770876399966,0.75,37.6182561467183));
#44654=CARTESIAN_POINT('Origin',(48.7590023146881,-4.95,29.8631829059837));
#44655=CARTESIAN_POINT('',(48.7590023146881,-0.75,29.8631829059837));
#44656=CARTESIAN_POINT('',(48.7590023146881,-4.95,29.8631829059837));
#44657=CARTESIAN_POINT('',(43.4689350440559,-0.75,37.1443358553582));
#44658=CARTESIAN_POINT('',(43.4689350440559,-0.75,37.1443358553582));
#44659=CARTESIAN_POINT('',(43.4689350440559,-4.95,37.1443358553582));
#44660=CARTESIAN_POINT('Origin',(60.0852402359374,-4.95,38.0921764380783));
#44661=CARTESIAN_POINT('',(48.7590023146881,-0.75,29.8631829059837));
#44662=CARTESIAN_POINT('Origin',(43.4689350440559,-4.95,37.1443358553582));
#44663=CARTESIAN_POINT('',(54.7951729653051,-0.75,45.3733293874529));
#44664=CARTESIAN_POINT('Origin',(51.7770876399966,-0.75,37.6182561467183));
#44665=CARTESIAN_POINT('Origin',(42.8243588069669,0.75,47.5612688305533));
#44666=CARTESIAN_POINT('Origin',(50.8524247661272,-4.95,49.7521948802802));
#44667=CARTESIAN_POINT('',(41.4845962771032,-0.75,39.3481673235966));
#44668=CARTESIAN_POINT('Origin',(42.8243588069669,-0.75,47.5612688305533));
#44669=CARTESIAN_POINT('Origin',(32.,0.75,55.4256258422041));
#44670=CARTESIAN_POINT('Origin',(32.3971143170299,-4.95,47.113448015713));
#44671=CARTESIAN_POINT('',(32.3971143170299,-0.75,47.113448015713));
#44672=CARTESIAN_POINT('',(32.3971143170299,-4.95,47.113448015713));
#44673=CARTESIAN_POINT('',(24.60288568297,-0.75,51.613448015713));
#44674=CARTESIAN_POINT('',(24.60288568297,-0.75,51.613448015713));
#44675=CARTESIAN_POINT('',(24.60288568297,-4.95,51.613448015713));
#44676=CARTESIAN_POINT('Origin',(39.3971143170299,-4.95,59.2378036686952));
#44677=CARTESIAN_POINT('',(32.3971143170299,-0.75,47.113448015713));
#44678=CARTESIAN_POINT('Origin',(24.60288568297,-4.95,51.613448015713));
#44679=CARTESIAN_POINT('',(31.60288568297,-0.75,63.7378036686952));
#44680=CARTESIAN_POINT('Origin',(32.,-0.75,55.4256258422041));
#44681=CARTESIAN_POINT('Origin',(19.7770876399966,0.75,60.8676170428898));
#44682=CARTESIAN_POINT('Origin',(26.2199609239494,-4.95,66.1344361822686));
#44683=CARTESIAN_POINT('',(21.8937230027002,-0.75,52.8196449541365));
#44684=CARTESIAN_POINT('Origin',(19.7770876399966,-0.75,60.8676170428898));
#44685=CARTESIAN_POINT('Origin',(6.68982164912979,0.75,63.6494013035695));
#44686=CARTESIAN_POINT('Origin',(10.4334709354135,-4.95,56.2173699512871));
#44687=CARTESIAN_POINT('',(10.4334709354135,-0.75,56.2173699512871));
#44688=CARTESIAN_POINT('',(10.4334709354135,-4.95,56.2173699512871));
#44689=CARTESIAN_POINT('',(1.48277387709899,-0.75,57.158126120696));
#44690=CARTESIAN_POINT('',(1.48277387709899,-0.75,57.158126120696));
#44691=CARTESIAN_POINT('',(1.48277387709899,-4.95,57.158126120696));
#44692=CARTESIAN_POINT('Origin',(11.8968694211606,-4.95,70.140676486443));
#44693=CARTESIAN_POINT('',(10.4334709354135,-0.75,56.2173699512871));
#44694=CARTESIAN_POINT('Origin',(1.48277387709899,-4.95,57.158126120696));
#44695=CARTESIAN_POINT('',(2.94617236284613,-0.75,71.0814326558519));
#44696=CARTESIAN_POINT('Origin',(6.68982164912979,-0.75,63.6494013035695));
#44697=CARTESIAN_POINT('Origin',(-6.68982164912987,0.75,63.6494013035695));
#44698=CARTESIAN_POINT('Origin',(-2.94617236284622,-4.95,71.0814326558519));
#44699=CARTESIAN_POINT('',(-1.48277387709906,-0.75,57.158126120696));
#44700=CARTESIAN_POINT('Origin',(-6.68982164912987,-0.75,63.6494013035695));
#44701=CARTESIAN_POINT('Origin',(-19.7770876399966,0.75,60.8676170428898));
#44702=CARTESIAN_POINT('Origin',(-13.3342143560438,-4.95,55.600797903511));
#44703=CARTESIAN_POINT('',(-13.3342143560438,-0.75,55.600797903511));
#44704=CARTESIAN_POINT('',(-13.3342143560438,-4.95,55.600797903511));
#44705=CARTESIAN_POINT('',(-21.8937230027002,-0.75,52.8196449541365));
#44706=CARTESIAN_POINT('',(-21.8937230027002,-0.75,52.8196449541365));
#44707=CARTESIAN_POINT('',(-21.8937230027002,-4.95,52.8196449541365));
#44708=CARTESIAN_POINT('Origin',(-17.6604522772931,-4.95,68.9155891316432));
#44709=CARTESIAN_POINT('',(-13.3342143560438,-0.75,55.600797903511));
#44710=CARTESIAN_POINT('Origin',(-21.8937230027002,-4.95,52.8196449541365));
#44711=CARTESIAN_POINT('',(-26.2199609239495,-0.75,66.1344361822686));
#44712=CARTESIAN_POINT('Origin',(-19.7770876399966,-0.75,60.8676170428898));
#44713=CARTESIAN_POINT('Origin',(-32.,0.75,55.4256258422041));
#44714=CARTESIAN_POINT('Origin',(-24.6028856829701,-4.95,51.613448015713));
#44715=CARTESIAN_POINT('',(-24.6028856829701,-0.75,51.613448015713));
#44716=CARTESIAN_POINT('',(-24.6028856829701,-4.95,51.613448015713));
#44717=CARTESIAN_POINT('',(-32.39711431703,-0.75,47.113448015713));
#44718=CARTESIAN_POINT('',(-32.39711431703,-0.75,47.113448015713));
#44719=CARTESIAN_POINT('',(-32.39711431703,-4.95,47.113448015713));
#44720=CARTESIAN_POINT('Origin',(-31.6028856829701,-4.95,63.7378036686951));
#44721=CARTESIAN_POINT('',(-24.6028856829701,-0.75,51.613448015713));
#44722=CARTESIAN_POINT('Origin',(-32.39711431703,-4.95,47.113448015713));
#44723=CARTESIAN_POINT('',(-39.39711431703,-0.75,59.2378036686951));
#44724=CARTESIAN_POINT('Origin',(-32.,-0.75,55.4256258422041));
#44725=CARTESIAN_POINT('Origin',(-42.8243588069669,0.75,47.5612688305532));
#44726=CARTESIAN_POINT('Origin',(-44.1641213368307,-4.95,55.7743703375098));
#44727=CARTESIAN_POINT('',(-34.7962928478067,-0.75,45.3703427808263));
#44728=CARTESIAN_POINT('Origin',(-42.8243588069669,-0.75,47.5612688305532));
#44729=CARTESIAN_POINT('Origin',(-51.7770876399966,0.75,37.6182561467183));
#44730=CARTESIAN_POINT('Origin',(-43.4689350440559,-4.95,37.1443358553582));
#44731=CARTESIAN_POINT('',(-43.4689350440559,-0.75,37.1443358553582));
#44732=CARTESIAN_POINT('',(-43.4689350440559,-4.95,37.1443358553582));
#44733=CARTESIAN_POINT('',(-48.7590023146881,-0.75,29.8631829059837));
#44734=CARTESIAN_POINT('',(-48.7590023146881,-0.75,29.8631829059837));
#44735=CARTESIAN_POINT('',(-48.7590023146881,-4.95,29.8631829059837));
#44736=CARTESIAN_POINT('Origin',(-54.7951729653051,-4.95,45.3733293874529));
#44737=CARTESIAN_POINT('',(-43.4689350440559,-0.75,37.1443358553582));
#44738=CARTESIAN_POINT('Origin',(-48.7590023146881,-4.95,29.8631829059837));
#44739=CARTESIAN_POINT('',(-60.0852402359374,-0.75,38.0921764380783));
#44740=CARTESIAN_POINT('Origin',(-51.7770876399966,-0.75,37.6182561467183));
#44741=CARTESIAN_POINT('Origin',(-58.4669092891265,0.75,26.0311451568512));
#44742=CARTESIAN_POINT('Origin',(-63.0314125987836,-4.95,32.9892562177735));
#44743=CARTESIAN_POINT('',(-50.2417761917872,-0.75,27.2949432147123));
#44744=CARTESIAN_POINT('Origin',(-58.4669092891265,-0.75,26.0311451568512));
#44745=CARTESIAN_POINT('Origin',(-62.6014464469636,0.75,13.3063482123366));
#44746=CARTESIAN_POINT('Origin',(-54.818810633147,-4.95,16.2526305799144));
#44747=CARTESIAN_POINT('',(-54.818810633147,-0.75,16.2526305799144));
#44748=CARTESIAN_POINT('',(-54.818810633147,-4.95,16.2526305799144));
#44749=CARTESIAN_POINT('',(-56.6900158505068,-0.75,7.44930217331014));
#44750=CARTESIAN_POINT('',(-56.6900158505068,-0.75,7.44930217331014));
#44751=CARTESIAN_POINT('',(-56.6900158505068,-4.95,7.44930217331014));
#44752=CARTESIAN_POINT('Origin',(-68.5128770434203,-4.95,19.163394251363));
#44753=CARTESIAN_POINT('',(-54.818810633147,-0.75,16.2526305799144));
#44754=CARTESIAN_POINT('Origin',(-56.6900158505068,-4.95,7.44930217331014));
#44755=CARTESIAN_POINT('',(-70.3840822607801,-0.75,10.3600658447588));
#44756=CARTESIAN_POINT('Origin',(-62.6014464469636,-0.75,13.3063482123366));
#44757=CARTESIAN_POINT('Origin',(-64.,0.75,-7.83773951454306E-15));
#44758=CARTESIAN_POINT('Origin',(-71.,-4.95,4.49999999999999));
#44759=CARTESIAN_POINT('',(-57.,-0.75,4.49999999999999));
#44760=CARTESIAN_POINT('Origin',(-64.,-0.75,-7.83773951454306E-15));
#44761=CARTESIAN_POINT('Origin',(-62.6014464469636,0.75,-13.3063482123366));
#44762=CARTESIAN_POINT('Origin',(-56.6900158505068,-4.95,-7.44930217331018));
#44763=CARTESIAN_POINT('',(-56.6900158505068,-0.75,-7.44930217331018));
#44764=CARTESIAN_POINT('',(-56.6900158505068,-4.95,-7.44930217331018));
#44765=CARTESIAN_POINT('',(-54.818810633147,-0.75,-16.2526305799144));
#44766=CARTESIAN_POINT('',(-54.818810633147,-0.75,-16.2526305799144));
#44767=CARTESIAN_POINT('',(-54.818810633147,-4.95,-16.2526305799144));
#44768=CARTESIAN_POINT('Origin',(-70.3840822607801,-4.95,-10.3600658447588));
#44769=CARTESIAN_POINT('',(-56.6900158505068,-0.75,-7.44930217331018));
#44770=CARTESIAN_POINT('Origin',(-54.818810633147,-4.95,-16.2526305799144));
#44771=CARTESIAN_POINT('',(-68.5128770434203,-0.75,-19.1633942513631));
#44772=CARTESIAN_POINT('Origin',(-62.6014464469636,-0.75,-13.3063482123366));
#44773=CARTESIAN_POINT('Origin',(-58.4669092891264,0.75,-26.0311451568512));
#44774=CARTESIAN_POINT('Origin',(-66.6920423864657,-4.95,-24.7673470989901));
#44775=CARTESIAN_POINT('',(-53.9024059794693,-0.75,-19.0730340959289));
#44776=CARTESIAN_POINT('Origin',(-58.4669092891264,-0.75,-26.0311451568512));
#44777=CARTESIAN_POINT('Origin',(-51.7770876399966,0.75,-37.6182561467183));
#44778=CARTESIAN_POINT('Origin',(-48.7590023146881,-4.95,-29.8631829059837));
#44779=CARTESIAN_POINT('',(-48.7590023146881,-0.75,-29.8631829059837));
#44780=CARTESIAN_POINT('',(-48.7590023146881,-4.95,-29.8631829059837));
#44781=CARTESIAN_POINT('',(-43.4689350440559,-0.75,-37.1443358553582));
#44782=CARTESIAN_POINT('',(-43.4689350440559,-0.75,-37.1443358553582));
#44783=CARTESIAN_POINT('',(-43.4689350440559,-4.95,-37.1443358553582));
#44784=CARTESIAN_POINT('Origin',(-60.0852402359374,-4.95,-38.0921764380783));
#44785=CARTESIAN_POINT('',(-48.7590023146881,-0.75,-29.8631829059837));
#44786=CARTESIAN_POINT('Origin',(-43.4689350440559,-4.95,-37.1443358553582));
#44787=CARTESIAN_POINT('',(-54.7951729653051,-0.75,-45.3733293874529));
#44788=CARTESIAN_POINT('Origin',(-51.7770876399966,-0.75,-37.6182561467183));
#44789=CARTESIAN_POINT('Origin',(-42.8243588069669,0.75,-47.5612688305532));
#44790=CARTESIAN_POINT('Origin',(-50.8524247661272,-4.95,-49.7521948802801));
#44791=CARTESIAN_POINT('',(-41.4845962771032,-0.75,-39.3481673235966));
#44792=CARTESIAN_POINT('Origin',(-42.8243588069669,-0.75,-47.5612688305532));
#44793=CARTESIAN_POINT('Origin',(-32.39711431703,4.95,-47.113448015713));
#44794=CARTESIAN_POINT('',(-32.39711431703,0.75,-47.113448015713));
#44795=CARTESIAN_POINT('Origin',(-32.,0.75,-55.4256258422041));
#44796=CARTESIAN_POINT('Origin',(-32.39711431703,-4.95,-47.113448015713));
#44797=CARTESIAN_POINT('',(-32.39711431703,-0.75,-47.113448015713));
#44798=CARTESIAN_POINT('',(-32.39711431703,-4.95,-47.113448015713));
#44799=CARTESIAN_POINT('',(-24.60288568297,-0.75,-51.613448015713));
#44800=CARTESIAN_POINT('',(-24.60288568297,-0.75,-51.613448015713));
#44801=CARTESIAN_POINT('',(-24.60288568297,-4.95,-51.613448015713));
#44802=CARTESIAN_POINT('Origin',(-39.39711431703,-4.95,-59.2378036686952));
#44803=CARTESIAN_POINT('',(-32.39711431703,-0.75,-47.113448015713));
#44804=CARTESIAN_POINT('Origin',(-24.60288568297,-4.95,-51.613448015713));
#44805=CARTESIAN_POINT('',(-31.60288568297,-0.75,-63.7378036686952));
#44806=CARTESIAN_POINT('Origin',(-32.,-0.75,-55.4256258422041));
#44807=CARTESIAN_POINT('Origin',(-19.7770876399966,0.75,-60.8676170428898));
#44808=CARTESIAN_POINT('Origin',(-26.2199609239495,-4.95,-66.1344361822686));
#44809=CARTESIAN_POINT('',(-21.8937230027002,-0.75,-52.8196449541365));
#44810=CARTESIAN_POINT('Origin',(-19.7770876399966,-0.75,-60.8676170428898));
#44811=CARTESIAN_POINT('Origin',(-6.68982164912981,0.75,-63.6494013035695));
#44812=CARTESIAN_POINT('Origin',(-10.4334709354135,-4.95,-56.2173699512871));
#44813=CARTESIAN_POINT('',(-10.4334709354135,-0.75,-56.2173699512871));
#44814=CARTESIAN_POINT('',(-10.4334709354135,-4.95,-56.2173699512871));
#44815=CARTESIAN_POINT('',(-1.48277387709901,-0.75,-57.158126120696));
#44816=CARTESIAN_POINT('',(-1.48277387709901,-0.75,-57.158126120696));
#44817=CARTESIAN_POINT('',(-1.48277387709901,-4.95,-57.158126120696));
#44818=CARTESIAN_POINT('Origin',(-11.8968694211606,-4.95,-70.140676486443));
#44819=CARTESIAN_POINT('',(-10.4334709354135,-0.75,-56.2173699512871));
#44820=CARTESIAN_POINT('Origin',(-1.48277387709901,-4.95,-57.158126120696));
#44821=CARTESIAN_POINT('',(-2.94617236284616,-0.75,-71.0814326558519));
#44822=CARTESIAN_POINT('Origin',(-6.68982164912981,-0.75,-63.6494013035695));
#44823=CARTESIAN_POINT('Origin',(6.68982164912984,0.75,-63.6494013035695));
#44824=CARTESIAN_POINT('Origin',(1.48277387709903,-4.95,-57.158126120696));
#44825=CARTESIAN_POINT('',(1.48277387709903,-0.75,-57.158126120696));
#44826=CARTESIAN_POINT('',(1.48277387709903,-4.95,-57.158126120696));
#44827=CARTESIAN_POINT('',(10.4334709354135,-0.75,-56.2173699512871));
#44828=CARTESIAN_POINT('',(10.4334709354135,-0.75,-56.2173699512871));
#44829=CARTESIAN_POINT('',(10.4334709354135,-4.95,-56.2173699512871));
#44830=CARTESIAN_POINT('Origin',(2.94617236284618,-4.95,-71.0814326558518));
#44831=CARTESIAN_POINT('',(1.48277387709903,-0.75,-57.158126120696));
#44832=CARTESIAN_POINT('Origin',(10.4334709354135,-4.95,-56.2173699512871));
#44833=CARTESIAN_POINT('',(11.8968694211606,-0.75,-70.140676486443));
#44834=CARTESIAN_POINT('Origin',(6.68982164912984,-0.75,-63.6494013035695));
#44835=CARTESIAN_POINT('Origin',(19.7770876399966,0.75,-60.8676170428898));
#44836=CARTESIAN_POINT('',(26.2199609239495,0.75,-66.1344361822686));
#44837=CARTESIAN_POINT('Origin',(26.2199609239495,4.95,-66.1344361822686));
#44838=CARTESIAN_POINT('Origin',(17.6604522772931,-4.95,-68.9155891316432));
#44839=CARTESIAN_POINT('',(13.3342143560438,-0.75,-55.600797903511));
#44840=CARTESIAN_POINT('Origin',(19.7770876399966,-0.75,-60.8676170428898));
#44841=CARTESIAN_POINT('Origin',(24.60288568297,4.95,-51.613448015713));
#44842=CARTESIAN_POINT('',(24.60288568297,0.75,-51.613448015713));
#44843=CARTESIAN_POINT('',(24.60288568297,4.95,-51.613448015713));
#44844=CARTESIAN_POINT('',(24.60288568297,0.75,-51.613448015713));
#44845=CARTESIAN_POINT('Origin',(32.,0.75,-55.4256258422041));
#44846=CARTESIAN_POINT('',(32.39711431703,0.75,-47.113448015713));
#44847=CARTESIAN_POINT('',(32.39711431703,0.75,-47.113448015713));
#44848=CARTESIAN_POINT('',(39.39711431703,0.75,-59.2378036686951));
#44849=CARTESIAN_POINT('Origin',(32.39711431703,4.95,-47.113448015713));
#44850=CARTESIAN_POINT('',(32.39711431703,4.95,-47.113448015713));
#44851=CARTESIAN_POINT('Origin',(39.39711431703,4.95,-59.2378036686951));
#44852=CARTESIAN_POINT('Origin',(24.60288568297,-4.95,-51.613448015713));
#44853=CARTESIAN_POINT('',(24.60288568297,-0.75,-51.613448015713));
#44854=CARTESIAN_POINT('',(24.60288568297,-4.95,-51.613448015713));
#44855=CARTESIAN_POINT('',(32.39711431703,-0.75,-47.113448015713));
#44856=CARTESIAN_POINT('',(32.39711431703,-0.75,-47.113448015713));
#44857=CARTESIAN_POINT('',(32.39711431703,-4.95,-47.113448015713));
#44858=CARTESIAN_POINT('Origin',(31.60288568297,-4.95,-63.7378036686951));
#44859=CARTESIAN_POINT('',(24.60288568297,-0.75,-51.613448015713));
#44860=CARTESIAN_POINT('Origin',(32.39711431703,-4.95,-47.113448015713));
#44861=CARTESIAN_POINT('',(39.39711431703,-0.75,-59.2378036686951));
#44862=CARTESIAN_POINT('Origin',(32.,-0.75,-55.4256258422041));
#44863=CARTESIAN_POINT('Origin',(34.7962928478066,4.95,-45.3703427808263));
#44864=CARTESIAN_POINT('',(34.7962928478066,0.75,-45.3703427808263));
#44865=CARTESIAN_POINT('',(34.7962928478066,4.95,-45.3703427808263));
#44866=CARTESIAN_POINT('',(34.7962928478066,0.75,-45.3703427808263));
#44867=CARTESIAN_POINT('Origin',(42.8243588069669,0.75,-47.5612688305532));
#44868=CARTESIAN_POINT('',(41.4845962771032,0.75,-39.3481673235966));
#44869=CARTESIAN_POINT('',(41.4845962771032,0.75,-39.3481673235966));
#44870=CARTESIAN_POINT('',(50.8524247661272,0.75,-49.7521948802801));
#44871=CARTESIAN_POINT('Origin',(41.4845962771032,4.95,-39.3481673235966));
#44872=CARTESIAN_POINT('',(41.4845962771032,4.95,-39.3481673235966));
#44873=CARTESIAN_POINT('Origin',(50.8524247661272,4.95,-49.7521948802801));
#44874=CARTESIAN_POINT('Origin',(44.1641213368307,-4.95,-55.7743703375099));
#44875=CARTESIAN_POINT('',(34.7962928478066,-0.75,-45.3703427808263));
#44876=CARTESIAN_POINT('Origin',(42.8243588069669,-0.75,-47.5612688305532));
#44877=CARTESIAN_POINT('Origin',(43.4689350440559,4.95,-37.1443358553582));
#44878=CARTESIAN_POINT('',(43.4689350440559,0.75,-37.1443358553582));
#44879=CARTESIAN_POINT('',(43.4689350440559,4.95,-37.1443358553582));
#44880=CARTESIAN_POINT('',(43.4689350440559,0.75,-37.1443358553582));
#44881=CARTESIAN_POINT('Origin',(51.7770876399966,0.75,-37.6182561467183));
#44882=CARTESIAN_POINT('',(48.7590023146881,0.75,-29.8631829059837));
#44883=CARTESIAN_POINT('',(48.7590023146881,0.75,-29.8631829059837));
#44884=CARTESIAN_POINT('',(60.0852402359374,0.75,-38.0921764380783));
#44885=CARTESIAN_POINT('Origin',(48.7590023146881,4.95,-29.8631829059837));
#44886=CARTESIAN_POINT('',(48.7590023146881,4.95,-29.8631829059837));
#44887=CARTESIAN_POINT('Origin',(60.0852402359374,4.95,-38.0921764380783));
#44888=CARTESIAN_POINT('Origin',(43.4689350440559,-4.95,-37.1443358553582));
#44889=CARTESIAN_POINT('',(43.4689350440559,-0.75,-37.1443358553582));
#44890=CARTESIAN_POINT('',(43.4689350440559,-4.95,-37.1443358553582));
#44891=CARTESIAN_POINT('',(48.7590023146881,-0.75,-29.8631829059837));
#44892=CARTESIAN_POINT('',(48.7590023146881,-0.75,-29.8631829059837));
#44893=CARTESIAN_POINT('',(48.7590023146881,-4.95,-29.8631829059837));
#44894=CARTESIAN_POINT('Origin',(54.7951729653051,-4.95,-45.3733293874529));
#44895=CARTESIAN_POINT('',(43.4689350440559,-0.75,-37.1443358553582));
#44896=CARTESIAN_POINT('Origin',(48.7590023146881,-4.95,-29.8631829059837));
#44897=CARTESIAN_POINT('',(60.0852402359374,-0.75,-38.0921764380783));
#44898=CARTESIAN_POINT('Origin',(51.7770876399966,-0.75,-37.6182561467183));
#44899=CARTESIAN_POINT('Origin',(50.2417761917872,4.95,-27.2949432147123));
#44900=CARTESIAN_POINT('',(50.2417761917872,0.75,-27.2949432147123));
#44901=CARTESIAN_POINT('',(50.2417761917872,4.95,-27.2949432147123));
#44902=CARTESIAN_POINT('',(50.2417761917872,0.75,-27.2949432147123));
#44903=CARTESIAN_POINT('Origin',(58.4669092891265,0.75,-26.0311451568512));
#44904=CARTESIAN_POINT('',(53.9024059794694,0.75,-19.0730340959289));
#44905=CARTESIAN_POINT('',(53.9024059794694,0.75,-19.0730340959289));
#44906=CARTESIAN_POINT('',(66.6920423864658,0.75,-24.7673470989901));
#44907=CARTESIAN_POINT('Origin',(53.9024059794694,4.95,-19.0730340959289));
#44908=CARTESIAN_POINT('',(53.9024059794694,4.95,-19.0730340959289));
#44909=CARTESIAN_POINT('Origin',(66.6920423864658,4.95,-24.7673470989901));
#44910=CARTESIAN_POINT('Origin',(63.0314125987836,-4.95,-32.9892562177735));
#44911=CARTESIAN_POINT('',(50.2417761917872,-0.75,-27.2949432147123));
#44912=CARTESIAN_POINT('Origin',(58.4669092891265,-0.75,-26.0311451568512));
#44913=CARTESIAN_POINT('Origin',(54.818810633147,4.95,-16.2526305799144));
#44914=CARTESIAN_POINT('',(54.818810633147,0.75,-16.2526305799144));
#44915=CARTESIAN_POINT('',(54.818810633147,4.95,-16.2526305799144));
#44916=CARTESIAN_POINT('',(54.818810633147,0.75,-16.2526305799144));
#44917=CARTESIAN_POINT('Origin',(62.6014464469636,0.75,-13.3063482123366));
#44918=CARTESIAN_POINT('',(56.6900158505068,0.75,-7.44930217331016));
#44919=CARTESIAN_POINT('',(56.6900158505068,0.75,-7.44930217331016));
#44920=CARTESIAN_POINT('',(70.3840822607801,0.75,-10.3600658447588));
#44921=CARTESIAN_POINT('Origin',(56.6900158505068,4.95,-7.44930217331016));
#44922=CARTESIAN_POINT('',(56.6900158505068,4.95,-7.44930217331016));
#44923=CARTESIAN_POINT('Origin',(70.3840822607801,4.95,-10.3600658447588));
#44924=CARTESIAN_POINT('Origin',(54.818810633147,-4.95,-16.2526305799144));
#44925=CARTESIAN_POINT('',(54.818810633147,-0.75,-16.2526305799144));
#44926=CARTESIAN_POINT('',(54.818810633147,-4.95,-16.2526305799144));
#44927=CARTESIAN_POINT('',(56.6900158505068,-0.75,-7.44930217331016));
#44928=CARTESIAN_POINT('',(56.6900158505068,-0.75,-7.44930217331016));
#44929=CARTESIAN_POINT('',(56.6900158505068,-4.95,-7.44930217331016));
#44930=CARTESIAN_POINT('Origin',(68.5128770434203,-4.95,-19.163394251363));
#44931=CARTESIAN_POINT('',(54.818810633147,-0.75,-16.2526305799144));
#44932=CARTESIAN_POINT('Origin',(56.6900158505068,-4.95,-7.44930217331016));
#44933=CARTESIAN_POINT('',(70.3840822607801,-0.75,-10.3600658447588));
#44934=CARTESIAN_POINT('Origin',(62.6014464469636,-0.75,-13.3063482123366));
#44935=CARTESIAN_POINT('Origin',(57.,4.95,-4.5));
#44936=CARTESIAN_POINT('',(57.,0.75,-4.5));
#44937=CARTESIAN_POINT('',(57.,4.95,-4.5));
#44938=CARTESIAN_POINT('',(57.,0.75,-4.5));
#44939=CARTESIAN_POINT('Origin',(64.,0.75,0.));
#44940=CARTESIAN_POINT('',(57.,0.75,4.5));
#44941=CARTESIAN_POINT('',(57.,0.75,4.5));
#44942=CARTESIAN_POINT('',(71.,0.75,4.5));
#44943=CARTESIAN_POINT('Origin',(57.,4.95,4.5));
#44944=CARTESIAN_POINT('',(57.,4.95,4.5));
#44945=CARTESIAN_POINT('Origin',(71.,4.95,4.5));
#44946=CARTESIAN_POINT('Origin',(64.,-0.75,0.));
#44947=CARTESIAN_POINT('',(57.,-0.75,4.5));
#44948=CARTESIAN_POINT('',(71.,-0.75,4.5));
#44949=CARTESIAN_POINT('',(57.,-0.75,-4.5));
#44950=CARTESIAN_POINT('',(57.,-0.75,4.5));
#44951=CARTESIAN_POINT('',(57.,-0.75,-4.5));
#44952=CARTESIAN_POINT('Origin',(71.,-4.95,-4.5));
#44953=CARTESIAN_POINT('',(57.,-4.95,-4.5));
#44954=CARTESIAN_POINT('Origin',(57.,-4.95,-4.5));
#44955=CARTESIAN_POINT('',(57.,-4.95,4.5));
#44956=CARTESIAN_POINT('Origin',(57.,-4.95,4.5));
#44957=CARTESIAN_POINT('Origin',(0.,0.,0.));
#44958=CARTESIAN_POINT('',(0.,0.,0.));
#44959=CARTESIAN_POINT('Origin',(165.,-3.,10.));
#44960=CARTESIAN_POINT('',(165.,-3.,9.53939201416946));
#44961=CARTESIAN_POINT('',(165.,3.,9.53939201416946));
#44962=CARTESIAN_POINT('Origin',(165.,0.,0.));
#44963=CARTESIAN_POINT('',(165.,-3.,6.5));
#44964=CARTESIAN_POINT('',(165.,-3.,10.));
#44965=CARTESIAN_POINT('',(165.,3.,6.5));
#44966=CARTESIAN_POINT('',(165.,3.,6.5));
#44967=CARTESIAN_POINT('',(165.,3.,10.));
#44968=CARTESIAN_POINT('Origin',(165.,3.,10.));
#44969=CARTESIAN_POINT('',(190.,3.,9.53939201416946));
#44970=CARTESIAN_POINT('',(167.25,3.,9.53939201416946));
#44971=CARTESIAN_POINT('',(190.,3.,6.5));
#44972=CARTESIAN_POINT('',(190.,3.,6.5));
#44973=CARTESIAN_POINT('',(190.,3.,10.));
#44974=CARTESIAN_POINT('Origin',(190.,-3.,10.));
#44975=CARTESIAN_POINT('',(190.,-3.,9.53939201416946));
#44976=CARTESIAN_POINT('',(167.25,-3.,9.53939201416946));
#44977=CARTESIAN_POINT('',(190.,-3.,6.5));
#44978=CARTESIAN_POINT('',(190.,-3.,10.));
#44979=CARTESIAN_POINT('',(165.,-3.,6.5));
#44980=CARTESIAN_POINT('Origin',(190.,3.,10.));
#44981=CARTESIAN_POINT('Origin',(190.,0.,0.));
#44982=CARTESIAN_POINT('',(190.,-3.,6.5));
#44983=CARTESIAN_POINT('Origin',(177.5,0.,6.5));
#44984=CARTESIAN_POINT('Origin',(0.,-11.,0.));
#44985=CARTESIAN_POINT('',(1.38777878078145E-16,-9.67987086690727,2.51));
#44986=CARTESIAN_POINT('',(2.51,-10.,-6.81712338612749E-16));
#44987=CARTESIAN_POINT('Ctrl Pts',(-6.93889390390723E-17,-9.67987086690727,
2.51));
#44988=CARTESIAN_POINT('Ctrl Pts',(0.316647397714408,-9.67987086690727,
2.51));
#44989=CARTESIAN_POINT('Ctrl Pts',(0.653424667393654,-9.69702654534655,
2.4464396819459));
#44990=CARTESIAN_POINT('Ctrl Pts',(1.27140541887387,-9.75816738483577,2.18987665098482));
#44991=CARTESIAN_POINT('Ctrl Pts',(1.55273320805174,-9.80118127300772,1.99694283350472));
#44992=CARTESIAN_POINT('Ctrl Pts',(1.99691126398784,-9.8812874714592,1.55276477756863));
#44993=CARTESIAN_POINT('Ctrl Pts',(2.18986969302056,-9.92370211108617,1.27142384596148));
#44994=CARTESIAN_POINT('Ctrl Pts',(2.44645069525432,-9.98345908137755,0.653396472215422));
#44995=CARTESIAN_POINT('Ctrl Pts',(2.51,-10.,0.316602390110811));
#44996=CARTESIAN_POINT('Ctrl Pts',(2.51,-10.,-6.93889390390723E-17));
#44997=CARTESIAN_POINT('',(-2.51,-10.,3.07386346585986E-16));
#44998=CARTESIAN_POINT('Ctrl Pts',(-2.51,-10.,-4.16333634234434E-16));
#44999=CARTESIAN_POINT('Ctrl Pts',(-2.51,-10.,0.31660239011081));
#45000=CARTESIAN_POINT('Ctrl Pts',(-2.44645069525432,-9.98345908137755,
0.65339647221542));
#45001=CARTESIAN_POINT('Ctrl Pts',(-2.18986969302057,-9.92370211108617,
1.27142384596147));
#45002=CARTESIAN_POINT('Ctrl Pts',(-1.99691126398784,-9.8812874714592,1.55276477756863));
#45003=CARTESIAN_POINT('Ctrl Pts',(-1.55273320805175,-9.80118127300772,
1.99694283350472));
#45004=CARTESIAN_POINT('Ctrl Pts',(-1.27140541887387,-9.75816738483577,
2.18987665098481));
#45005=CARTESIAN_POINT('Ctrl Pts',(-0.653424667393656,-9.69702654534655,
2.4464396819459));
#45006=CARTESIAN_POINT('Ctrl Pts',(-0.316647397714409,-9.67987086690727,
2.51));
#45007=CARTESIAN_POINT('Ctrl Pts',(0.,-9.67987086690727,2.51));
#45008=CARTESIAN_POINT('',(-2.51,10.,3.07386346585986E-16));
#45009=CARTESIAN_POINT('',(-2.51,-11.,3.07386346585986E-16));
#45010=CARTESIAN_POINT('',(-6.93889390390723E-17,9.67987086690727,2.51));
#45011=CARTESIAN_POINT('Ctrl Pts',(-6.93889390390723E-17,9.67987086690727,
2.51));
#45012=CARTESIAN_POINT('Ctrl Pts',(-0.316647397714408,9.67987086690727,
2.51));
#45013=CARTESIAN_POINT('Ctrl Pts',(-0.653424667393654,9.69702654534655,
2.4464396819459));
#45014=CARTESIAN_POINT('Ctrl Pts',(-1.27140541887387,9.75816738483577,2.18987665098482));
#45015=CARTESIAN_POINT('Ctrl Pts',(-1.55273320805175,9.80118127300772,1.99694283350472));
#45016=CARTESIAN_POINT('Ctrl Pts',(-1.99691126398784,9.8812874714592,1.55276477756863));
#45017=CARTESIAN_POINT('Ctrl Pts',(-2.18986969302057,9.92370211108617,1.27142384596147));
#45018=CARTESIAN_POINT('Ctrl Pts',(-2.44645069525432,9.98345908137755,0.653396472215421));
#45019=CARTESIAN_POINT('Ctrl Pts',(-2.51,10.,0.31660239011081));
#45020=CARTESIAN_POINT('Ctrl Pts',(-2.51,10.,-3.46944695195361E-16));
#45021=CARTESIAN_POINT('Ctrl Pts',(-2.51,10.,-2.77555756156289E-16));
#45022=CARTESIAN_POINT('Ctrl Pts',(-2.51,10.,-0.316602390110811));
#45023=CARTESIAN_POINT('Ctrl Pts',(-2.44645069525432,9.98345908137755,-0.653396472215422));
#45024=CARTESIAN_POINT('Ctrl Pts',(-2.18986969302056,9.92370211108617,-1.27142384596148));
#45025=CARTESIAN_POINT('Ctrl Pts',(-1.99691126398784,9.8812874714592,-1.55276477756863));
#45026=CARTESIAN_POINT('Ctrl Pts',(-1.55273320805174,9.80118127300772,-1.99694283350472));
#45027=CARTESIAN_POINT('Ctrl Pts',(-1.27140541887387,9.75816738483577,-2.18987665098482));
#45028=CARTESIAN_POINT('Ctrl Pts',(-0.653424667393654,9.69702654534655,
-2.4464396819459));
#45029=CARTESIAN_POINT('Ctrl Pts',(-0.316647397714408,9.67987086690727,
-2.51));
#45030=CARTESIAN_POINT('Ctrl Pts',(0.316647397714408,9.67987086690727,-2.51));
#45031=CARTESIAN_POINT('Ctrl Pts',(0.653424667393654,9.69702654534655,-2.4464396819459));
#45032=CARTESIAN_POINT('Ctrl Pts',(1.27140541887387,9.75816738483577,-2.18987665098482));
#45033=CARTESIAN_POINT('Ctrl Pts',(1.55273320805174,9.80118127300772,-1.99694283350472));
#45034=CARTESIAN_POINT('Ctrl Pts',(1.99691126398784,9.8812874714592,-1.55276477756863));
#45035=CARTESIAN_POINT('Ctrl Pts',(2.18986969302056,9.92370211108617,-1.27142384596148));
#45036=CARTESIAN_POINT('Ctrl Pts',(2.44645069525432,9.98345908137755,-0.653396472215422));
#45037=CARTESIAN_POINT('Ctrl Pts',(2.51,10.,-0.316602390110811));
#45038=CARTESIAN_POINT('Ctrl Pts',(2.51,10.,0.316602390110811));
#45039=CARTESIAN_POINT('Ctrl Pts',(2.44645069525432,9.98345908137755,0.653396472215422));
#45040=CARTESIAN_POINT('Ctrl Pts',(2.18986969302056,9.92370211108617,1.27142384596148));
#45041=CARTESIAN_POINT('Ctrl Pts',(1.99691126398784,9.8812874714592,1.55276477756863));
#45042=CARTESIAN_POINT('Ctrl Pts',(1.55273320805174,9.80118127300772,1.99694283350472));
#45043=CARTESIAN_POINT('Ctrl Pts',(1.27140541887387,9.75816738483577,2.18987665098482));
#45044=CARTESIAN_POINT('Ctrl Pts',(0.653424667393655,9.69702654534655,2.4464396819459));
#45045=CARTESIAN_POINT('Ctrl Pts',(0.316647397714408,9.67987086690727,2.51));
#45046=CARTESIAN_POINT('Ctrl Pts',(-6.93889390390723E-17,9.67987086690727,
2.51));
#45047=CARTESIAN_POINT('Ctrl Pts',(2.51,-10.,0.));
#45048=CARTESIAN_POINT('Ctrl Pts',(2.51,-10.,-0.316602390110811));
#45049=CARTESIAN_POINT('Ctrl Pts',(2.44645069525432,-9.98345908137755,-0.653396472215422));
#45050=CARTESIAN_POINT('Ctrl Pts',(2.18986969302056,-9.92370211108617,-1.27142384596148));
#45051=CARTESIAN_POINT('Ctrl Pts',(1.99691126398784,-9.8812874714592,-1.55276477756863));
#45052=CARTESIAN_POINT('Ctrl Pts',(1.55273320805174,-9.80118127300772,-1.99694283350472));
#45053=CARTESIAN_POINT('Ctrl Pts',(1.27140541887387,-9.75816738483577,-2.18987665098482));
#45054=CARTESIAN_POINT('Ctrl Pts',(0.653424667393654,-9.69702654534655,
-2.4464396819459));
#45055=CARTESIAN_POINT('Ctrl Pts',(0.316647397714408,-9.67987086690727,
-2.51));
#45056=CARTESIAN_POINT('Ctrl Pts',(-0.316647397714408,-9.67987086690727,
-2.51));
#45057=CARTESIAN_POINT('Ctrl Pts',(-0.653424667393654,-9.69702654534655,
-2.4464396819459));
#45058=CARTESIAN_POINT('Ctrl Pts',(-1.27140541887387,-9.75816738483577,
-2.18987665098482));
#45059=CARTESIAN_POINT('Ctrl Pts',(-1.55273320805174,-9.80118127300772,
-1.99694283350472));
#45060=CARTESIAN_POINT('Ctrl Pts',(-1.99691126398784,-9.8812874714592,-1.55276477756863));
#45061=CARTESIAN_POINT('Ctrl Pts',(-2.18986969302057,-9.92370211108617,
-1.27142384596148));
#45062=CARTESIAN_POINT('Ctrl Pts',(-2.44645069525432,-9.98345908137755,
-0.653396472215421));
#45063=CARTESIAN_POINT('Ctrl Pts',(-2.51,-10.,-0.316602390110811));
#45064=CARTESIAN_POINT('Ctrl Pts',(-2.51,-10.,-3.46944695195361E-16));
#45065=CARTESIAN_POINT('Origin',(-4.5,9.6,0.));
#45066=CARTESIAN_POINT('',(-4.49999999999999,-9.6,-1.17566092718146E-15));
#45067=CARTESIAN_POINT('Origin',(-4.49999999999999,0.,0.));
#45068=CARTESIAN_POINT('Origin',(-4.3,0.,0.));
#45069=CARTESIAN_POINT('',(-4.1,-10.,-1.22464679914735E-15));
#45070=CARTESIAN_POINT('Origin',(-4.1,0.,0.));
#45071=CARTESIAN_POINT('',(-4.3,-9.8,-1.20015386316441E-15));
#45072=CARTESIAN_POINT('Origin',(17.95,0.,0.));
#45073=CARTESIAN_POINT('',(40.,-10.,-1.22464679914735E-15));
#45074=CARTESIAN_POINT('Origin',(40.,0.,0.));
#45075=CARTESIAN_POINT('',(17.95,-10.,-1.22464679914735E-15));
#45076=CARTESIAN_POINT('',(17.95,-10.,-1.22464679914735E-15));
#45077=CARTESIAN_POINT('Origin',(40.25,0.,0.));
#45078=CARTESIAN_POINT('',(40.5,-12.5,-1.53080849893419E-15));
#45079=CARTESIAN_POINT('Origin',(40.5,0.,0.));
#45080=CARTESIAN_POINT('',(40.25,-11.25,-1.37772764904077E-15));
#45081=CARTESIAN_POINT('Origin',(61.25,0.,0.));
#45082=CARTESIAN_POINT('',(82.,-12.5,-1.53080849893419E-15));
#45083=CARTESIAN_POINT('Origin',(82.,0.,0.));
#45084=CARTESIAN_POINT('',(61.25,-12.5,-1.53080849893419E-15));
#45085=CARTESIAN_POINT('Origin',(82.,15.,0.));
#45086=CARTESIAN_POINT('',(82.,-15.,-1.83697019872103E-15));
#45087=CARTESIAN_POINT('Origin',(82.,0.,0.));
#45088=CARTESIAN_POINT('Origin',(97.5,0.,0.));
#45089=CARTESIAN_POINT('',(113.,-15.,-1.83697019872103E-15));
#45090=CARTESIAN_POINT('Origin',(113.,0.,0.));
#45091=CARTESIAN_POINT('',(97.5,-15.,-1.83697019872103E-15));
#45092=CARTESIAN_POINT('Origin',(113.,12.5,0.));
#45093=CARTESIAN_POINT('',(113.,-12.5,-1.53080849893419E-15));
#45094=CARTESIAN_POINT('Origin',(113.,0.,0.));
#45095=CARTESIAN_POINT('Origin',(120.5,0.,0.));
#45096=CARTESIAN_POINT('',(128.,-12.5,-1.53080849893419E-15));
#45097=CARTESIAN_POINT('Origin',(128.,0.,0.));
#45098=CARTESIAN_POINT('',(120.5,-12.5,-1.53080849893419E-15));
#45099=CARTESIAN_POINT('Origin',(128.,11.95,0.));
#45100=CARTESIAN_POINT('',(128.,-11.95,-1.46345292498109E-15));
#45101=CARTESIAN_POINT('Origin',(128.,0.,0.));
#45102=CARTESIAN_POINT('Origin',(128.625,0.,0.));
#45103=CARTESIAN_POINT('',(129.25,-11.95,-1.46345292498109E-15));
#45104=CARTESIAN_POINT('Origin',(129.25,0.,0.));
#45105=CARTESIAN_POINT('',(128.625,-11.95,-1.46345292498109E-15));
#45106=CARTESIAN_POINT('Origin',(129.25,12.5,0.));
#45107=CARTESIAN_POINT('',(129.25,-12.5,-1.53080849893419E-15));
#45108=CARTESIAN_POINT('Origin',(129.25,0.,0.));
#45109=CARTESIAN_POINT('Origin',(134.625,0.,0.));
#45110=CARTESIAN_POINT('',(140.,-12.5,-1.53080849893419E-15));
#45111=CARTESIAN_POINT('Origin',(140.,0.,0.));
#45112=CARTESIAN_POINT('',(134.625,-12.5,-1.53080849893419E-15));
#45113=CARTESIAN_POINT('Origin',(140.,10.,0.));
#45114=CARTESIAN_POINT('',(140.,-10.,-1.22464679914735E-15));
#45115=CARTESIAN_POINT('Origin',(140.,0.,0.));
#45116=CARTESIAN_POINT('Origin',(167.25,0.,0.));
#45117=CARTESIAN_POINT('',(194.5,-10.,-1.22464679914735E-15));
#45118=CARTESIAN_POINT('Origin',(194.5,0.,0.));
#45119=CARTESIAN_POINT('',(167.25,-10.,-1.22464679914735E-15));
#45120=CARTESIAN_POINT('Origin',(194.75,0.,0.));
#45121=CARTESIAN_POINT('',(195.,-9.50000000000001,-1.16341445918999E-15));
#45122=CARTESIAN_POINT('Origin',(195.,0.,0.));
#45123=CARTESIAN_POINT('',(194.75,-9.75,-1.19403062916867E-15));
#45124=CARTESIAN_POINT('Origin',(195.,0.,0.));
#45125=CARTESIAN_POINT('',(0.,0.,0.));
#45126=CARTESIAN_POINT('Origin',(0.35,0.,0.));
#45127=CARTESIAN_POINT('',(0.7,-16.,-1.95943487863577E-15));
#45128=CARTESIAN_POINT('Origin',(0.7,0.,0.));
#45129=CARTESIAN_POINT('',(-3.46944695195361E-16,-15.8,-1.93494194265282E-15));
#45130=CARTESIAN_POINT('',(0.35,-15.9,-1.94718841064429E-15));
#45131=CARTESIAN_POINT('Origin',(0.,0.,0.));
#45132=CARTESIAN_POINT('Origin',(0.7,22.6,0.));
#45133=CARTESIAN_POINT('',(0.700000000000001,-22.6,-2.76770176607302E-15));
#45134=CARTESIAN_POINT('Origin',(0.7,0.,0.));
#45135=CARTESIAN_POINT('Origin',(0.35,0.,0.));
#45136=CARTESIAN_POINT('',(3.46944695195361E-16,-22.8,-2.79219470205597E-15));
#45137=CARTESIAN_POINT('',(0.35,-22.7,-2.77994823406449E-15));
#45138=CARTESIAN_POINT('Origin',(0.,0.,0.));
#45139=CARTESIAN_POINT('Origin',(0.,25.55,0.));
#45140=CARTESIAN_POINT('',(-4.5102810375397E-16,-25.55,-3.12897257182149E-15));
#45141=CARTESIAN_POINT('Origin',(0.,0.,0.));
#45142=CARTESIAN_POINT('Origin',(0.225,0.,0.));
#45143=CARTESIAN_POINT('',(0.45,-26.,-3.18408167778312E-15));
#45144=CARTESIAN_POINT('Origin',(0.45,0.,0.));
#45145=CARTESIAN_POINT('',(0.225,-25.775,-3.1565271248023E-15));
#45146=CARTESIAN_POINT('Origin',(7.5,0.,0.));
#45147=CARTESIAN_POINT('',(14.55,-26.,-3.18408167778312E-15));
#45148=CARTESIAN_POINT('Origin',(14.55,0.,0.));
#45149=CARTESIAN_POINT('',(7.5,-26.,-3.18408167778312E-15));
#45150=CARTESIAN_POINT('Origin',(14.775,0.,0.));
#45151=CARTESIAN_POINT('',(15.,-25.55,-3.12897257182149E-15));
#45152=CARTESIAN_POINT('Origin',(15.,0.,0.));
#45153=CARTESIAN_POINT('',(14.775,-25.775,-3.1565271248023E-15));
#45154=CARTESIAN_POINT('Origin',(15.,22.8,0.));
#45155=CARTESIAN_POINT('',(15.,-22.8,-2.79219470205597E-15));
#45156=CARTESIAN_POINT('Origin',(15.,0.,0.));
#45157=CARTESIAN_POINT('Origin',(14.65,0.,0.));
#45158=CARTESIAN_POINT('',(14.3,-22.6,-2.76770176607302E-15));
#45159=CARTESIAN_POINT('',(14.65,-22.7,-2.77994823406449E-15));
#45160=CARTESIAN_POINT('Origin',(14.3,0.,0.));
#45161=CARTESIAN_POINT('Origin',(14.3,16.,0.));
#45162=CARTESIAN_POINT('',(14.3,-16.,-1.95943487863577E-15));
#45163=CARTESIAN_POINT('Origin',(14.3,0.,0.));
#45164=CARTESIAN_POINT('Origin',(14.65,0.,0.));
#45165=CARTESIAN_POINT('',(15.,-15.8,-1.93494194265282E-15));
#45166=CARTESIAN_POINT('Origin',(15.,0.,0.));
#45167=CARTESIAN_POINT('',(14.65,-15.9,-1.94718841064429E-15));
#45168=CARTESIAN_POINT('Origin',(15.,12.95,0.));
#45169=CARTESIAN_POINT('',(15.,-12.95,-1.58591760489582E-15));
#45170=CARTESIAN_POINT('Origin',(15.,0.,0.));
#45171=CARTESIAN_POINT('Origin',(14.775,0.,0.));
#45172=CARTESIAN_POINT('',(14.55,-12.5,-1.53080849893419E-15));
#45173=CARTESIAN_POINT('',(14.775,-12.725,-1.55836305191501E-15));
#45174=CARTESIAN_POINT('Origin',(14.55,0.,0.));
#45175=CARTESIAN_POINT('Origin',(7.5,0.,0.));
#45176=CARTESIAN_POINT('',(0.45,-12.5,-1.53080849893419E-15));
#45177=CARTESIAN_POINT('',(7.5,-12.5,-1.53080849893419E-15));
#45178=CARTESIAN_POINT('Origin',(0.45,0.,0.));
#45179=CARTESIAN_POINT('Origin',(0.225,0.,0.));
#45180=CARTESIAN_POINT('',(-2.08166817117217E-16,-12.95,-1.58591760489582E-15));
#45181=CARTESIAN_POINT('',(0.225,-12.725,-1.55836305191501E-15));
#45182=CARTESIAN_POINT('Origin',(0.,0.,0.));
#45183=CARTESIAN_POINT('Origin',(0.,15.8,0.));
#45184=CARTESIAN_POINT('',(0.,0.,0.));
#45185=CARTESIAN_POINT('Origin',(16.75,0.,0.));
#45186=CARTESIAN_POINT('',(17.,17.5,-2.14313189850787E-15));
#45187=CARTESIAN_POINT('Origin',(17.,0.,0.));
#45188=CARTESIAN_POINT('',(16.5,18.,2.20436423846524E-15));
#45189=CARTESIAN_POINT('',(16.75,17.75,2.17374806848655E-15));
#45190=CARTESIAN_POINT('',(16.5,-18.,-2.20436423846524E-15));
#45191=CARTESIAN_POINT('Origin',(16.5,0.,0.));
#45192=CARTESIAN_POINT('Origin',(16.5,0.,0.));
#45193=CARTESIAN_POINT('Origin',(11.5,0.,0.));
#45194=CARTESIAN_POINT('',(6.,-18.,-2.20436423846524E-15));
#45195=CARTESIAN_POINT('',(11.5,-18.,-2.20436423846524E-15));
#45196=CARTESIAN_POINT('Origin',(6.,0.,0.));
#45197=CARTESIAN_POINT('Origin',(17.,16.,0.));
#45198=CARTESIAN_POINT('',(17.,-16.,-1.95943487863577E-15));
#45199=CARTESIAN_POINT('Origin',(17.,0.,0.));
#45200=CARTESIAN_POINT('Origin',(11.,0.,0.));
#45201=CARTESIAN_POINT('',(17.,-10.,-1.22464679914735E-15));
#45202=CARTESIAN_POINT('Origin',(17.,0.,0.));
#45203=CARTESIAN_POINT('',(5.,-10.,-1.22464679914735E-15));
#45204=CARTESIAN_POINT('',(11.,-10.,-1.22464679914735E-15));
#45205=CARTESIAN_POINT('Origin',(5.,0.,0.));
#45206=CARTESIAN_POINT('Origin',(5.,17.,0.));
#45207=CARTESIAN_POINT('',(5.,-17.,-2.0818995585505E-15));
#45208=CARTESIAN_POINT('Origin',(5.,0.,0.));
#45209=CARTESIAN_POINT('Origin',(5.5,0.,0.));
#45210=CARTESIAN_POINT('',(5.5,-17.5,-2.14313189850787E-15));
#45211=CARTESIAN_POINT('Origin',(19.5,0.,0.));
#45212=CARTESIAN_POINT('',(22.,-16.,-1.95943487863577E-15));
#45213=CARTESIAN_POINT('Origin',(22.,0.,0.));
#45214=CARTESIAN_POINT('',(19.5,-16.,-1.95943487863577E-15));
#45215=CARTESIAN_POINT('Origin',(22.,13.,0.));
#45216=CARTESIAN_POINT('',(22.,-13.,-1.59204083889156E-15));
#45217=CARTESIAN_POINT('Origin',(22.,0.,0.));
#45218=CARTESIAN_POINT('Origin',(19.5,0.,0.));
#45219=CARTESIAN_POINT('',(17.,-13.,-1.59204083889156E-15));
#45220=CARTESIAN_POINT('',(19.5,-13.,-1.59204083889156E-15));
#45221=CARTESIAN_POINT('Origin',(17.,0.,0.));
#45222=CARTESIAN_POINT('Origin',(17.,10.,0.));
#45223=CARTESIAN_POINT('',(0.,0.,0.));
#45224=CARTESIAN_POINT('Origin',(26.,0.,0.));
#45225=CARTESIAN_POINT('',(30.,-13.,-1.59204083889156E-15));
#45226=CARTESIAN_POINT('Origin',(30.,0.,0.));
#45227=CARTESIAN_POINT('',(22.,-13.,-1.59204083889156E-15));
#45228=CARTESIAN_POINT('',(26.,-13.,-1.59204083889156E-15));
#45229=CARTESIAN_POINT('Origin',(22.,0.,0.));
#45230=CARTESIAN_POINT('Origin',(22.,19.5,0.));
#45231=CARTESIAN_POINT('',(22.,-19.5,-2.38806125833734E-15));
#45232=CARTESIAN_POINT('Origin',(22.,0.,0.));
#45233=CARTESIAN_POINT('Origin',(22.25,0.,0.));
#45234=CARTESIAN_POINT('',(22.5,-20.,-2.44929359829471E-15));
#45235=CARTESIAN_POINT('Origin',(22.5,0.,0.));
#45236=CARTESIAN_POINT('',(22.25,-19.75,-2.41867742831602E-15));
#45237=CARTESIAN_POINT('Origin',(26.25,0.,0.));
#45238=CARTESIAN_POINT('',(30.,-20.,-2.44929359829471E-15));
#45239=CARTESIAN_POINT('Origin',(30.,0.,0.));
#45240=CARTESIAN_POINT('',(26.25,-20.,-2.44929359829471E-15));
#45241=CARTESIAN_POINT('Origin',(30.,13.,0.));
#45242=CARTESIAN_POINT('',(0.,0.,0.));
#45243=CARTESIAN_POINT('Origin',(-11.5,2.2,0.));
#45244=CARTESIAN_POINT('',(-11.5,-2.2,-2.69422295812418E-16));
#45245=CARTESIAN_POINT('Origin',(-11.5,0.,0.));
#45246=CARTESIAN_POINT('Origin',(-11.35,0.,0.));
#45247=CARTESIAN_POINT('',(-11.2,-2.5,-3.06161699786838E-16));
#45248=CARTESIAN_POINT('Origin',(-11.2,0.,0.));
#45249=CARTESIAN_POINT('',(-11.35,-2.35,-2.87791997799628E-16));
#45250=CARTESIAN_POINT('Origin',(0.,0.,0.));
#45251=CARTESIAN_POINT('',(11.2,-2.5,-3.06161699786838E-16));
#45252=CARTESIAN_POINT('Origin',(11.2,0.,0.));
#45253=CARTESIAN_POINT('',(0.,-2.5,-3.06161699786838E-16));
#45254=CARTESIAN_POINT('Origin',(11.35,0.,0.));
#45255=CARTESIAN_POINT('',(11.5,-2.2,-2.69422295812418E-16));
#45256=CARTESIAN_POINT('Origin',(11.5,0.,0.));
#45257=CARTESIAN_POINT('',(11.35,-2.35,-2.87791997799628E-16));
#45258=CARTESIAN_POINT('Origin',(11.5,0.,0.));
#45259=CARTESIAN_POINT('',(0.,0.,0.));
#45260=CARTESIAN_POINT('Origin',(0.25,0.,0.));
#45261=CARTESIAN_POINT('',(0.5,-12.55,-1.53693173292993E-15));
#45262=CARTESIAN_POINT('Origin',(0.5,0.,0.));
#45263=CARTESIAN_POINT('',(0.,-12.55,-1.53693173292993E-15));
#45264=CARTESIAN_POINT('',(0.25,-12.55,-1.53693173292993E-15));
#45265=CARTESIAN_POINT('Origin',(0.,0.,0.));
#45266=CARTESIAN_POINT('Origin',(0.,16.,0.));
#45267=CARTESIAN_POINT('',(0.,-16.,-1.95943487863577E-15));
#45268=CARTESIAN_POINT('Origin',(0.,0.,0.));
#45269=CARTESIAN_POINT('Origin',(0.25,0.,0.));
#45270=CARTESIAN_POINT('',(0.5,-16.,-1.95943487863577E-15));
#45271=CARTESIAN_POINT('Origin',(0.5,0.,0.));
#45272=CARTESIAN_POINT('',(0.25,-16.,-1.95943487863577E-15));
#45273=CARTESIAN_POINT('Origin',(0.5,12.55,0.));
#45274=CARTESIAN_POINT('',(0.,0.,0.));
#45275=CARTESIAN_POINT('Origin',(-1.5,0.,0.));
#45276=CARTESIAN_POINT('',(-1.5,-8.81745695386094E-15,72.));
#45277=CARTESIAN_POINT('Origin',(-1.5,-9.00115397373305E-15,73.5));
#45278=CARTESIAN_POINT('Origin',(-1.5,0.,0.));
#45279=CARTESIAN_POINT('',(0.,0.,0.));
#45280=CARTESIAN_POINT('Origin',(1.1,3.1,7.78717523412628));
#45281=CARTESIAN_POINT('',(1.,3.,15.7162336455017));
#45282=CARTESIAN_POINT('',(1.,3.,11.5673030564605));
#45283=CARTESIAN_POINT('',(1.,3.,7.78717523412628));
#45284=CARTESIAN_POINT('',(1.2,3.2,11.5135789396695));
#45285=CARTESIAN_POINT('Origin',(-2.,0.,3.12250225675825E-16));
#45286=CARTESIAN_POINT('',(1.2,3.2,15.4725563498732));
#45287=CARTESIAN_POINT('',(1.2,3.2,7.78717523412628));
#45288=CARTESIAN_POINT('Ctrl Pts',(1.2,3.2,15.4725563498732));
#45289=CARTESIAN_POINT('Ctrl Pts',(1.13355790711216,3.13355790711216,15.554145955128));
#45290=CARTESIAN_POINT('Ctrl Pts',(1.06688589706653,3.06688589706653,15.6353725388951));
#45291=CARTESIAN_POINT('Ctrl Pts',(1.,3.,15.7162336455017));
#45292=CARTESIAN_POINT('Origin',(1.1,0.,-1.90819582357449E-16));
#45293=CARTESIAN_POINT('',(1.2,-3.2,15.4725563498732));
#45294=CARTESIAN_POINT('Origin',(1.2,0.,-1.90819582357449E-16));
#45295=CARTESIAN_POINT('',(1.,-3.,15.7162336455017));
#45296=CARTESIAN_POINT('Ctrl Pts',(1.2,-3.2,15.4725563498732));
#45297=CARTESIAN_POINT('Ctrl Pts',(1.13355790711234,-3.13355790711234,15.5541459551277));
#45298=CARTESIAN_POINT('Ctrl Pts',(1.06688589706689,-3.0668858970669,15.6353725388946));
#45299=CARTESIAN_POINT('Ctrl Pts',(1.,-3.,15.7162336455017));
#45300=CARTESIAN_POINT('Origin',(1.,0.,-1.90819582357449E-16));
#45301=CARTESIAN_POINT('Origin',(1.1,-3.1,5.71270993960567));
#45302=CARTESIAN_POINT('',(1.2,-3.2,11.5135789396695));
#45303=CARTESIAN_POINT('',(1.2,-3.2,5.71270993960567));
#45304=CARTESIAN_POINT('',(1.,-3.,11.5673030564605));
#45305=CARTESIAN_POINT('Origin',(-2.,0.,3.12250225675825E-16));
#45306=CARTESIAN_POINT('',(1.,-3.,5.71270993960567));
#45307=CARTESIAN_POINT('Origin',(1.2,0.,-0.141883177249145));
#45308=CARTESIAN_POINT('Origin',(1.2,0.,3.12250225675825E-16));
#45309=CARTESIAN_POINT('Origin',(0.1,3.1,7.78717523412628));
#45310=CARTESIAN_POINT('',(0.,3.2,15.4725563498732));
#45311=CARTESIAN_POINT('',(0.,3.2,11.5135789396695));
#45312=CARTESIAN_POINT('',(0.,3.2,7.78717523412628));
#45313=CARTESIAN_POINT('',(0.2,3.,11.5673030564605));
#45314=CARTESIAN_POINT('Origin',(3.2,0.,3.12250225675825E-16));
#45315=CARTESIAN_POINT('',(0.2,3.,15.7162336455017));
#45316=CARTESIAN_POINT('',(0.2,3.,7.78717523412628));
#45317=CARTESIAN_POINT('Ctrl Pts',(0.2,3.,15.7162336455017));
#45318=CARTESIAN_POINT('Ctrl Pts',(0.133114102933436,3.06688589706656,15.635372538895));
#45319=CARTESIAN_POINT('Ctrl Pts',(0.0664420928878206,3.13355790711218,
15.5541459551279));
#45320=CARTESIAN_POINT('Ctrl Pts',(-1.96023752785379E-15,3.2,15.4725563498732));
#45321=CARTESIAN_POINT('Origin',(0.1,-3.1,5.71270993960567));
#45322=CARTESIAN_POINT('',(0.2,-3.,15.7162336455017));
#45323=CARTESIAN_POINT('',(0.2,-3.,11.5673030564605));
#45324=CARTESIAN_POINT('',(0.2,-3.,5.71270993960567));
#45325=CARTESIAN_POINT('',(0.,-3.2,11.5135789396695));
#45326=CARTESIAN_POINT('Origin',(3.2,0.,3.12250225675825E-16));
#45327=CARTESIAN_POINT('',(0.,-3.2,15.4725563498732));
#45328=CARTESIAN_POINT('',(0.,-3.2,5.71270993960567));
#45329=CARTESIAN_POINT('Ctrl Pts',(-2.94902990916057E-16,-3.2,15.4725563498732));
#45330=CARTESIAN_POINT('Ctrl Pts',(0.066442092887622,-3.13355790711238,
15.5541459551277));
#45331=CARTESIAN_POINT('Ctrl Pts',(0.133114102933025,-3.06688589706697,
15.6353725388945));
#45332=CARTESIAN_POINT('Ctrl Pts',(0.2,-3.,15.7162336455017));
#45333=CARTESIAN_POINT('Origin',(0.1,0.,-1.90819582357449E-16));
#45334=CARTESIAN_POINT('Origin',(0.2,0.,-1.90819582357449E-16));
#45335=CARTESIAN_POINT('Origin',(0.,0.,-1.90819582357449E-16));
#45336=CARTESIAN_POINT('Origin',(0.,0.,-0.141883177249145));
#45337=CARTESIAN_POINT('Origin',(0.,0.,3.12250225675825E-16));
#45338=CARTESIAN_POINT('Origin',(0.,-3.,11.5673030564605));
#45339=CARTESIAN_POINT('',(0.,-3.,11.5673030564605));
#45340=CARTESIAN_POINT('',(0.,-3.,15.7162336455017));
#45341=CARTESIAN_POINT('Origin',(0.,0.,-1.90819582357449E-16));
#45342=CARTESIAN_POINT('',(0.,3.,15.7162336455017));
#45343=CARTESIAN_POINT('Origin',(0.,0.,3.12250225675825E-16));
#45344=CARTESIAN_POINT('',(0.,3.,11.5673030564605));
#45345=CARTESIAN_POINT('Origin',(0.,3.,15.7162336455017));
#45346=CARTESIAN_POINT('',(0.,0.,0.));
#45347=CARTESIAN_POINT('Origin',(1.8,3.5,21.9198066289735));
#45348=CARTESIAN_POINT('',(1.8,3.5,21.9198066289735));
#45349=CARTESIAN_POINT('',(2.,3.7,21.8894951974686));
#45350=CARTESIAN_POINT('',(1.8,3.5,21.9198066289735));
#45351=CARTESIAN_POINT('',(1.8,3.69730611962488,21.6870912631866));
#45352=CARTESIAN_POINT('',(1.8,3.69730611962488,21.6870912631866));
#45353=CARTESIAN_POINT('Ctrl Pts',(1.79999999999876,3.69730611962487,21.6870912631853));
#45354=CARTESIAN_POINT('Ctrl Pts',(1.89946355488301,3.69863475902964,21.7877634000965));
#45355=CARTESIAN_POINT('Ctrl Pts',(2.,3.7,21.8894951974686));
#45356=CARTESIAN_POINT('Origin',(0.2,3.5,21.9198066289735));
#45357=CARTESIAN_POINT('',(0.2,3.5,21.9198066289735));
#45358=CARTESIAN_POINT('',(0.2,3.69730611962488,21.6870912631866));
#45359=CARTESIAN_POINT('',(0.2,3.5,21.9198066289735));
#45360=CARTESIAN_POINT('',(0.,3.7,21.8894951974686));
#45361=CARTESIAN_POINT('',(0.,3.7,21.8894951974686));
#45362=CARTESIAN_POINT('Ctrl Pts',(-2.94902990916057E-16,3.7,21.8894951974686));
#45363=CARTESIAN_POINT('Ctrl Pts',(0.100536445051347,3.69863475903052,21.7877634001629));
#45364=CARTESIAN_POINT('Ctrl Pts',(0.200000000000001,3.69730611962489,21.6870912631866));
#45365=CARTESIAN_POINT('Origin',(0.1,3.6,13.5822725454788));
#45366=CARTESIAN_POINT('',(0.2,3.5,27.2763633939717));
#45367=CARTESIAN_POINT('',(0.,3.7,27.2499541284018));
#45368=CARTESIAN_POINT('Origin',(3.7,0.,1.21430643318376E-16));
#45369=CARTESIAN_POINT('',(0.,3.7,13.5822725454788));
#45370=CARTESIAN_POINT('',(0.2,3.5,13.5822725454788));
#45371=CARTESIAN_POINT('Origin',(1.8,-3.69730611962489,21.6870912631866));
#45372=CARTESIAN_POINT('',(1.8,-3.69730611962489,21.6870912631866));
#45373=CARTESIAN_POINT('',(2.,-3.7,21.8894951974686));
#45374=CARTESIAN_POINT('Ctrl Pts',(2.,-3.7,21.8894951974686));
#45375=CARTESIAN_POINT('Ctrl Pts',(1.89946355488263,-3.69863475902964,21.7877634000961));
#45376=CARTESIAN_POINT('Ctrl Pts',(1.79999999999876,-3.69730611962488,21.6870912631853));
#45377=CARTESIAN_POINT('',(1.8,-3.5,21.9198066289735));
#45378=CARTESIAN_POINT('',(1.8,-3.5,21.9198066289735));
#45379=CARTESIAN_POINT('',(2.,-3.7,21.8894951974686));
#45380=CARTESIAN_POINT('Origin',(0.2,-3.69730611962489,21.6870912631866));
#45381=CARTESIAN_POINT('',(0.2,-3.69730611962489,21.6870912631866));
#45382=CARTESIAN_POINT('',(0.2,-3.5,21.9198066289735));
#45383=CARTESIAN_POINT('',(0.2,-3.69730611962489,21.6870912631866));
#45384=CARTESIAN_POINT('',(0.,-3.7,21.8894951974686));
#45385=CARTESIAN_POINT('Ctrl Pts',(0.199999999999999,-3.6973061196249,21.6870912631866));
#45386=CARTESIAN_POINT('Ctrl Pts',(0.100536445422227,-3.69863475902553,
21.7877633997876));
#45387=CARTESIAN_POINT('Ctrl Pts',(-9.8879238130678E-16,-3.7,21.8894951974686));
#45388=CARTESIAN_POINT('',(0.2,-3.5,21.9198066289735));
#45389=CARTESIAN_POINT('Origin',(0.1,-2.77555756156289E-16,-8.67361737988404E-16));
#45390=CARTESIAN_POINT('Origin',(0.,-2.77555756156289E-16,-8.67361737988404E-16));
#45391=CARTESIAN_POINT('Origin',(0.2,-2.77555756156289E-16,-8.67361737988404E-16));
#45392=CARTESIAN_POINT('Origin',(0.1,-3.6,10.8039941629797));
#45393=CARTESIAN_POINT('',(0.,-3.7,27.2499541284018));
#45394=CARTESIAN_POINT('',(0.2,-3.5,27.2763633939717));
#45395=CARTESIAN_POINT('Origin',(3.7,0.,1.21430643318376E-16));
#45396=CARTESIAN_POINT('',(0.2,-3.5,10.8039941629797));
#45397=CARTESIAN_POINT('',(0.,-3.7,10.8039941629797));
#45398=CARTESIAN_POINT('Origin',(0.,-3.59865305981244,21.80344894608));
#45399=CARTESIAN_POINT('',(0.,-3.69730611962489,21.6870912631866));
#45400=CARTESIAN_POINT('',(0.,-3.5,21.9198066289735));
#45401=CARTESIAN_POINT('Origin',(1.9,-3.6,10.8039941629797));
#45402=CARTESIAN_POINT('',(1.8,-3.5,27.2763633939717));
#45403=CARTESIAN_POINT('',(2.,-3.7,27.2499541284018));
#45404=CARTESIAN_POINT('Origin',(-1.7,0.,1.21430643318376E-16));
#45405=CARTESIAN_POINT('',(2.,-3.7,10.8039941629797));
#45406=CARTESIAN_POINT('',(1.8,-3.5,10.8039941629797));
#45407=CARTESIAN_POINT('Origin',(1.9,-2.77555756156289E-16,-8.67361737988404E-16));
#45408=CARTESIAN_POINT('Origin',(2.,-2.77555756156289E-16,-8.67361737988404E-16));
#45409=CARTESIAN_POINT('Origin',(1.8,-2.77555756156289E-16,-8.67361737988404E-16));
#45410=CARTESIAN_POINT('Origin',(0.,3.59865305981244,21.80344894608));
#45411=CARTESIAN_POINT('',(0.,3.5,21.9198066289735));
#45412=CARTESIAN_POINT('',(0.,3.69730611962488,21.6870912631866));
#45413=CARTESIAN_POINT('Origin',(1.9,3.6,13.5822725454788));
#45414=CARTESIAN_POINT('',(2.,3.7,27.2499541284018));
#45415=CARTESIAN_POINT('',(1.8,3.5,27.2763633939717));
#45416=CARTESIAN_POINT('Origin',(-1.7,0.,1.21430643318376E-16));
#45417=CARTESIAN_POINT('',(1.8,3.5,13.5822725454788));
#45418=CARTESIAN_POINT('',(2.,3.7,13.5822725454788));
#45419=CARTESIAN_POINT('Origin',(0.,0.,-0.11181830301414));
#45420=CARTESIAN_POINT('Origin',(0.,0.,1.21430643318376E-16));
#45421=CARTESIAN_POINT('Origin',(0.,3.5,27.2763633939717));
#45422=CARTESIAN_POINT('',(0.,3.5,27.2763633939717));
#45423=CARTESIAN_POINT('Origin',(0.,-2.77555756156289E-16,-8.67361737988404E-16));
#45424=CARTESIAN_POINT('Origin',(0.,0.,1.21430643318376E-16));
#45425=CARTESIAN_POINT('Origin',(2.,0.,1.21430643318376E-16));
#45426=CARTESIAN_POINT('',(0.,-3.5,27.2763633939717));
#45427=CARTESIAN_POINT('Origin',(0.,-3.5,21.7198066289735));
#45428=CARTESIAN_POINT('Origin',(2.,0.,-0.11181830301414));
#45429=CARTESIAN_POINT('',(0.,0.,0.));
#45430=CARTESIAN_POINT('Origin',(9.87499724990925,0.,-4.41062959606175E-16));
#45431=CARTESIAN_POINT('',(10.,-13.4732,1.64999112542721E-15));
#45432=CARTESIAN_POINT('Origin',(10.,0.,0.));
#45433=CARTESIAN_POINT('',(9.74999449981849,-14.4062095263144,-3.5285036768494E-15));
#45434=CARTESIAN_POINT('',(9.87499724990925,-13.9397047631572,-2.58924740113831E-15));
#45435=CARTESIAN_POINT('Origin',(9.74999449981849,0.,-8.8212591921235E-16));
#45436=CARTESIAN_POINT('Origin',(8.7431870669746,0.,0.));
#45437=CARTESIAN_POINT('',(8.36752131451236,14.5497923702765,-8.40032654163231));
#45438=CARTESIAN_POINT('',(8.36752131451235,-3.33066907387547E-15,-16.8006530832646));
#45439=CARTESIAN_POINT('Ctrl Pts',(8.36752131451236,14.5497923702765,-8.40032654163231));
#45440=CARTESIAN_POINT('Ctrl Pts',(9.15318176943128,12.1845393672071,-9.77553709986417));
#45441=CARTESIAN_POINT('Ctrl Pts',(9.79023847218445,8.88417527786995,-11.6941257536935));
#45442=CARTESIAN_POINT('Ctrl Pts',(9.57244918857082,4.39048143018587,-14.2836892688202));
#45443=CARTESIAN_POINT('Ctrl Pts',(8.89129495112497,1.58239585367736,-15.8934771446516));
#45444=CARTESIAN_POINT('Ctrl Pts',(8.36752131451235,-8.88178419700125E-15,
-16.8006530832646));
#45445=CARTESIAN_POINT('',(8.36752131451236,14.5497923702765,8.4003265416323));
#45446=CARTESIAN_POINT('Ctrl Pts',(8.36752131451236,14.5497923702765,8.4003265416323));
#45447=CARTESIAN_POINT('Ctrl Pts',(9.15318176943128,14.5581331477232,5.66435207548085));
#45448=CARTESIAN_POINT('Ctrl Pts',(9.79054641267288,14.5694951319271,1.84651364397653));
#45449=CARTESIAN_POINT('Ctrl Pts',(9.57257984044265,14.565278525504,-3.33951930676775));
#45450=CARTESIAN_POINT('Ctrl Pts',(8.89129495112498,14.5553528885743,-6.57634356419801));
#45451=CARTESIAN_POINT('Ctrl Pts',(8.36752131451236,14.5497923702765,-8.40032654163231));
#45452=CARTESIAN_POINT('',(8.36752131451236,5.55111512312578E-16,16.8006530832646));
#45453=CARTESIAN_POINT('Ctrl Pts',(8.36752131451236,-5.55111512312578E-16,
16.8006530832646));
#45454=CARTESIAN_POINT('Ctrl Pts',(9.15318176943128,2.37359378051606,15.439889175345));
#45455=CARTESIAN_POINT('Ctrl Pts',(9.79023847218445,5.68532233881341,13.5409843591558));
#45456=CARTESIAN_POINT('Ctrl Pts',(9.57244918857082,10.1747970514685,10.9441130877949));
#45457=CARTESIAN_POINT('Ctrl Pts',(8.89129495112497,12.9729570348969,9.31713358045354));
#45458=CARTESIAN_POINT('Ctrl Pts',(8.36752131451235,14.5497923702765,8.4003265416323));
#45459=CARTESIAN_POINT('',(8.36752131451235,-14.5497923702765,8.4003265416323));
#45460=CARTESIAN_POINT('Ctrl Pts',(8.36752131451235,-14.5497923702765,8.4003265416323));
#45461=CARTESIAN_POINT('Ctrl Pts',(9.15318176943129,-12.1845393672071,9.77553709986416));
#45462=CARTESIAN_POINT('Ctrl Pts',(9.79023847218445,-8.88417527786995,11.6941257536935));
#45463=CARTESIAN_POINT('Ctrl Pts',(9.57244918857083,-4.39048143018589,14.2836892688202));
#45464=CARTESIAN_POINT('Ctrl Pts',(8.89129495112497,-1.58239585367737,15.8934771446515));
#45465=CARTESIAN_POINT('Ctrl Pts',(8.36752131451235,4.44089209850063E-15,
16.8006530832646));
#45466=CARTESIAN_POINT('',(9.65699525572486,-14.5669896065098,-0.00095436007870299));
#45467=CARTESIAN_POINT('Ctrl Pts',(9.65699525572486,-14.5669896065098,-0.000954360078702712));
#45468=CARTESIAN_POINT('Ctrl Pts',(9.65729513939778,-14.5669682027371,1.12120526983947));
#45469=CARTESIAN_POINT('Ctrl Pts',(9.48741922927794,-14.5640378208878,3.74412233894653));
#45470=CARTESIAN_POINT('Ctrl Pts',(8.89129495112497,-14.5553528885743,6.576343564198));
#45471=CARTESIAN_POINT('Ctrl Pts',(8.36752131451236,-14.5497923702765,8.4003265416323));
#45472=CARTESIAN_POINT('',(8.7431870669746,-16.15,-1.97780458062298E-15));
#45473=CARTESIAN_POINT('',(8.36752131451236,-14.5497923702765,-8.4003265416323));
#45474=CARTESIAN_POINT('Ctrl Pts',(8.36752131451236,-14.5497923702765,-8.4003265416323));
#45475=CARTESIAN_POINT('Ctrl Pts',(9.15318176943128,-14.5581331477232,-5.66435207548086));
#45476=CARTESIAN_POINT('Ctrl Pts',(9.5993370197004,-14.5660865366659,-2.99186517342783));
#45477=CARTESIAN_POINT('Ctrl Pts',(9.65689529450055,-14.5669967411007,-0.375007570051427));
#45478=CARTESIAN_POINT('Ctrl Pts',(9.65699525572486,-14.5669896065098,-0.000954360078702712));
#45479=CARTESIAN_POINT('Ctrl Pts',(8.36752131451236,-3.33066907387547E-15,
-16.8006530832646));
#45480=CARTESIAN_POINT('Ctrl Pts',(9.15318176943128,-2.37359378051606,-15.439889175345));
#45481=CARTESIAN_POINT('Ctrl Pts',(9.79023847218444,-5.6853223388134,-13.5409843591558));
#45482=CARTESIAN_POINT('Ctrl Pts',(9.57244918857082,-10.1747970514685,-10.9441130877949));
#45483=CARTESIAN_POINT('Ctrl Pts',(8.89129495112497,-12.9729570348969,-9.31713358045354));
#45484=CARTESIAN_POINT('Ctrl Pts',(8.36752131451235,-14.5497923702765,-8.4003265416323));
#45485=CARTESIAN_POINT('Origin',(10.,0.,0.));
#45486=CARTESIAN_POINT('Origin',(7.68963026555328,-15.,8.16025403784512));
#45487=CARTESIAN_POINT('',(7.68963026555328,-15.,8.16025403784512));
#45488=CARTESIAN_POINT('',(7.6896302655531,-14.5669872981078,8.91025403784439));
#45489=CARTESIAN_POINT('',(7.6896302655531,-15.,8.16025403784439));
#45490=CARTESIAN_POINT('Ctrl Pts',(7.68963026555328,-15.,8.16025403784512));
#45491=CARTESIAN_POINT('Ctrl Pts',(7.80268870802714,-14.9249959521809,8.20015220863497));
#45492=CARTESIAN_POINT('Ctrl Pts',(7.91571517126633,-14.8499724569668,8.24010952390002));
#45493=CARTESIAN_POINT('Ctrl Pts',(8.14167814509372,-14.6999037370903,8.32013340767416));
#45494=CARTESIAN_POINT('Ctrl Pts',(8.2546169532586,-14.6248570018396,8.36020076335937));
#45495=CARTESIAN_POINT('Ctrl Pts',(8.36752131451236,-14.5497923702765,8.4003265416323));
#45496=CARTESIAN_POINT('Ctrl Pts',(8.36752131451235,-14.5497923702765,8.4003265416323));
#45497=CARTESIAN_POINT('Ctrl Pts',(8.25461606995072,-14.5525747644948,8.48539797417988));
#45498=CARTESIAN_POINT('Ctrl Pts',(8.14167637792964,-14.5553988066539,8.57042469607987));
#45499=CARTESIAN_POINT('Ctrl Pts',(7.91571340305211,-14.561130451635,8.74039996027625));
#45500=CARTESIAN_POINT('Ctrl Pts',(7.80268782367441,-14.5640381267354,8.8253502057819));
#45501=CARTESIAN_POINT('Ctrl Pts',(7.6896302655536,-14.5669872981074,8.91025403784458));
#45502=CARTESIAN_POINT('Origin',(8.36752131451236,5.55111512312578E-16,
16.8006530832646));
#45503=CARTESIAN_POINT('',(7.68963026555329,-0.433012701891581,17.0705080756891));
#45504=CARTESIAN_POINT('Ctrl Pts',(7.68963026555328,-0.433012701891577,
17.0705080756891));
#45505=CARTESIAN_POINT('Ctrl Pts',(7.80268870801826,-0.360957848519129,
17.0255017502896));
#45506=CARTESIAN_POINT('Ctrl Pts',(7.91571517126183,-0.288842050822766,
16.9805081551843));
#45507=CARTESIAN_POINT('Ctrl Pts',(8.14167814510512,-0.144504974616458,
16.8905567733386));
#45508=CARTESIAN_POINT('Ctrl Pts',(8.25461695326423,-0.072282259108921,
16.8455980719853));
#45509=CARTESIAN_POINT('Ctrl Pts',(8.36752131451235,4.44089209850063E-15,
16.8006530832646));
#45510=CARTESIAN_POINT('',(7.68963026555311,0.43301270189222,17.0705080756888));
#45511=CARTESIAN_POINT('Ctrl Pts',(8.36752131451236,1.66533453693773E-15,
16.8006530832646));
#45512=CARTESIAN_POINT('Ctrl Pts',(8.25461606995411,0.0722828246112067,
16.8455984236135));
#45513=CARTESIAN_POINT('Ctrl Pts',(8.14167637793691,0.144506104695097,16.8905574768131));
#45514=CARTESIAN_POINT('Ctrl Pts',(7.91571340304379,0.288843179023551,16.9805088590765));
#45515=CARTESIAN_POINT('Ctrl Pts',(7.80268782365699,0.360958412144736,17.0255021023359));
#45516=CARTESIAN_POINT('Ctrl Pts',(7.6896302655536,0.433012701892559,17.0705080756886));
#45517=CARTESIAN_POINT('',(7.68963026555311,-0.43301270189222,17.0705080756888));
#45518=CARTESIAN_POINT('Origin',(7.68963026555328,-14.5669872981084,-8.91025403784402));
#45519=CARTESIAN_POINT('',(7.68963026555328,-14.5669872981084,-8.91025403784402));
#45520=CARTESIAN_POINT('',(7.6896302655531,-15.,-8.16025403784439));
#45521=CARTESIAN_POINT('',(7.6896302655531,-14.5669872981078,-8.91025403784439));
#45522=CARTESIAN_POINT('Ctrl Pts',(7.68963026555328,-14.5669872981084,-8.91025403784402));
#45523=CARTESIAN_POINT('Ctrl Pts',(7.80268870801892,-14.5640381036676,-8.82534954165722));
#45524=CARTESIAN_POINT('Ctrl Pts',(7.91571517126228,-14.561130406147,-8.74039863128551));
#45525=CARTESIAN_POINT('Ctrl Pts',(8.14167814509705,-14.5553987624665,-8.57042336566644));
#45526=CARTESIAN_POINT('Ctrl Pts',(8.25461695326025,-14.552574742727,-8.4853973086269));
#45527=CARTESIAN_POINT('Ctrl Pts',(8.36752131451236,-14.5497923702765,-8.40032654163231));
#45528=CARTESIAN_POINT('Ctrl Pts',(8.36752131451236,-14.5497923702765,-8.4003265416323));
#45529=CARTESIAN_POINT('Ctrl Pts',(8.25461606994656,-14.624857589111,-8.36020044943344));
#45530=CARTESIAN_POINT('Ctrl Pts',(8.14167637792168,-14.6999049113589,-8.32013278073326));
#45531=CARTESIAN_POINT('Ctrl Pts',(7.91571340304811,-14.8499736306559,-8.24010889879555));
#45532=CARTESIAN_POINT('Ctrl Pts',(7.80268782366648,-14.9249965388743,-8.20015189654426));
#45533=CARTESIAN_POINT('Ctrl Pts',(7.6896302655536,-15.,-8.160254037844));
#45534=CARTESIAN_POINT('Origin',(8.36752131451236,14.5497923702765,8.4003265416323));
#45535=CARTESIAN_POINT('',(7.68963026555328,14.5669872981084,8.91025403784402));
#45536=CARTESIAN_POINT('Ctrl Pts',(7.68963026555328,14.5669872981084,8.91025403784401));
#45537=CARTESIAN_POINT('Ctrl Pts',(7.8026887080225,14.5640381036675,8.82534954165453));
#45538=CARTESIAN_POINT('Ctrl Pts',(7.91571517126384,14.561130406147,8.74039863128433));
#45539=CARTESIAN_POINT('Ctrl Pts',(8.14167814509868,14.5553987624664,8.5704233656652));
#45540=CARTESIAN_POINT('Ctrl Pts',(8.25461695326104,14.552574742727,8.4853973086263));
#45541=CARTESIAN_POINT('Ctrl Pts',(8.36752131451235,14.5497923702765,8.4003265416323));
#45542=CARTESIAN_POINT('',(7.68963026555311,15.,8.16025403784438));
#45543=CARTESIAN_POINT('Ctrl Pts',(8.36752131451236,14.5497923702765,8.40032654163229));
#45544=CARTESIAN_POINT('Ctrl Pts',(8.25461606994361,14.6248575891129,8.36020044943239));
#45545=CARTESIAN_POINT('Ctrl Pts',(8.14167637791574,14.6999049113629,8.32013278073115));
#45546=CARTESIAN_POINT('Ctrl Pts',(7.9157134030506,14.8499736306542,8.24010889879643));
#45547=CARTESIAN_POINT('Ctrl Pts',(7.8026878236717,14.9249965388709,8.20015189654609));
#45548=CARTESIAN_POINT('Ctrl Pts',(7.6896302655536,15.,8.16025403784399));
#45549=CARTESIAN_POINT('',(7.6896302655531,14.5669872981078,8.91025403784439));
#45550=CARTESIAN_POINT('Origin',(7.68963026555328,0.433012701891573,-17.0705080756891));
#45551=CARTESIAN_POINT('',(7.68963026555328,0.433012701891573,-17.0705080756891));
#45552=CARTESIAN_POINT('',(7.6896302655531,-0.433012701892221,-17.0705080756888));
#45553=CARTESIAN_POINT('',(7.68963026555311,0.433012701892215,-17.0705080756888));
#45554=CARTESIAN_POINT('Ctrl Pts',(7.68963026555328,0.433012701891573,-17.0705080756891));
#45555=CARTESIAN_POINT('Ctrl Pts',(7.8026887080221,0.360957848516674,-17.025501750288));
#45556=CARTESIAN_POINT('Ctrl Pts',(7.91571517126382,0.28884205082149,-16.9805081551835));
#45557=CARTESIAN_POINT('Ctrl Pts',(8.1416781451065,0.144504974615578,-16.890556773338));
#45558=CARTESIAN_POINT('Ctrl Pts',(8.25461695326464,0.0722822591086511,
-16.8455980719851));
#45559=CARTESIAN_POINT('Ctrl Pts',(8.36752131451235,-7.7715611723761E-15,
-16.8006530832646));
#45560=CARTESIAN_POINT('Ctrl Pts',(8.36752131451235,-4.44089209850063E-15,
-16.8006530832646));
#45561=CARTESIAN_POINT('Ctrl Pts',(8.25461606994312,-0.0722828246182448,
-16.8455984236178));
#45562=CARTESIAN_POINT('Ctrl Pts',(8.14167637791487,-0.144506104709167,
-16.8905574768218));
#45563=CARTESIAN_POINT('Ctrl Pts',(7.91571340305124,-0.288843179018781,
-16.9805088590736));
#45564=CARTESIAN_POINT('Ctrl Pts',(7.80268782367245,-0.360958412134893,
-17.0255021023297));
#45565=CARTESIAN_POINT('Ctrl Pts',(7.6896302655536,-0.433012701892566,-17.0705080756886));
#45566=CARTESIAN_POINT('Origin',(8.36752131451236,14.5497923702765,-8.40032654163231));
#45567=CARTESIAN_POINT('',(7.68963026555329,15.,-8.16025403784513));
#45568=CARTESIAN_POINT('Ctrl Pts',(7.68963026555329,15.,-8.16025403784513));
#45569=CARTESIAN_POINT('Ctrl Pts',(7.80268870802034,14.9249959521854,-8.20015220863258));
#45570=CARTESIAN_POINT('Ctrl Pts',(7.91571517126294,14.8499724569691,-8.24010952389882));
#45571=CARTESIAN_POINT('Ctrl Pts',(8.14167814509783,14.6999037370876,-8.32013340767562));
#45572=CARTESIAN_POINT('Ctrl Pts',(8.25461695326057,14.6248570018383,-8.36020076336009));
#45573=CARTESIAN_POINT('Ctrl Pts',(8.36752131451236,14.5497923702765,-8.40032654163231));
#45574=CARTESIAN_POINT('',(7.68963026555311,14.5669872981078,-8.91025403784439));
#45575=CARTESIAN_POINT('Ctrl Pts',(8.36752131451236,14.5497923702765,-8.40032654163231));
#45576=CARTESIAN_POINT('Ctrl Pts',(8.25461606994752,14.5525747644949,-8.4853979741823));
#45577=CARTESIAN_POINT('Ctrl Pts',(8.14167637792352,14.5553988066541,-8.57042469608449));
#45578=CARTESIAN_POINT('Ctrl Pts',(7.91571340305315,14.561130451635,-8.74039996027547));
#45579=CARTESIAN_POINT('Ctrl Pts',(7.80268782367616,14.5640381267354,-8.8253502057806));
#45580=CARTESIAN_POINT('Ctrl Pts',(7.6896302655536,14.5669872981074,-8.91025403784459));
#45581=CARTESIAN_POINT('',(7.68963026555311,15.,-8.16025403784439));
#45582=CARTESIAN_POINT('Ctrl Pts',(7.67668825215334,14.6070156607043,-8.88714365192406));
#45583=CARTESIAN_POINT('Ctrl Pts',(8.43313591503712,12.272413163364,-10.2350270322143));
#45584=CARTESIAN_POINT('Ctrl Pts',(9.03177916174122,9.05069193308572,-12.0950886517694));
#45585=CARTESIAN_POINT('Ctrl Pts',(8.82820572731108,4.69332251318476,-14.6108170593078));
#45586=CARTESIAN_POINT('Ctrl Pts',(8.18098669407586,1.94938600418923,-16.1950295414156));
#45587=CARTESIAN_POINT('Ctrl Pts',(7.67668825215334,0.392984339295657,-17.0936184616091));
#45588=CARTESIAN_POINT('Ctrl Pts',(7.90696593960635,14.5879412305617,-8.72487128182681));
#45589=CARTESIAN_POINT('Ctrl Pts',(8.67315119983517,12.2431218979784,-10.0818637214309));
#45590=CARTESIAN_POINT('Ctrl Pts',(9.28459893188896,8.99518638134712,-11.9614343524107));
#45591=CARTESIAN_POINT('Ctrl Pts',(9.07628688106433,4.59237548551847,-14.5017744624786));
#45592=CARTESIAN_POINT('Ctrl Pts',(8.41775611309223,1.82705595401861,-16.0945120758276));
#45593=CARTESIAN_POINT('Ctrl Pts',(7.90696593960635,0.261989559530435,-16.9959633354943));
#45594=CARTESIAN_POINT('Ctrl Pts',(8.13724362705935,14.5688668004191,-8.56259891172956));
#45595=CARTESIAN_POINT('Ctrl Pts',(8.91316648463323,12.2138306325927,-9.92870041064754));
#45596=CARTESIAN_POINT('Ctrl Pts',(9.5374187020367,8.93968082960853,-11.8277800530521));
#45597=CARTESIAN_POINT('Ctrl Pts',(9.32436803481757,4.49142845785217,-14.3927318656494));
#45598=CARTESIAN_POINT('Ctrl Pts',(8.6545255321086,1.70472590384799,-15.9939946102396));
#45599=CARTESIAN_POINT('Ctrl Pts',(8.13724362705935,0.130994779765213,-16.8983082093794));
#45600=CARTESIAN_POINT('Ctrl Pts',(8.36752131451236,14.5497923702765,-8.40032654163231));
#45601=CARTESIAN_POINT('Ctrl Pts',(9.15318176943128,12.1845393672071,-9.77553709986417));
#45602=CARTESIAN_POINT('Ctrl Pts',(9.79023847218445,8.88417527786995,-11.6941257536935));
#45603=CARTESIAN_POINT('Ctrl Pts',(9.57244918857082,4.39048143018587,-14.2836892688202));
#45604=CARTESIAN_POINT('Ctrl Pts',(8.89129495112497,1.58239585367736,-15.8934771446516));
#45605=CARTESIAN_POINT('Ctrl Pts',(8.36752131451235,-8.88178419700125E-15,
-16.8006530832646));
#45606=CARTESIAN_POINT('Ctrl Pts',(7.68963170841622,0.433013796132934,-17.0705074439286));
#45607=CARTESIAN_POINT('Ctrl Pts',(8.18653121623005,1.97292920995541,-16.1814368652289));
#45608=CARTESIAN_POINT('Ctrl Pts',(8.82870487706607,4.70400651959465,-14.6046486453311));
#45609=CARTESIAN_POINT('Ctrl Pts',(9.03128001198622,9.04000792667569,-12.1012570657462));
#45610=CARTESIAN_POINT('Ctrl Pts',(8.437237091211,12.2502959475146,-10.2477964127386));
#45611=CARTESIAN_POINT('Ctrl Pts',(7.68963261441509,14.5669848961069,-8.91025542464026));
#45612=CARTESIAN_POINT('Origin',(0.,14.7834936490539,-8.53525403784439));
#45613=CARTESIAN_POINT('',(0.,14.5669872981078,-8.91025403784439));
#45614=CARTESIAN_POINT('',(0.,15.,-8.16025403784439));
#45615=CARTESIAN_POINT('',(0.,14.7834936490539,-8.53525403784436));
#45616=CARTESIAN_POINT('',(0.,15.,-8.16025403784439));
#45617=CARTESIAN_POINT('',(0.,14.5669872981078,-8.91025403784439));
#45618=CARTESIAN_POINT('Ctrl Pts',(7.67668825215335,15.,8.20647480968506));
#45619=CARTESIAN_POINT('Ctrl Pts',(8.43313591503712,15.,5.5107080491046));
#45620=CARTESIAN_POINT('Ctrl Pts',(9.03209294028292,15.,1.79027110761766));
#45621=CARTESIAN_POINT('Ctrl Pts',(8.82833525724056,15.,-3.24081609633395));
#45622=CARTESIAN_POINT('Ctrl Pts',(8.18098669407586,15.,-6.4092969692981));
#45623=CARTESIAN_POINT('Ctrl Pts',(7.67668825215335,15.,-8.20647480968507));
#45624=CARTESIAN_POINT('Ctrl Pts',(7.90696593960635,14.8499307900922,8.27109205366748));
#45625=CARTESIAN_POINT('Ctrl Pts',(8.67315119983518,14.8527110492411,5.56192272456335));
#45626=CARTESIAN_POINT('Ctrl Pts',(9.2849107644129,14.856498377309,1.80901861973728));
#45627=CARTESIAN_POINT('Ctrl Pts',(9.07641678497459,14.8550928418347,-3.27371716647856));
#45628=CARTESIAN_POINT('Ctrl Pts',(8.41775611309223,14.8517842961914,-6.46497916759807));
#45629=CARTESIAN_POINT('Ctrl Pts',(7.90696593960635,14.8499307900922,-8.27109205366748));
#45630=CARTESIAN_POINT('Ctrl Pts',(8.13724362705935,14.6998615801843,8.33570929764989));
#45631=CARTESIAN_POINT('Ctrl Pts',(8.91316648463323,14.7054220984821,5.6131374000221));
#45632=CARTESIAN_POINT('Ctrl Pts',(9.53772858854289,14.7129967546181,1.82776613185691));
#45633=CARTESIAN_POINT('Ctrl Pts',(9.32449831270862,14.7101856836694,-3.30661823662315));
#45634=CARTESIAN_POINT('Ctrl Pts',(8.6545255321086,14.7035685923829,-6.52066136589804));
#45635=CARTESIAN_POINT('Ctrl Pts',(8.13724362705935,14.6998615801843,-8.3357092976499));
#45636=CARTESIAN_POINT('Ctrl Pts',(8.36752131451236,14.5497923702765,8.4003265416323));
#45637=CARTESIAN_POINT('Ctrl Pts',(9.15318176943128,14.5581331477232,5.66435207548085));
#45638=CARTESIAN_POINT('Ctrl Pts',(9.79054641267288,14.5694951319271,1.84651364397653));
#45639=CARTESIAN_POINT('Ctrl Pts',(9.57257984044265,14.565278525504,-3.33951930676775));
#45640=CARTESIAN_POINT('Ctrl Pts',(8.89129495112498,14.5553528885743,-6.57634356419801));
#45641=CARTESIAN_POINT('Ctrl Pts',(8.36752131451236,14.5497923702765,-8.40032654163231));
#45642=CARTESIAN_POINT('Ctrl Pts',(7.68963172268071,15.,-8.16025276820764));
#45643=CARTESIAN_POINT('Ctrl Pts',(8.18653232738211,15.,-6.38211114204574));
#45644=CARTESIAN_POINT('Ctrl Pts',(8.82883485876201,15.,-3.22848017464455));
#45645=CARTESIAN_POINT('Ctrl Pts',(9.03159333876146,15.,1.77793518592809));
#45646=CARTESIAN_POINT('Ctrl Pts',(8.43723924018764,15.,5.48516714116145));
#45647=CARTESIAN_POINT('Ctrl Pts',(7.68963263283691,15.,8.16025124584423));
#45648=CARTESIAN_POINT('Ctrl Pts',(7.67668825215334,-0.392984339295669,
-17.0936184616091));
#45649=CARTESIAN_POINT('Ctrl Pts',(8.43313591503712,-2.72758683663603,-15.7457350813189));
#45650=CARTESIAN_POINT('Ctrl Pts',(9.03177916174122,-5.94930806691429,-13.8856734617638));
#45651=CARTESIAN_POINT('Ctrl Pts',(8.82820572731108,-10.3066774868152,-11.3699450542253));
#45652=CARTESIAN_POINT('Ctrl Pts',(8.18098669407586,-13.0506139958108,-9.78573257211753));
#45653=CARTESIAN_POINT('Ctrl Pts',(7.67668825215334,-14.6070156607043,-8.88714365192405));
#45654=CARTESIAN_POINT('Ctrl Pts',(7.90696593960635,-0.261989559530447,
-16.9959633354943));
#45655=CARTESIAN_POINT('Ctrl Pts',(8.67315119983517,-2.60958915126271,-15.6437864459943));
#45656=CARTESIAN_POINT('Ctrl Pts',(9.28459893188896,-5.861312824214,-13.7707770942278));
#45657=CARTESIAN_POINT('Ctrl Pts',(9.07628688106433,-10.2627173416997,-11.2280010654152));
#45658=CARTESIAN_POINT('Ctrl Pts',(8.41775611309223,-13.0247283421728,-9.62953290822953));
#45659=CARTESIAN_POINT('Ctrl Pts',(7.90696593960635,-14.5879412305617,-8.7248712818268));
#45660=CARTESIAN_POINT('Ctrl Pts',(8.13724362705935,-0.130994779765225,
-16.8983082093794));
#45661=CARTESIAN_POINT('Ctrl Pts',(8.91316648463323,-2.49159146588939,-15.5418378106696));
#45662=CARTESIAN_POINT('Ctrl Pts',(9.5374187020367,-5.7733175815137,-13.6558807266918));
#45663=CARTESIAN_POINT('Ctrl Pts',(9.32436803481757,-10.2187571965841,-11.0860570766051));
#45664=CARTESIAN_POINT('Ctrl Pts',(8.6545255321086,-12.9988426885349,-9.47333324434154));
#45665=CARTESIAN_POINT('Ctrl Pts',(8.13724362705935,-14.5688668004191,-8.56259891172955));
#45666=CARTESIAN_POINT('Ctrl Pts',(8.36752131451236,-3.33066907387547E-15,
-16.8006530832646));
#45667=CARTESIAN_POINT('Ctrl Pts',(9.15318176943128,-2.37359378051606,-15.439889175345));
#45668=CARTESIAN_POINT('Ctrl Pts',(9.79023847218444,-5.6853223388134,-13.5409843591558));
#45669=CARTESIAN_POINT('Ctrl Pts',(9.57244918857082,-10.1747970514685,-10.9441130877949));
#45670=CARTESIAN_POINT('Ctrl Pts',(8.89129495112497,-12.9729570348969,-9.31713358045354));
#45671=CARTESIAN_POINT('Ctrl Pts',(8.36752131451235,-14.5497923702765,-8.4003265416323));
#45672=CARTESIAN_POINT('Ctrl Pts',(7.68963170841621,-14.5669862038671,-8.91025466960456));
#45673=CARTESIAN_POINT('Ctrl Pts',(8.18653121623004,-13.0270707900446,-9.79932524830422));
#45674=CARTESIAN_POINT('Ctrl Pts',(8.82870487706607,-10.2959934804053,-11.3761134682021));
#45675=CARTESIAN_POINT('Ctrl Pts',(9.03128001198622,-5.95999207332432,-13.8795050477869));
#45676=CARTESIAN_POINT('Ctrl Pts',(8.437237091211,-2.74970405248537,-15.7329657007945));
#45677=CARTESIAN_POINT('Ctrl Pts',(7.68963261441509,-0.433015103893123,
-17.0705066888929));
#45678=CARTESIAN_POINT('Origin',(0.,-3.01841884819964E-15,-17.0705080756888));
#45679=CARTESIAN_POINT('',(0.,-0.433012701892219,-17.0705080756888));
#45680=CARTESIAN_POINT('',(0.,0.433012701892215,-17.0705080756888));
#45681=CARTESIAN_POINT('',(0.,-2.33931761355391E-14,-17.0705080756888));
#45682=CARTESIAN_POINT('',(0.,0.433012701892215,-17.0705080756888));
#45683=CARTESIAN_POINT('',(0.,-0.433012701892221,-17.0705080756888));
#45684=CARTESIAN_POINT('Origin',(0.,14.7834936490539,8.53525403784439));
#45685=CARTESIAN_POINT('',(0.,15.,8.16025403784438));
#45686=CARTESIAN_POINT('',(0.,14.5669872981078,8.91025403784439));
#45687=CARTESIAN_POINT('',(0.,14.7834936490539,8.53525403784438));
#45688=CARTESIAN_POINT('',(0.,14.5669872981078,8.91025403784439));
#45689=CARTESIAN_POINT('',(0.,15.,8.16025403784438));
#45690=CARTESIAN_POINT('Ctrl Pts',(7.67668825215334,0.392984339295667,17.0936184616091));
#45691=CARTESIAN_POINT('Ctrl Pts',(8.43313591503712,2.72758683663604,15.7457350813189));
#45692=CARTESIAN_POINT('Ctrl Pts',(9.03177916174123,5.94930806691429,13.8856734617638));
#45693=CARTESIAN_POINT('Ctrl Pts',(8.82820572731109,10.3066774868152,11.3699450542253));
#45694=CARTESIAN_POINT('Ctrl Pts',(8.18098669407586,13.0506139958108,9.78573257211753));
#45695=CARTESIAN_POINT('Ctrl Pts',(7.67668825215334,14.6070156607043,8.88714365192404));
#45696=CARTESIAN_POINT('Ctrl Pts',(7.90696593960635,0.261989559530445,16.9959633354943));
#45697=CARTESIAN_POINT('Ctrl Pts',(8.67315119983518,2.60958915126271,15.6437864459943));
#45698=CARTESIAN_POINT('Ctrl Pts',(9.28459893188897,5.86131282421399,13.7707770942278));
#45699=CARTESIAN_POINT('Ctrl Pts',(9.07628688106433,10.2627173416997,11.2280010654152));
#45700=CARTESIAN_POINT('Ctrl Pts',(8.41775611309223,13.0247283421728,9.62953290822953));
#45701=CARTESIAN_POINT('Ctrl Pts',(7.90696593960635,14.5879412305617,8.72487128182679));
#45702=CARTESIAN_POINT('Ctrl Pts',(8.13724362705935,0.130994779765222,16.8983082093794));
#45703=CARTESIAN_POINT('Ctrl Pts',(8.91316648463323,2.49159146588939,15.5418378106696));
#45704=CARTESIAN_POINT('Ctrl Pts',(9.53741870203671,5.7733175815137,13.6558807266918));
#45705=CARTESIAN_POINT('Ctrl Pts',(9.32436803481758,10.2187571965841,11.0860570766051));
#45706=CARTESIAN_POINT('Ctrl Pts',(8.6545255321086,12.9988426885349,9.47333324434154));
#45707=CARTESIAN_POINT('Ctrl Pts',(8.13724362705935,14.5688668004191,8.56259891172954));
#45708=CARTESIAN_POINT('Ctrl Pts',(8.36752131451236,-5.55111512312578E-16,
16.8006530832646));
#45709=CARTESIAN_POINT('Ctrl Pts',(9.15318176943128,2.37359378051606,15.439889175345));
#45710=CARTESIAN_POINT('Ctrl Pts',(9.79023847218445,5.68532233881341,13.5409843591558));
#45711=CARTESIAN_POINT('Ctrl Pts',(9.57244918857082,10.1747970514685,10.9441130877949));
#45712=CARTESIAN_POINT('Ctrl Pts',(8.89129495112497,12.9729570348969,9.31713358045354));
#45713=CARTESIAN_POINT('Ctrl Pts',(8.36752131451235,14.5497923702765,8.4003265416323));
#45714=CARTESIAN_POINT('Ctrl Pts',(7.68963170841621,14.5669862038671,8.91025466960456));
#45715=CARTESIAN_POINT('Ctrl Pts',(8.18653121623005,13.0270707900446,9.79932524830422));
#45716=CARTESIAN_POINT('Ctrl Pts',(8.82870487706607,10.2959934804054,11.3761134682021));
#45717=CARTESIAN_POINT('Ctrl Pts',(9.03128001198623,5.95999207332431,13.8795050477869));
#45718=CARTESIAN_POINT('Ctrl Pts',(8.43723709121101,2.74970405248537,15.7329657007945));
#45719=CARTESIAN_POINT('Ctrl Pts',(7.68963261441509,0.43301510389312,17.0705066888929));
#45720=CARTESIAN_POINT('Ctrl Pts',(7.67668825215334,-15.,-8.20647480968506));
#45721=CARTESIAN_POINT('Ctrl Pts',(8.43313591503712,-15.,-5.5107080491046));
#45722=CARTESIAN_POINT('Ctrl Pts',(9.03209294028291,-15.,-1.79027110761766));
#45723=CARTESIAN_POINT('Ctrl Pts',(8.82833525724056,-15.,3.24081609633395));
#45724=CARTESIAN_POINT('Ctrl Pts',(8.18098669407586,-15.,6.40929696929809));
#45725=CARTESIAN_POINT('Ctrl Pts',(7.67668825215334,-15.,8.20647480968506));
#45726=CARTESIAN_POINT('Ctrl Pts',(7.90696593960635,-14.8499307900922,-8.27109205366748));
#45727=CARTESIAN_POINT('Ctrl Pts',(8.67315119983517,-14.8527110492411,-5.56192272456335));
#45728=CARTESIAN_POINT('Ctrl Pts',(9.2849107644129,-14.856498377309,-1.80901861973728));
#45729=CARTESIAN_POINT('Ctrl Pts',(9.07641678497459,-14.8550928418347,3.27371716647854));
#45730=CARTESIAN_POINT('Ctrl Pts',(8.41775611309223,-14.8517842961914,6.46497916759806));
#45731=CARTESIAN_POINT('Ctrl Pts',(7.90696593960635,-14.8499307900922,8.27109205366747));
#45732=CARTESIAN_POINT('Ctrl Pts',(8.13724362705935,-14.6998615801843,-8.33570929764989));
#45733=CARTESIAN_POINT('Ctrl Pts',(8.91316648463323,-14.7054220984821,-5.6131374000221));
#45734=CARTESIAN_POINT('Ctrl Pts',(9.53772858854288,-14.7129967546181,-1.82776613185692));
#45735=CARTESIAN_POINT('Ctrl Pts',(9.32449831270862,-14.7101856836694,3.30661823662315));
#45736=CARTESIAN_POINT('Ctrl Pts',(8.6545255321086,-14.7035685923829,6.52066136589803));
#45737=CARTESIAN_POINT('Ctrl Pts',(8.13724362705935,-14.6998615801843,8.33570929764989));
#45738=CARTESIAN_POINT('Ctrl Pts',(8.36752131451236,-14.5497923702765,-8.4003265416323));
#45739=CARTESIAN_POINT('Ctrl Pts',(9.15318176943128,-14.5581331477232,-5.66435207548086));
#45740=CARTESIAN_POINT('Ctrl Pts',(9.79054641267287,-14.5694951319271,-1.84651364397654));
#45741=CARTESIAN_POINT('Ctrl Pts',(9.57257984044265,-14.5652785255041,3.33951930676774));
#45742=CARTESIAN_POINT('Ctrl Pts',(8.89129495112497,-14.5553528885743,6.576343564198));
#45743=CARTESIAN_POINT('Ctrl Pts',(8.36752131451236,-14.5497923702765,8.4003265416323));
#45744=CARTESIAN_POINT('Ctrl Pts',(7.6896317226807,-15.,8.16025276820764));
#45745=CARTESIAN_POINT('Ctrl Pts',(8.1865323273821,-15.,6.38211114204573));
#45746=CARTESIAN_POINT('Ctrl Pts',(8.828834858762,-15.,3.22848017464454));
#45747=CARTESIAN_POINT('Ctrl Pts',(9.03159333876145,-15.,-1.77793518592809));
#45748=CARTESIAN_POINT('Ctrl Pts',(8.43723924018764,-15.,-5.48516714116146));
#45749=CARTESIAN_POINT('Ctrl Pts',(7.68963263283691,-15.,-8.16025124584424));
#45750=CARTESIAN_POINT('Origin',(0.,-14.7834936490539,-8.53525403784439));
#45751=CARTESIAN_POINT('',(0.,-15.,-8.16025403784439));
#45752=CARTESIAN_POINT('',(0.,-14.5669872981078,-8.91025403784439));
#45753=CARTESIAN_POINT('',(0.,-14.7834936490539,-8.53525403784438));
#45754=CARTESIAN_POINT('',(0.,-14.5669872981078,-8.91025403784439));
#45755=CARTESIAN_POINT('',(0.,-15.,-8.16025403784439));
#45756=CARTESIAN_POINT('Origin',(0.,4.16333634234434E-16,17.0705080756888));
#45757=CARTESIAN_POINT('',(0.,0.433012701892219,17.0705080756888));
#45758=CARTESIAN_POINT('',(0.,-0.43301270189222,17.0705080756888));
#45759=CARTESIAN_POINT('',(0.,-2.1675799894322E-14,17.0705080756888));
#45760=CARTESIAN_POINT('',(0.,-0.43301270189222,17.0705080756888));
#45761=CARTESIAN_POINT('',(0.,0.43301270189222,17.0705080756888));
#45762=CARTESIAN_POINT('Ctrl Pts',(7.67668825215334,-14.6070156607043,8.88714365192404));
#45763=CARTESIAN_POINT('Ctrl Pts',(8.43313591503712,-12.272413163364,10.2350270322143));
#45764=CARTESIAN_POINT('Ctrl Pts',(9.03177916174123,-9.05069193308572,12.0950886517694));
#45765=CARTESIAN_POINT('Ctrl Pts',(8.82820572731109,-4.69332251318478,14.6108170593078));
#45766=CARTESIAN_POINT('Ctrl Pts',(8.18098669407586,-1.94938600418924,16.1950295414156));
#45767=CARTESIAN_POINT('Ctrl Pts',(7.67668825215334,-0.392984339295662,
17.0936184616091));
#45768=CARTESIAN_POINT('Ctrl Pts',(7.90696593960635,-14.5879412305617,8.7248712818268));
#45769=CARTESIAN_POINT('Ctrl Pts',(8.67315119983517,-12.2431218979784,10.0818637214309));
#45770=CARTESIAN_POINT('Ctrl Pts',(9.28459893188897,-8.99518638134712,11.9614343524107));
#45771=CARTESIAN_POINT('Ctrl Pts',(9.07628688106433,-4.59237548551848,14.5017744624786));
#45772=CARTESIAN_POINT('Ctrl Pts',(8.41775611309223,-1.82705595401862,16.0945120758276));
#45773=CARTESIAN_POINT('Ctrl Pts',(7.90696593960635,-0.26198955953044,16.9959633354943));
#45774=CARTESIAN_POINT('Ctrl Pts',(8.13724362705935,-14.5688668004191,8.56259891172955));
#45775=CARTESIAN_POINT('Ctrl Pts',(8.91316648463323,-12.2138306325927,9.92870041064753));
#45776=CARTESIAN_POINT('Ctrl Pts',(9.53741870203671,-8.93968082960854,11.8277800530521));
#45777=CARTESIAN_POINT('Ctrl Pts',(9.32436803481758,-4.49142845785218,14.3927318656494));
#45778=CARTESIAN_POINT('Ctrl Pts',(8.6545255321086,-1.704725903848,15.9939946102396));
#45779=CARTESIAN_POINT('Ctrl Pts',(8.13724362705935,-0.130994779765218,
16.8983082093794));
#45780=CARTESIAN_POINT('Ctrl Pts',(8.36752131451235,-14.5497923702765,8.4003265416323));
#45781=CARTESIAN_POINT('Ctrl Pts',(9.15318176943129,-12.1845393672071,9.77553709986416));
#45782=CARTESIAN_POINT('Ctrl Pts',(9.79023847218445,-8.88417527786995,11.6941257536935));
#45783=CARTESIAN_POINT('Ctrl Pts',(9.57244918857083,-4.39048143018589,14.2836892688202));
#45784=CARTESIAN_POINT('Ctrl Pts',(8.89129495112497,-1.58239585367737,15.8934771446515));
#45785=CARTESIAN_POINT('Ctrl Pts',(8.36752131451235,4.44089209850063E-15,
16.8006530832646));
#45786=CARTESIAN_POINT('Ctrl Pts',(7.68963170841622,-0.433013796132936,
17.0705074439286));
#45787=CARTESIAN_POINT('Ctrl Pts',(8.18653121623005,-1.97292920995542,16.1814368652289));
#45788=CARTESIAN_POINT('Ctrl Pts',(8.82870487706608,-4.70400651959466,14.604648645331));
#45789=CARTESIAN_POINT('Ctrl Pts',(9.03128001198623,-9.04000792667568,12.1012570657462));
#45790=CARTESIAN_POINT('Ctrl Pts',(8.437237091211,-12.2502959475146,10.2477964127386));
#45791=CARTESIAN_POINT('Ctrl Pts',(7.68963261441509,-14.5669848961069,8.91025542464025));
#45792=CARTESIAN_POINT('Origin',(0.,-14.7834936490539,8.53525403784439));
#45793=CARTESIAN_POINT('',(0.,-14.5669872981078,8.91025403784439));
#45794=CARTESIAN_POINT('',(0.,-15.,8.16025403784439));
#45795=CARTESIAN_POINT('',(0.,-14.7834936490539,8.5352540378444));
#45796=CARTESIAN_POINT('',(0.,-15.,8.16025403784439));
#45797=CARTESIAN_POINT('',(0.,-14.5669872981078,8.91025403784439));
#45798=CARTESIAN_POINT('Origin',(0.,0.,0.));
#45799=CARTESIAN_POINT('',(1.11022302462516E-15,-1.14252408577115,-16.6608714872132));
#45800=CARTESIAN_POINT('',(0.,-15.,-8.66025403784439));
#45801=CARTESIAN_POINT('',(1.11022302462516E-15,1.14252408577115,-16.6608714872132));
#45802=CARTESIAN_POINT('Origin',(0.,0.,0.));
#45803=CARTESIAN_POINT('',(0.,-3.18172571617472E-15,-17.3205080756888));
#45804=CARTESIAN_POINT('Origin',(0.,-15.,-8.66025403784439));
#45805=CARTESIAN_POINT('',(1.11022302462516E-15,-13.8574759142288,-9.31989062632));
#45806=CARTESIAN_POINT('',(0.,-15.,-8.66025403784439));
#45807=CARTESIAN_POINT('',(0.,-11.25,-10.8253175473055));
#45808=CARTESIAN_POINT('Origin',(0.,0.,0.));
#45809=CARTESIAN_POINT('',(1.11022302462516E-15,-15.,-7.34098086089318));
#45810=CARTESIAN_POINT('',(0.,-15.,8.66025403784439));
#45811=CARTESIAN_POINT('Origin',(0.,0.,0.));
#45812=CARTESIAN_POINT('Origin',(0.,-15.,8.66025403784439));
#45813=CARTESIAN_POINT('',(1.11022302462516E-15,-15.,7.34098086089317));
#45814=CARTESIAN_POINT('',(0.,-15.,8.66025403784439));
#45815=CARTESIAN_POINT('',(0.,-15.,4.33012701892219));
#45816=CARTESIAN_POINT('Origin',(0.,0.,0.));
#45817=CARTESIAN_POINT('',(1.11022302462516E-15,-13.8574759142288,9.31989062631999));
#45818=CARTESIAN_POINT('',(0.,1.06057523872491E-15,17.3205080756888));
#45819=CARTESIAN_POINT('Origin',(0.,0.,0.));
#45820=CARTESIAN_POINT('Origin',(0.,1.06057523872491E-15,17.3205080756888));
#45821=CARTESIAN_POINT('',(1.11022302462516E-15,-1.14252408577115,16.6608714872132));
#45822=CARTESIAN_POINT('',(0.,1.06057523872491E-15,17.3205080756888));
#45823=CARTESIAN_POINT('',(0.,-3.75,15.1554445662277));
#45824=CARTESIAN_POINT('Origin',(0.,15.,8.66025403784439));
#45825=CARTESIAN_POINT('',(1.11022302462516E-15,13.8574759142288,9.31989062631999));
#45826=CARTESIAN_POINT('',(0.,15.,8.66025403784439));
#45827=CARTESIAN_POINT('',(1.11022302462516E-15,1.14252408577115,16.6608714872132));
#45828=CARTESIAN_POINT('',(0.,11.25,10.8253175473055));
#45829=CARTESIAN_POINT('',(0.,15.,8.66025403784439));
#45830=CARTESIAN_POINT('Origin',(0.,15.,-8.66025403784439));
#45831=CARTESIAN_POINT('',(1.11022302462516E-15,15.,-7.34098086089319));
#45832=CARTESIAN_POINT('',(0.,15.,-8.66025403784439));
#45833=CARTESIAN_POINT('',(1.11022302462516E-15,15.,7.34098086089318));
#45834=CARTESIAN_POINT('',(0.,15.,-4.3301270189222));
#45835=CARTESIAN_POINT('',(0.,15.,-8.66025403784439));
#45836=CARTESIAN_POINT('Origin',(0.,0.,0.));
#45837=CARTESIAN_POINT('',(1.11022302462516E-15,13.8574759142288,-9.31989062632));
#45838=CARTESIAN_POINT('',(0.,-3.18172571617472E-15,-17.3205080756888));
#45839=CARTESIAN_POINT('Origin',(0.,0.,0.));
#45840=CARTESIAN_POINT('Origin',(0.,0.,0.));
#45841=CARTESIAN_POINT('Origin',(0.,0.,0.));
#45842=CARTESIAN_POINT('Origin',(0.,0.,0.));
#45843=CARTESIAN_POINT('Origin',(0.,0.,0.));
#45844=CARTESIAN_POINT('Origin',(0.,-3.18172571617472E-15,-17.3205080756888));
#45845=CARTESIAN_POINT('',(0.,3.75,-15.1554445662277));
#45846=CARTESIAN_POINT('Origin',(0.,0.,0.));
#45847=CARTESIAN_POINT('Origin',(0.,0.,0.));
#45848=CARTESIAN_POINT('Origin',(0.,0.,0.));
#45849=CARTESIAN_POINT('Origin',(0.,0.,0.));
#45850=CARTESIAN_POINT('Origin',(0.,0.,0.));
#45851=CARTESIAN_POINT('Origin',(0.,0.,0.));
#45852=CARTESIAN_POINT('Origin',(0.,0.,0.));
#45853=CARTESIAN_POINT('Origin',(0.,0.,0.));
#45854=CARTESIAN_POINT('Origin',(0.,0.,0.));
#45855=CARTESIAN_POINT('Origin',(0.,0.,0.));
#45856=CARTESIAN_POINT('Origin',(0.,0.,0.));
#45857=CARTESIAN_POINT('',(1.11022302462516E-15,-16.7,-2.04516015457608E-15));
#45858=CARTESIAN_POINT('Origin',(0.,0.,0.));
#45859=CARTESIAN_POINT('Origin',(0.,0.,0.));
#45860=CARTESIAN_POINT('Origin',(-18.,16.2,0.));
#45861=CARTESIAN_POINT('',(-18.,-16.2,-1.98392781461871E-15));
#45862=CARTESIAN_POINT('Origin',(-18.,0.,0.));
#45863=CARTESIAN_POINT('Origin',(-17.75,0.,0.));
#45864=CARTESIAN_POINT('',(-17.5,-16.7,-2.04516015457608E-15));
#45865=CARTESIAN_POINT('Origin',(-17.5,0.,0.));
#45866=CARTESIAN_POINT('',(-17.75,-16.45,-2.0145439845974E-15));
#45867=CARTESIAN_POINT('Origin',(-8.75,0.,0.));
#45868=CARTESIAN_POINT('',(-8.75,-16.7,-2.04516015457608E-15));
#45869=CARTESIAN_POINT('',(0.,0.,0.));
#45870=CARTESIAN_POINT('Origin',(-56.4,179.5,-41.9));
#45871=CARTESIAN_POINT('',(-56.3,142.,-42.));
#45872=CARTESIAN_POINT('',(-56.5,142.,-41.8));
#45873=CARTESIAN_POINT('',(-56.3,142.,-42.));
#45874=CARTESIAN_POINT('',(-56.5,192.,-41.8));
#45875=CARTESIAN_POINT('',(-56.5,179.5,-41.8));
#45876=CARTESIAN_POINT('',(-56.3,192.,-42.));
#45877=CARTESIAN_POINT('',(-56.5,192.,-41.8));
#45878=CARTESIAN_POINT('',(-56.3,179.5,-42.));
#45879=CARTESIAN_POINT('Origin',(-56.4,142.,-37.));
#45880=CARTESIAN_POINT('',(-56.3,137.,-37.));
#45881=CARTESIAN_POINT('',(-56.5,137.2,-37.));
#45882=CARTESIAN_POINT('',(-56.3,137.,-37.));
#45883=CARTESIAN_POINT('Origin',(-56.5,142.,-37.));
#45884=CARTESIAN_POINT('Origin',(-56.3,142.,-37.));
#45885=CARTESIAN_POINT('Origin',(-56.4,137.1,-18.5));
#45886=CARTESIAN_POINT('',(-56.3,137.,37.));
#45887=CARTESIAN_POINT('',(-56.5,137.2,37.));
#45888=CARTESIAN_POINT('',(-56.3,137.,37.));
#45889=CARTESIAN_POINT('',(-56.5,137.2,-18.5));
#45890=CARTESIAN_POINT('',(-56.3,137.,-18.5));
#45891=CARTESIAN_POINT('Origin',(-56.4,142.,37.));
#45892=CARTESIAN_POINT('',(-56.3,142.,42.));
#45893=CARTESIAN_POINT('',(-56.5,142.,41.8));
#45894=CARTESIAN_POINT('',(-56.3,142.,42.));
#45895=CARTESIAN_POINT('Origin',(-56.5,142.,37.));
#45896=CARTESIAN_POINT('Origin',(-56.3,142.,37.));
#45897=CARTESIAN_POINT('Origin',(-56.4,154.5,41.9));
#45898=CARTESIAN_POINT('',(-56.3,192.,42.));
#45899=CARTESIAN_POINT('',(-56.5,192.,41.8));
#45900=CARTESIAN_POINT('',(-56.3,192.,42.));
#45901=CARTESIAN_POINT('',(-56.5,154.5,41.8));
#45902=CARTESIAN_POINT('',(-56.3,154.5,42.));
#45903=CARTESIAN_POINT('Origin',(-56.4,192.,37.));
#45904=CARTESIAN_POINT('',(-56.3,197.,37.));
#45905=CARTESIAN_POINT('',(-56.5,196.8,37.));
#45906=CARTESIAN_POINT('',(-56.3,197.,37.));
#45907=CARTESIAN_POINT('Origin',(-56.5,192.,37.));
#45908=CARTESIAN_POINT('Origin',(-56.3,192.,37.));
#45909=CARTESIAN_POINT('Origin',(-56.4,196.9,18.5));
#45910=CARTESIAN_POINT('',(-56.3,197.,-37.));
#45911=CARTESIAN_POINT('',(-56.5,196.8,-37.));
#45912=CARTESIAN_POINT('',(-56.3,197.,-37.));
#45913=CARTESIAN_POINT('',(-56.5,196.8,18.5));
#45914=CARTESIAN_POINT('',(-56.3,197.,18.5));
#45915=CARTESIAN_POINT('Origin',(-56.4,192.,-37.));
#45916=CARTESIAN_POINT('Origin',(-56.5,192.,-37.));
#45917=CARTESIAN_POINT('Origin',(-56.3,192.,-37.));
#45918=CARTESIAN_POINT('Origin',(-55.,142.,37.));
#45919=CARTESIAN_POINT('',(-55.2,137.,37.));
#45920=CARTESIAN_POINT('',(-55.,137.,37.));
#45921=CARTESIAN_POINT('',(-55.2,142.,42.));
#45922=CARTESIAN_POINT('Origin',(-55.2,142.,37.));
#45923=CARTESIAN_POINT('',(-55.,142.,42.));
#45924=CARTESIAN_POINT('Origin',(-55.,137.,-37.));
#45925=CARTESIAN_POINT('',(-55.2,137.,-37.));
#45926=CARTESIAN_POINT('',(-55.,137.,-37.));
#45927=CARTESIAN_POINT('',(-55.2,137.,-18.5));
#45928=CARTESIAN_POINT('Origin',(-55.,142.,-37.));
#45929=CARTESIAN_POINT('',(-55.2,142.,-42.));
#45930=CARTESIAN_POINT('',(-55.,142.,-42.));
#45931=CARTESIAN_POINT('Origin',(-55.2,142.,-37.));
#45932=CARTESIAN_POINT('Origin',(-55.,192.,-42.));
#45933=CARTESIAN_POINT('',(-55.2,192.,-42.));
#45934=CARTESIAN_POINT('',(-55.,192.,-42.));
#45935=CARTESIAN_POINT('',(-55.2,179.5,-42.));
#45936=CARTESIAN_POINT('Origin',(-56.5,167.,8.88178419700125E-15));
#45937=CARTESIAN_POINT('',(-56.5,193.,40.75));
#45938=CARTESIAN_POINT('Origin',(-56.5,193.,38.));
#45939=CARTESIAN_POINT('',(-56.5,141.,-35.25));
#45940=CARTESIAN_POINT('Origin',(-56.5,141.,-38.));
#45941=CARTESIAN_POINT('',(-56.5,141.,40.75));
#45942=CARTESIAN_POINT('Origin',(-56.5,141.,38.));
#45943=CARTESIAN_POINT('',(-56.5,193.,-35.25));
#45944=CARTESIAN_POINT('Origin',(-56.5,193.,-38.));
#45945=CARTESIAN_POINT('',(-56.5,151.,-30.));
#45946=CARTESIAN_POINT('',(-56.5,183.,-30.));
#45947=CARTESIAN_POINT('',(-56.5,175.,-30.));
#45948=CARTESIAN_POINT('',(-56.5,187.,-26.));
#45949=CARTESIAN_POINT('Origin',(-56.5,183.,-26.));
#45950=CARTESIAN_POINT('',(-56.5,187.,26.));
#45951=CARTESIAN_POINT('',(-56.5,187.,13.));
#45952=CARTESIAN_POINT('',(-56.5,183.,30.));
#45953=CARTESIAN_POINT('Origin',(-56.5,183.,26.));
#45954=CARTESIAN_POINT('',(-56.5,151.,30.));
#45955=CARTESIAN_POINT('',(-56.5,159.,30.));
#45956=CARTESIAN_POINT('',(-56.5,147.,26.));
#45957=CARTESIAN_POINT('Origin',(-56.5,151.,26.));
#45958=CARTESIAN_POINT('',(-56.5,147.,-26.));
#45959=CARTESIAN_POINT('',(-56.5,147.,-13.));
#45960=CARTESIAN_POINT('Origin',(-56.5,151.,-26.));
#45961=CARTESIAN_POINT('Origin',(-55.1,179.5,-41.9));
#45962=CARTESIAN_POINT('',(-55.,192.,-41.8));
#45963=CARTESIAN_POINT('',(-55.2,192.,-42.));
#45964=CARTESIAN_POINT('',(-55.,142.,-41.8));
#45965=CARTESIAN_POINT('',(-55.,179.5,-41.8));
#45966=CARTESIAN_POINT('',(-55.,142.,-41.8));
#45967=CARTESIAN_POINT('Origin',(-55.1,192.,-37.));
#45968=CARTESIAN_POINT('',(-55.2,197.,-37.));
#45969=CARTESIAN_POINT('',(-55.,196.8,-37.));
#45970=CARTESIAN_POINT('',(-55.2,197.,-37.));
#45971=CARTESIAN_POINT('Origin',(-55.,192.,-37.));
#45972=CARTESIAN_POINT('Origin',(-55.2,192.,-37.));
#45973=CARTESIAN_POINT('Origin',(-55.1,196.9,18.5));
#45974=CARTESIAN_POINT('',(-55.2,197.,37.));
#45975=CARTESIAN_POINT('',(-55.,196.8,37.));
#45976=CARTESIAN_POINT('',(-55.2,197.,37.));
#45977=CARTESIAN_POINT('',(-55.,196.8,18.5));
#45978=CARTESIAN_POINT('',(-55.2,197.,18.5));
#45979=CARTESIAN_POINT('Origin',(-55.1,192.,37.));
#45980=CARTESIAN_POINT('',(-55.2,192.,42.));
#45981=CARTESIAN_POINT('',(-55.,192.,41.8));
#45982=CARTESIAN_POINT('',(-55.2,192.,42.));
#45983=CARTESIAN_POINT('Origin',(-55.,192.,37.));
#45984=CARTESIAN_POINT('Origin',(-55.2,192.,37.));
#45985=CARTESIAN_POINT('Origin',(-55.1,154.5,41.9));
#45986=CARTESIAN_POINT('',(-55.,142.,41.8));
#45987=CARTESIAN_POINT('',(-55.2,142.,42.));
#45988=CARTESIAN_POINT('',(-55.,154.5,41.8));
#45989=CARTESIAN_POINT('',(-55.2,154.5,42.));
#45990=CARTESIAN_POINT('Origin',(-55.1,142.,37.));
#45991=CARTESIAN_POINT('',(-55.,137.2,37.));
#45992=CARTESIAN_POINT('',(-55.2,137.,37.));
#45993=CARTESIAN_POINT('Origin',(-55.,142.,37.));
#45994=CARTESIAN_POINT('Origin',(-55.1,137.1,-18.5));
#45995=CARTESIAN_POINT('',(-55.,137.2,-37.));
#45996=CARTESIAN_POINT('',(-55.2,137.,-37.));
#45997=CARTESIAN_POINT('',(-55.,137.2,-18.5));
#45998=CARTESIAN_POINT('Origin',(-55.1,142.,-37.));
#45999=CARTESIAN_POINT('Origin',(-55.,142.,-37.));
#46000=CARTESIAN_POINT('Origin',(-55.,192.,37.));
#46001=CARTESIAN_POINT('',(-55.,192.,42.));
#46002=CARTESIAN_POINT('',(-55.,197.,37.));
#46003=CARTESIAN_POINT('Origin',(-55.,197.,37.));
#46004=CARTESIAN_POINT('',(-55.,197.,-37.));
#46005=CARTESIAN_POINT('Origin',(-55.,192.,-37.));
#46006=CARTESIAN_POINT('Origin',(-55.,167.,8.88178419700125E-15));
#46007=CARTESIAN_POINT('',(-55.,193.,40.75));
#46008=CARTESIAN_POINT('Origin',(-55.,193.,38.));
#46009=CARTESIAN_POINT('',(-55.,141.,-35.25));
#46010=CARTESIAN_POINT('Origin',(-55.,141.,-38.));
#46011=CARTESIAN_POINT('',(-55.,141.,40.75));
#46012=CARTESIAN_POINT('Origin',(-55.,141.,38.));
#46013=CARTESIAN_POINT('',(-55.,193.,-35.25));
#46014=CARTESIAN_POINT('Origin',(-55.,193.,-38.));
#46015=CARTESIAN_POINT('Origin',(-57.,175.,-29.9));
#46016=CARTESIAN_POINT('',(-56.9,151.,-30.));
#46017=CARTESIAN_POINT('',(-57.1,151.,-29.8));
#46018=CARTESIAN_POINT('',(-56.9,151.,-30.));
#46019=CARTESIAN_POINT('',(-57.1,183.,-29.8));
#46020=CARTESIAN_POINT('',(-57.1,175.,-29.8));
#46021=CARTESIAN_POINT('',(-56.9,183.,-30.));
#46022=CARTESIAN_POINT('',(-57.1,183.,-29.8));
#46023=CARTESIAN_POINT('',(-56.9,175.,-30.));
#46024=CARTESIAN_POINT('Origin',(-57.,151.,-26.));
#46025=CARTESIAN_POINT('',(-56.9,147.,-26.));
#46026=CARTESIAN_POINT('',(-57.1,147.2,-26.));
#46027=CARTESIAN_POINT('',(-56.9,147.,-26.));
#46028=CARTESIAN_POINT('Origin',(-57.1,151.,-26.));
#46029=CARTESIAN_POINT('Origin',(-56.9,151.,-26.));
#46030=CARTESIAN_POINT('Origin',(-57.,147.1,-13.));
#46031=CARTESIAN_POINT('',(-56.9,147.,26.));
#46032=CARTESIAN_POINT('',(-57.1,147.2,26.));
#46033=CARTESIAN_POINT('',(-56.9,147.,26.));
#46034=CARTESIAN_POINT('',(-57.1,147.2,-13.));
#46035=CARTESIAN_POINT('',(-56.9,147.,-13.));
#46036=CARTESIAN_POINT('Origin',(-57.,151.,26.));
#46037=CARTESIAN_POINT('',(-56.9,151.,30.));
#46038=CARTESIAN_POINT('',(-57.1,151.,29.8));
#46039=CARTESIAN_POINT('',(-56.9,151.,30.));
#46040=CARTESIAN_POINT('Origin',(-57.1,151.,26.));
#46041=CARTESIAN_POINT('Origin',(-56.9,151.,26.));
#46042=CARTESIAN_POINT('Origin',(-57.,159.,29.9));
#46043=CARTESIAN_POINT('',(-56.9,183.,30.));
#46044=CARTESIAN_POINT('',(-57.1,183.,29.8));
#46045=CARTESIAN_POINT('',(-56.9,183.,30.));
#46046=CARTESIAN_POINT('',(-57.1,159.,29.8));
#46047=CARTESIAN_POINT('',(-56.9,159.,30.));
#46048=CARTESIAN_POINT('Origin',(-57.,183.,26.));
#46049=CARTESIAN_POINT('',(-56.9,187.,26.));
#46050=CARTESIAN_POINT('',(-57.1,186.8,26.));
#46051=CARTESIAN_POINT('',(-56.9,187.,26.));
#46052=CARTESIAN_POINT('Origin',(-57.1,183.,26.));
#46053=CARTESIAN_POINT('Origin',(-56.9,183.,26.));
#46054=CARTESIAN_POINT('Origin',(-57.,186.9,13.));
#46055=CARTESIAN_POINT('',(-56.9,187.,-26.));
#46056=CARTESIAN_POINT('',(-57.1,186.8,-26.));
#46057=CARTESIAN_POINT('',(-56.9,187.,-26.));
#46058=CARTESIAN_POINT('',(-57.1,186.8,13.));
#46059=CARTESIAN_POINT('',(-56.9,187.,13.));
#46060=CARTESIAN_POINT('Origin',(-57.,183.,-26.));
#46061=CARTESIAN_POINT('Origin',(-57.1,183.,-26.));
#46062=CARTESIAN_POINT('Origin',(-56.9,183.,-26.));
#46063=CARTESIAN_POINT('Origin',(-56.5,151.,26.));
#46064=CARTESIAN_POINT('',(-56.5,147.,26.));
#46065=CARTESIAN_POINT('',(-56.5,151.,30.));
#46066=CARTESIAN_POINT('Origin',(-56.5,147.,-26.));
#46067=CARTESIAN_POINT('',(-56.5,147.,-26.));
#46068=CARTESIAN_POINT('Origin',(-56.5,151.,-26.));
#46069=CARTESIAN_POINT('',(-56.5,151.,-30.));
#46070=CARTESIAN_POINT('Origin',(-56.5,183.,-30.));
#46071=CARTESIAN_POINT('',(-56.5,183.,-30.));
#46072=CARTESIAN_POINT('Origin',(-57.1,167.,0.));
#46073=CARTESIAN_POINT('Origin',(-56.5,183.,-26.));
#46074=CARTESIAN_POINT('',(-56.5,187.,-26.));
#46075=CARTESIAN_POINT('Origin',(-56.5,187.,26.));
#46076=CARTESIAN_POINT('',(-56.5,187.,26.));
#46077=CARTESIAN_POINT('Origin',(-56.5,183.,26.));
#46078=CARTESIAN_POINT('',(-56.5,183.,30.));
#46079=CARTESIAN_POINT('Origin',(-56.5,151.,30.));
#46080=CARTESIAN_POINT('Origin',(-55.,193.,-38.));
#46081=CARTESIAN_POINT('',(-55.,193.,-35.25));
#46082=CARTESIAN_POINT('Origin',(-55.,141.,38.));
#46083=CARTESIAN_POINT('',(-55.,141.,40.75));
#46084=CARTESIAN_POINT('Origin',(-55.,141.,-38.));
#46085=CARTESIAN_POINT('',(-55.,141.,-35.25));
#46086=CARTESIAN_POINT('Origin',(-55.,193.,38.));
#46087=CARTESIAN_POINT('',(-55.,193.,40.75));
#46088=CARTESIAN_POINT('Origin',(-55.,142.,42.));
#46089=CARTESIAN_POINT('',(0.,0.,0.));
#46090=CARTESIAN_POINT('Origin',(189.823223304703,0.,-7.45612530191356E-16));
#46091=CARTESIAN_POINT('',(190.,-17.6605334048044,15.5034047827497));
#46092=CARTESIAN_POINT('',(189.646446609407,-18.2099328514786,16.170773274433));
#46093=CARTESIAN_POINT('Ctrl Pts',(189.646446609407,-18.2099328514786,16.1707732744329));
#46094=CARTESIAN_POINT('Ctrl Pts',(189.826457221484,-17.9303333695711,15.8311371760613));
#46095=CARTESIAN_POINT('Ctrl Pts',(190.,-17.6605334048044,15.5034047827497));
#46096=CARTESIAN_POINT('',(189.646446609407,-24.3535533905933,-2.98245012076542E-15));
#46097=CARTESIAN_POINT('Origin',(189.646446609407,0.,-1.49122506038271E-15));
#46098=CARTESIAN_POINT('',(189.646446609407,-18.2099328514786,-16.170773274433));
#46099=CARTESIAN_POINT('Origin',(189.646446609407,0.,-1.49122506038271E-15));
#46100=CARTESIAN_POINT('',(190.,-17.6605334048044,-15.5034047827497));
#46101=CARTESIAN_POINT('Ctrl Pts',(190.,-17.6605334048045,-15.5034047827498));
#46102=CARTESIAN_POINT('Ctrl Pts',(189.826457222012,-17.9303333687502,-15.831137175064));
#46103=CARTESIAN_POINT('Ctrl Pts',(189.646446609407,-18.2099328514788,-16.1707732744332));
#46104=CARTESIAN_POINT('Origin',(190.,0.,0.));
#46105=CARTESIAN_POINT('Origin',(189.5,0.,0.));
#46106=CARTESIAN_POINT('',(190.,-17.9824248820024,-15.8944139672761));
#46107=CARTESIAN_POINT('Ctrl Pts',(189.646446609407,-18.2099328514786,-16.170773274433));
#46108=CARTESIAN_POINT('Ctrl Pts',(189.824548278075,-18.0953471159447,-16.0315832735063));
#46109=CARTESIAN_POINT('Ctrl Pts',(190.,-17.9824248820024,-15.8944139672761));
#46110=CARTESIAN_POINT('',(189.353553390593,-24.6464466094067,-3.01831919505661E-15));
#46111=CARTESIAN_POINT('',(189.5,-24.5,-3.00038465791102E-15));
#46112=CARTESIAN_POINT('',(189.353553390593,24.6464466094067,-3.01831919505661E-15));
#46113=CARTESIAN_POINT('Origin',(189.353553390593,0.,-1.5091595975283E-15));
#46114=CARTESIAN_POINT('Origin',(189.353553390593,0.,-1.5091595975283E-15));
#46115=CARTESIAN_POINT('',(190.,-17.9824248820024,15.8944139672761));
#46116=CARTESIAN_POINT('Ctrl Pts',(190.,-17.9824248820024,15.8944139672761));
#46117=CARTESIAN_POINT('Ctrl Pts',(189.824548278098,-18.0953471159299,16.0315832734883));
#46118=CARTESIAN_POINT('Ctrl Pts',(189.646446609407,-18.2099328514786,16.170773274433));
#46119=CARTESIAN_POINT('',(190.5,-17.6605334048044,15.5034047827497));
#46120=CARTESIAN_POINT('Ctrl Pts',(190.,-17.9824248820024,15.8944139672761));
#46121=CARTESIAN_POINT('Ctrl Pts',(190.252700024269,-17.8197849777336,15.6968514319361));
#46122=CARTESIAN_POINT('Ctrl Pts',(190.5,-17.6605334048044,15.5034047827497));
#46123=CARTESIAN_POINT('',(190.,-17.6436771757118,16.2696237116679));
#46124=CARTESIAN_POINT('Ctrl Pts',(190.499999999993,-17.6605334048042,15.5034047827607));
#46125=CARTESIAN_POINT('Ctrl Pts',(190.253091651642,-17.65449217735,15.8845492841333));
#46126=CARTESIAN_POINT('Ctrl Pts',(190.,-17.6436771757118,16.2696237116679));
#46127=CARTESIAN_POINT('',(190.,-4.77375383292611,23.5204437530975));
#46128=CARTESIAN_POINT('Origin',(190.,0.,0.));
#46129=CARTESIAN_POINT('',(189.646446609407,-4.89933402875813,23.8556510878058));
#46130=CARTESIAN_POINT('Ctrl Pts',(189.646446609407,-4.89933402875813,23.8556510878058));
#46131=CARTESIAN_POINT('Ctrl Pts',(189.82454827809,-4.83608481976441,23.6868219294443));
#46132=CARTESIAN_POINT('Ctrl Pts',(190.,-4.77375383292611,23.5204437530975));
#46133=CARTESIAN_POINT('',(189.646446609407,23.1092668802368,7.68487781337279));
#46134=CARTESIAN_POINT('Origin',(189.646446609407,0.,-1.49122506038271E-15));
#46135=CARTESIAN_POINT('',(190.,22.7561787149285,7.62602978582142));
#46136=CARTESIAN_POINT('Ctrl Pts',(190.,22.7561787149285,7.62602978582142));
#46137=CARTESIAN_POINT('Ctrl Pts',(189.824548278069,22.9314319357209,7.65523865595349));
#46138=CARTESIAN_POINT('Ctrl Pts',(189.646446609407,23.1092668802368,7.68487781337279));
#46139=CARTESIAN_POINT('',(190.5,22.2566090894166,7.54276818156944));
#46140=CARTESIAN_POINT('Ctrl Pts',(190.,22.7561787149285,7.62602978582142));
#46141=CARTESIAN_POINT('Ctrl Pts',(190.252700024268,22.5037645883542,7.58396076472571));
#46142=CARTESIAN_POINT('Ctrl Pts',(190.5,22.2566090894167,7.54276818156944));
#46143=CARTESIAN_POINT('',(190.,22.911746032174,7.14506079450414));
#46144=CARTESIAN_POINT('Ctrl Pts',(190.499999999993,22.2566090894261,7.5427681815638));
#46145=CARTESIAN_POINT('Ctrl Pts',(190.253091651642,22.5836692964003,7.34696407443207));
#46146=CARTESIAN_POINT('Ctrl Pts',(190.,22.911746032174,7.14506079450414));
#46147=CARTESIAN_POINT('',(190.,22.911746032174,-7.14506079450414));
#46148=CARTESIAN_POINT('Origin',(190.,0.,0.));
#46149=CARTESIAN_POINT('',(190.5,22.2566090894166,-7.54276818156944));
#46150=CARTESIAN_POINT('Ctrl Pts',(190.,22.911746032174,-7.14506079450415));
#46151=CARTESIAN_POINT('Ctrl Pts',(190.253091651653,22.5836692963867,-7.34696407444047));
#46152=CARTESIAN_POINT('Ctrl Pts',(190.500000000013,22.2566090893989,-7.54276818158009));
#46153=CARTESIAN_POINT('',(190.,22.7561787149285,-7.62602978582142));
#46154=CARTESIAN_POINT('Ctrl Pts',(190.5,22.2566090894167,-7.54276818156944));
#46155=CARTESIAN_POINT('Ctrl Pts',(190.252700024268,22.5037645883541,-7.58396076472568));
#46156=CARTESIAN_POINT('Ctrl Pts',(190.,22.7561787149285,-7.62602978582142));
#46157=CARTESIAN_POINT('',(189.646446609407,23.1092668802368,-7.6848778133728));
#46158=CARTESIAN_POINT('Ctrl Pts',(189.646446609407,23.1092668802368,-7.6848778133728));
#46159=CARTESIAN_POINT('Ctrl Pts',(189.824548278069,22.9314319357209,-7.65523865595349));
#46160=CARTESIAN_POINT('Ctrl Pts',(190.,22.7561787149285,-7.62602978582142));
#46161=CARTESIAN_POINT('',(189.646446609407,-4.89933402875815,-23.8556510878058));
#46162=CARTESIAN_POINT('Origin',(189.646446609407,0.,-1.49122506038271E-15));
#46163=CARTESIAN_POINT('',(190.,-4.77375383292613,-23.5204437530975));
#46164=CARTESIAN_POINT('Ctrl Pts',(190.,-4.77375383292613,-23.5204437530975));
#46165=CARTESIAN_POINT('Ctrl Pts',(189.824548278103,-4.83608481975967,-23.6868219294316));
#46166=CARTESIAN_POINT('Ctrl Pts',(189.646446609407,-4.89933402875815,-23.8556510878058));
#46167=CARTESIAN_POINT('',(190.5,-4.59607568461225,-23.0461729643192));
#46168=CARTESIAN_POINT('Ctrl Pts',(190.,-4.77375383292613,-23.5204437530975));
#46169=CARTESIAN_POINT('Ctrl Pts',(190.252700024269,-4.6839796106199,-23.2808121966615));
#46170=CARTESIAN_POINT('Ctrl Pts',(190.5,-4.59607568461225,-23.0461729643192));
#46171=CARTESIAN_POINT('',(190.,-5.26806885646218,-23.414684506172));
#46172=CARTESIAN_POINT('Ctrl Pts',(190.499999999993,-4.59607568462184,-23.0461729643245));
#46173=CARTESIAN_POINT('Ctrl Pts',(190.253091651642,-4.92917711905038,-23.2315133585654));
#46174=CARTESIAN_POINT('Ctrl Pts',(190.,-5.26806885646218,-23.414684506172));
#46175=CARTESIAN_POINT('',(190.,-17.6436771757118,-16.2696237116679));
#46176=CARTESIAN_POINT('Origin',(190.,0.,0.));
#46177=CARTESIAN_POINT('',(190.5,-17.6605334048044,-15.5034047827497));
#46178=CARTESIAN_POINT('Ctrl Pts',(190.,-17.6436771757118,-16.2696237116679));
#46179=CARTESIAN_POINT('Ctrl Pts',(190.253091651653,-17.6544921773504,-15.8845492841173));
#46180=CARTESIAN_POINT('Ctrl Pts',(190.500000000013,-17.6605334048048,-15.503404782729));
#46181=CARTESIAN_POINT('Ctrl Pts',(190.5,-17.6605334048044,-15.5034047827497));
#46182=CARTESIAN_POINT('Ctrl Pts',(190.252700024271,-17.819784977732,-15.696851431934));
#46183=CARTESIAN_POINT('Ctrl Pts',(190.,-17.9824248820024,-15.8944139672761));
#46184=CARTESIAN_POINT('Origin',(160.176776695297,0.,-7.45612530191356E-16));
#46185=CARTESIAN_POINT('',(160.353553390593,24.3535533905933,-2.98245012076542E-15));
#46186=CARTESIAN_POINT('',(160.353553390593,-24.3535533905933,-2.98245012076542E-15));
#46187=CARTESIAN_POINT('Origin',(160.353553390593,0.,-1.49122506038271E-15));
#46188=CARTESIAN_POINT('Origin',(160.353553390593,0.,-1.49122506038271E-15));
#46189=CARTESIAN_POINT('',(160.,23.5,2.87791997799628E-15));
#46190=CARTESIAN_POINT('',(160.176776695297,23.9267766952966,2.93018504938085E-15));
#46191=CARTESIAN_POINT('Origin',(160.,0.,0.));
#46192=CARTESIAN_POINT('Origin',(160.5,0.,0.));
#46193=CARTESIAN_POINT('',(160.646446609407,24.6464466094067,3.01831919505661E-15));
#46194=CARTESIAN_POINT('',(160.646446609407,-24.6464466094067,-3.01831919505661E-15));
#46195=CARTESIAN_POINT('Origin',(160.646446609407,0.,-1.5091595975283E-15));
#46196=CARTESIAN_POINT('Origin',(160.646446609407,0.,-1.5091595975283E-15));
#46197=CARTESIAN_POINT('',(160.5,-24.5,-3.00038465791102E-15));
#46198=CARTESIAN_POINT('Origin',(160.,24.,0.));
#46199=CARTESIAN_POINT('',(160.,6.12323399573677E-16,10.));
#46200=CARTESIAN_POINT('Origin',(160.,0.,0.));
#46201=CARTESIAN_POINT('Origin',(189.823223304703,0.,-7.45612530191356E-16));
#46202=CARTESIAN_POINT('',(190.,-4.59607568461223,23.0461729643192));
#46203=CARTESIAN_POINT('Ctrl Pts',(190.,-4.5960756846122,23.0461729643191));
#46204=CARTESIAN_POINT('Ctrl Pts',(189.826457221778,-4.74500028022709,23.4436927837287));
#46205=CARTESIAN_POINT('Ctrl Pts',(189.646446609407,-4.8993340287581,23.8556510878057));
#46206=CARTESIAN_POINT('',(190.,22.2566090894166,7.54276818156944));
#46207=CARTESIAN_POINT('Origin',(190.,0.,0.));
#46208=CARTESIAN_POINT('Ctrl Pts',(189.646446609407,23.1092668802367,7.68487781337279));
#46209=CARTESIAN_POINT('Ctrl Pts',(189.82645722158,22.6753336498196,7.61255560830327));
#46210=CARTESIAN_POINT('Ctrl Pts',(190.,22.2566090894167,7.54276818156945));
#46211=CARTESIAN_POINT('Origin',(189.823223304703,0.,-7.45612530191356E-16));
#46212=CARTESIAN_POINT('',(190.,-4.59607568461224,-23.0461729643192));
#46213=CARTESIAN_POINT('Ctrl Pts',(189.646446609407,-4.89933402875824,-23.855651087806));
#46214=CARTESIAN_POINT('Ctrl Pts',(189.826457222167,-4.74500027989357,-23.4436927828384));
#46215=CARTESIAN_POINT('Ctrl Pts',(190.,-4.5960756846123,-23.0461729643193));
#46216=CARTESIAN_POINT('',(190.,22.2566090894166,-7.54276818156944));
#46217=CARTESIAN_POINT('Ctrl Pts',(190.,22.2566090894165,-7.54276818156942));
#46218=CARTESIAN_POINT('Ctrl Pts',(189.826457222193,22.6753336483417,-7.61255560805694));
#46219=CARTESIAN_POINT('Ctrl Pts',(189.646446609407,23.1092668802368,-7.68487781337279));
#46220=CARTESIAN_POINT('Origin',(190.,0.,0.));
#46221=CARTESIAN_POINT('Origin',(195.5,13.4931969619161,-6.08219949365268));
#46222=CARTESIAN_POINT('',(195.5,13.,-5.5));
#46223=CARTESIAN_POINT('',(196.,13.5,-5.57643645580848));
#46224=CARTESIAN_POINT('',(195.5,13.,-5.5));
#46225=CARTESIAN_POINT('',(195.5,13.4931969619161,-6.08219949365268));
#46226=CARTESIAN_POINT('',(195.5,13.4931969619161,-6.08219949365268));
#46227=CARTESIAN_POINT('',(196.,13.5,-5.57643645580848));
#46228=CARTESIAN_POINT('Origin',(190.,13.246598480958,-5.79109974682634));
#46229=CARTESIAN_POINT('',(190.,13.,-5.5));
#46230=CARTESIAN_POINT('',(190.,13.4931969619161,-6.08219949365268));
#46231=CARTESIAN_POINT('',(190.,11.1403068356888,-3.3047058229942));
#46232=CARTESIAN_POINT('',(190.,13.4931969619161,-6.08219949365268));
#46233=CARTESIAN_POINT('',(190.,13.,-5.5));
#46234=CARTESIAN_POINT('Origin',(195.5,25.,-7.5));
#46235=CARTESIAN_POINT('',(195.5,24.5068030380839,-7.91780050634732));
#46236=CARTESIAN_POINT('',(196.,24.5,-7.40976978914182));
#46237=CARTESIAN_POINT('',(195.5,24.5068030380839,-7.91780050634732));
#46238=CARTESIAN_POINT('',(195.5,25.,-7.5));
#46239=CARTESIAN_POINT('',(195.5,25.,-7.5));
#46240=CARTESIAN_POINT('',(196.,24.5,-7.40976978914182));
#46241=CARTESIAN_POINT('Origin',(195.5,13.,5.5));
#46242=CARTESIAN_POINT('',(195.5,13.4931969619161,6.08219949365268));
#46243=CARTESIAN_POINT('',(196.,13.5,5.57643645580848));
#46244=CARTESIAN_POINT('',(195.5,13.4931969619161,6.08219949365268));
#46245=CARTESIAN_POINT('',(195.5,13.,5.5));
#46246=CARTESIAN_POINT('',(195.5,13.,5.5));
#46247=CARTESIAN_POINT('',(196.,13.5,5.57643645580848));
#46248=CARTESIAN_POINT('Origin',(190.,13.246598480958,5.79109974682634));
#46249=CARTESIAN_POINT('',(190.,13.4931969619161,6.08219949365268));
#46250=CARTESIAN_POINT('',(190.,13.,5.5));
#46251=CARTESIAN_POINT('',(190.,11.1403068356888,3.30470582299419));
#46252=CARTESIAN_POINT('',(190.,13.,5.5));
#46253=CARTESIAN_POINT('',(190.,13.4931969619161,6.08219949365268));
#46254=CARTESIAN_POINT('Origin',(195.75,13.25,3.));
#46255=CARTESIAN_POINT('',(196.,13.5,3.));
#46256=CARTESIAN_POINT('',(195.5,13.,3.));
#46257=CARTESIAN_POINT('Origin',(190.,24.5,-7.40976978914182));
#46258=CARTESIAN_POINT('',(190.5,24.5068030380839,-7.91780050634732));
#46259=CARTESIAN_POINT('',(190.5,25.,-7.5));
#46260=CARTESIAN_POINT('',(190.5,24.5068030380839,-7.91780050634732));
#46261=CARTESIAN_POINT('',(190.,24.5,-7.40976978914182));
#46262=CARTESIAN_POINT('',(190.,24.5,-7.40976978914182));
#46263=CARTESIAN_POINT('',(190.5,25.,-7.5));
#46264=CARTESIAN_POINT('Origin',(190.25,15.4735321792588,-6.15880692444737));
#46265=CARTESIAN_POINT('',(190.,15.5146319260851,-5.91220844348933));
#46266=CARTESIAN_POINT('',(190.5,15.4324324324324,-6.40540540540541));
#46267=CARTESIAN_POINT('Origin',(195.5,24.5068030380839,7.91780050634732));
#46268=CARTESIAN_POINT('',(195.5,25.,7.5));
#46269=CARTESIAN_POINT('',(196.,24.5,7.40976978914182));
#46270=CARTESIAN_POINT('',(195.5,25.,7.5));
#46271=CARTESIAN_POINT('',(195.5,24.5068030380839,7.91780050634732));
#46272=CARTESIAN_POINT('',(195.5,24.5068030380839,7.91780050634732));
#46273=CARTESIAN_POINT('',(196.,24.5,7.40976978914182));
#46274=CARTESIAN_POINT('Origin',(190.,24.5,7.40976978914181));
#46275=CARTESIAN_POINT('',(190.5,25.,7.5));
#46276=CARTESIAN_POINT('',(190.5,24.5068030380839,7.91780050634732));
#46277=CARTESIAN_POINT('',(190.5,25.,7.5));
#46278=CARTESIAN_POINT('',(190.,24.5,7.40976978914182));
#46279=CARTESIAN_POINT('',(190.,24.5,7.40976978914181));
#46280=CARTESIAN_POINT('',(190.5,24.5068030380839,7.91780050634732));
#46281=CARTESIAN_POINT('Origin',(190.25,24.75,-4.));
#46282=CARTESIAN_POINT('',(190.5,25.,-4.));
#46283=CARTESIAN_POINT('',(190.,24.5,-4.));
#46284=CARTESIAN_POINT('Origin',(190.25,21.4735321792588,7.15880692444737));
#46285=CARTESIAN_POINT('',(190.5,21.4324324324324,7.40540540540541));
#46286=CARTESIAN_POINT('',(190.,21.5146319260851,6.91220844348933));
#46287=CARTESIAN_POINT('Origin',(190.,24.753401519042,7.70890025317366));
#46288=CARTESIAN_POINT('',(190.,25.,7.5));
#46289=CARTESIAN_POINT('',(190.,24.5068030380839,7.91780050634732));
#46290=CARTESIAN_POINT('Origin',(195.75,21.4735321792588,7.15880692444737));
#46291=CARTESIAN_POINT('',(196.,21.5146319260851,6.91220844348934));
#46292=CARTESIAN_POINT('',(195.5,21.4324324324324,7.40540540540541));
#46293=CARTESIAN_POINT('Origin',(195.75,24.75,-4.));
#46294=CARTESIAN_POINT('',(196.,24.5,-4.));
#46295=CARTESIAN_POINT('',(195.5,25.,-4.));
#46296=CARTESIAN_POINT('Origin',(190.,24.753401519042,-7.70890025317366));
#46297=CARTESIAN_POINT('',(190.,24.5068030380839,-7.91780050634732));
#46298=CARTESIAN_POINT('',(190.,25.,-7.5));
#46299=CARTESIAN_POINT('Origin',(195.75,15.4735321792588,-6.15880692444737));
#46300=CARTESIAN_POINT('',(196.,15.5146319260851,-5.91220844348933));
#46301=CARTESIAN_POINT('',(195.5,15.4324324324324,-6.40540540540541));
#46302=CARTESIAN_POINT('Origin',(190.,13.,-6.));
#46303=CARTESIAN_POINT('',(190.,11.0540540540541,-5.67567567567568));
#46304=CARTESIAN_POINT('Origin',(190.,13.,6.));
#46305=CARTESIAN_POINT('',(190.,13.,3.));
#46306=CARTESIAN_POINT('Origin',(196.,19.,0.));
#46307=CARTESIAN_POINT('Origin',(190.,25.,-8.));
#46308=CARTESIAN_POINT('Origin',(161.073223304703,0.,-7.54579798764152E-16));
#46309=CARTESIAN_POINT('',(161.5,25.,-3.06161699786838E-15));
#46310=CARTESIAN_POINT('',(161.5,-25.,-3.06161699786838E-15));
#46311=CARTESIAN_POINT('Origin',(161.5,0.,0.));
#46312=CARTESIAN_POINT('Origin',(161.5,0.,0.));
#46313=CARTESIAN_POINT('',(161.073223304703,24.8232233047034,3.0399680964625E-15));
#46314=CARTESIAN_POINT('Origin',(175.,0.,0.));
#46315=CARTESIAN_POINT('',(188.5,25.,3.06161699786838E-15));
#46316=CARTESIAN_POINT('',(188.5,-25.,-3.06161699786838E-15));
#46317=CARTESIAN_POINT('Origin',(188.5,0.,0.));
#46318=CARTESIAN_POINT('Origin',(188.5,0.,0.));
#46319=CARTESIAN_POINT('',(175.,-25.,-3.06161699786838E-15));
#46320=CARTESIAN_POINT('',(168.1,-5.27355936696949E-15,25.));
#46321=CARTESIAN_POINT('Ctrl Pts',(168.1,-5.27355936696949E-15,25.));
#46322=CARTESIAN_POINT('Ctrl Pts',(168.1,-0.55163791047639,25.));
#46323=CARTESIAN_POINT('Ctrl Pts',(168.267431880558,-1.33721306717284,24.9721836184323));
#46324=CARTESIAN_POINT('Ctrl Pts',(168.855166000548,-2.3552917259163,24.8917927252736));
#46325=CARTESIAN_POINT('Ctrl Pts',(169.472757569434,-3.03716583184694,24.8179083643489));
#46326=CARTESIAN_POINT('Ctrl Pts',(170.143631676592,-3.44706604659973,24.7613408689562));
#46327=CARTESIAN_POINT('Ctrl Pts',(170.985290745162,-3.79588962505944,24.7105170302552));
#46328=CARTESIAN_POINT('Ctrl Pts',(171.508328520708,-3.89399419357905,24.6944572637537));
#46329=CARTESIAN_POINT('Ctrl Pts',(172.245040749362,-3.89326696112091,24.6947095740839));
#46330=CARTESIAN_POINT('Ctrl Pts',(172.752744962911,-3.8461850836113,24.7021619625942));
#46331=CARTESIAN_POINT('Ctrl Pts',(173.254085442162,-3.6963447003694,24.7252038218524));
#46332=CARTESIAN_POINT('Ctrl Pts',(174.336500109069,-3.24570229252571,24.790351880959));
#46333=CARTESIAN_POINT('Ctrl Pts',(175.349399920632,-2.33707446060684,24.9151419492839));
#46334=CARTESIAN_POINT('Ctrl Pts',(175.870653276153,-0.779198836510287,
24.995496028175));
#46335=CARTESIAN_POINT('Ctrl Pts',(175.909743056997,-0.0151962230191145,
25.0015962526685));
#46336=CARTESIAN_POINT('Ctrl Pts',(175.882356256358,0.418804816251774,24.9973027627956));
#46337=CARTESIAN_POINT('Ctrl Pts',(175.782240123002,1.08365275900373,24.9819016623594));
#46338=CARTESIAN_POINT('Ctrl Pts',(175.489157477974,1.84426230866362,24.937097682422));
#46339=CARTESIAN_POINT('Ctrl Pts',(174.958007340146,2.56739388230451,24.8693513631287));
#46340=CARTESIAN_POINT('Ctrl Pts',(174.346236594584,3.16619529082572,24.8015572991169));
#46341=CARTESIAN_POINT('Ctrl Pts',(173.337625674135,3.74893731769736,24.7187859134922));
#46342=CARTESIAN_POINT('Ctrl Pts',(172.429820467936,3.89494883801314,24.6944680938334));
#46343=CARTESIAN_POINT('Ctrl Pts',(171.509209330769,3.8953602168609,24.694365273583));
#46344=CARTESIAN_POINT('Ctrl Pts',(170.463418858553,3.69742950735511,24.727449381457));
#46345=CARTESIAN_POINT('Ctrl Pts',(169.587124183002,3.10037920374213,24.8094680053816));
#46346=CARTESIAN_POINT('Ctrl Pts',(168.895370153156,2.41044277844561,24.886002008101));
#46347=CARTESIAN_POINT('Ctrl Pts',(168.595968837042,1.9730248402679,24.926626355682));
#46348=CARTESIAN_POINT('Ctrl Pts',(168.197927739773,1.01300388320702,24.9841804475316));
#46349=CARTESIAN_POINT('Ctrl Pts',(168.1,0.490342890750044,25.));
#46350=CARTESIAN_POINT('Ctrl Pts',(168.1,4.71844785465692E-15,25.));
#46351=CARTESIAN_POINT('Origin',(188.926776695297,0.,-7.54579798764152E-16));
#46352=CARTESIAN_POINT('',(188.926776695297,24.8232233047034,3.0399680964625E-15));
#46353=CARTESIAN_POINT('Origin',(195.5,-1.47925920856996,14.7265510941127));
#46354=CARTESIAN_POINT('',(195.5,-1.73686027918559,14.0083302491977));
#46355=CARTESIAN_POINT('',(196.,-1.92066436668019,14.4795611789942));
#46356=CARTESIAN_POINT('',(195.5,-1.73686027918559,14.0083302491977));
#46357=CARTESIAN_POINT('',(195.5,-1.47925920856996,14.7265510941127));
#46358=CARTESIAN_POINT('',(195.5,-1.47925920856996,14.7265510941127));
#46359=CARTESIAN_POINT('',(196.,-1.92066436668019,14.4795611789942));
#46360=CARTESIAN_POINT('Origin',(190.,-1.60805974387777,14.3674406716552));
#46361=CARTESIAN_POINT('',(190.,-1.73686027918559,14.0083302491977));
#46362=CARTESIAN_POINT('',(190.,-1.47925920856996,14.7265510941127));
#46363=CARTESIAN_POINT('',(190.,-3.22940520398334,9.84694662451038));
#46364=CARTESIAN_POINT('',(190.,-1.47925920856996,14.7265510941127));
#46365=CARTESIAN_POINT('',(190.,-1.73686027918559,14.0083302491977));
#46366=CARTESIAN_POINT('Origin',(195.75,-2.53850810591948,16.8413619022243));
#46367=CARTESIAN_POINT('',(195.746598480958,-5.7005973050323,25.2915246721535));
#46368=CARTESIAN_POINT('',(196.,-5.83295112640872,24.9225072872897));
#46369=CARTESIAN_POINT('',(198.006448117623,-6.88093646116468,22.0006059505128));
#46370=CARTESIAN_POINT('',(196.,-2.77261852837696,16.753656086586));
#46371=CARTESIAN_POINT('',(195.5,-5.39638513844789,25.182414249696));
#46372=CARTESIAN_POINT('',(195.5,-2.304397683462,16.9290677178626));
#46373=CARTESIAN_POINT('',(193.284350279285,-2.66308524417351,24.2020737540619));
#46374=CARTESIAN_POINT('Origin',(195.75,-9.43958256229942,9.84983660014381));
#46375=CARTESIAN_POINT('',(195.746598480958,-11.6385387370803,8.57634092482885));
#46376=CARTESIAN_POINT('',(195.5,-11.2631397208144,8.50833024919771));
#46377=CARTESIAN_POINT('',(194.458916574697,-9.67828935113165,8.22120444506385));
#46378=CARTESIAN_POINT('',(195.5,-9.31458256229942,9.63333024919771));
#46379=CARTESIAN_POINT('',(196.,-11.5793356333198,8.90312472318568));
#46380=CARTESIAN_POINT('',(196.,-9.56458256229942,10.0663429510899));
#46381=CARTESIAN_POINT('',(197.517960591876,-11.2246890678024,10.8606699259324));
#46382=CARTESIAN_POINT('Origin',(190.,-1.30384757729337,14.2583302491977));
#46383=CARTESIAN_POINT('',(190.,1.73388677209908,6.14979985501346));
#46384=CARTESIAN_POINT('',(190.,-5.39396555337319,25.1759557260521));
#46385=CARTESIAN_POINT('',(190.,-1.30384757729337,14.2583302491977));
#46386=CARTESIAN_POINT('',(190.006803038084,-5.39638513844789,25.182414249696));
#46387=CARTESIAN_POINT('',(187.037671232877,-4.34037649759326,22.3636430287683));
#46388=CARTESIAN_POINT('',(190.,-5.39638513844789,25.182414249696));
#46389=CARTESIAN_POINT('Origin',(190.,-11.6961524227066,8.25833024919771));
#46390=CARTESIAN_POINT('',(190.,-11.2631397208144,8.50833024919771));
#46391=CARTESIAN_POINT('',(190.,-11.2631397208144,8.50833024919771));
#46392=CARTESIAN_POINT('',(190.,-5.34807621135331,11.9233937586588));
#46393=CARTESIAN_POINT('Origin',(190.,-11.6385387370803,8.57634092482885));
#46394=CARTESIAN_POINT('',(195.5,-12.0139377533461,8.64435160045999));
#46395=CARTESIAN_POINT('',(195.993196961916,-11.2631397208144,8.50833024919771));
#46396=CARTESIAN_POINT('',(190.,-12.0139377533461,8.64435160045999));
#46397=CARTESIAN_POINT('',(190.,-12.0139377533461,8.64435160045999));
#46398=CARTESIAN_POINT('',(190.,-0.410901631705506,6.54224080151618));
#46399=CARTESIAN_POINT('Origin',(195.5,-19.110417899636,17.2646137433487));
#46400=CARTESIAN_POINT('',(195.5,-18.9951905283833,17.900635094611));
#46401=CARTESIAN_POINT('',(196.,-18.6670488735913,17.5127374981478));
#46402=CARTESIAN_POINT('',(195.5,-18.9951905283833,17.900635094611));
#46403=CARTESIAN_POINT('',(195.5,-19.110417899636,17.2646137433487));
#46404=CARTESIAN_POINT('',(195.5,-19.110417899636,17.2646137433487));
#46405=CARTESIAN_POINT('',(196.,-18.6670488735913,17.5127374981478));
#46406=CARTESIAN_POINT('Origin',(190.,-18.6670488735913,17.5127374981478));
#46407=CARTESIAN_POINT('',(190.5,-18.9951905283833,17.900635094611));
#46408=CARTESIAN_POINT('',(190.5,-19.110417899636,17.2646137433487));
#46409=CARTESIAN_POINT('',(190.5,-18.9951905283833,17.900635094611));
#46410=CARTESIAN_POINT('',(190.,-18.6670488735913,17.5127374981478));
#46411=CARTESIAN_POINT('',(190.,-18.6670488735913,17.5127374981478));
#46412=CARTESIAN_POINT('',(190.5,-19.110417899636,17.2646137433487));
#46413=CARTESIAN_POINT('Origin',(190.25,-9.12740473580835,23.3091287436649));
#46414=CARTESIAN_POINT('',(190.,-9.00240473580835,23.0926223927187));
#46415=CARTESIAN_POINT('',(190.5,-6.0048094716167,25.400635094611));
#46416=CARTESIAN_POINT('',(190.5,-9.25240473580835,23.525635094611));
#46417=CARTESIAN_POINT('',(190.5,-6.0048094716167,25.400635094611));
#46418=CARTESIAN_POINT('Origin',(190.25,-17.2340621790159,15.3787074004835));
#46419=CARTESIAN_POINT('',(190.5,-17.4270728546471,15.2198147351638));
#46420=CARTESIAN_POINT('',(190.,-17.0410515033848,15.5376000658033));
#46421=CARTESIAN_POINT('Origin',(190.,-19.0528042140097,17.5826244189798));
#46422=CARTESIAN_POINT('',(190.,-18.9951905283833,17.900635094611));
#46423=CARTESIAN_POINT('',(190.,-19.110417899636,17.2646137433487));
#46424=CARTESIAN_POINT('Origin',(195.75,-17.2340621790159,15.3787074004835));
#46425=CARTESIAN_POINT('',(196.,-17.0410515033848,15.5376000658033));
#46426=CARTESIAN_POINT('',(195.5,-17.4270728546471,15.2198147351638));
#46427=CARTESIAN_POINT('Origin',(195.75,-9.12740473580835,23.3091287436649));
#46428=CARTESIAN_POINT('',(195.5,-6.0048094716167,25.400635094611));
#46429=CARTESIAN_POINT('',(195.5,-6.0048094716167,25.400635094611));
#46430=CARTESIAN_POINT('',(195.5,-9.25240473580835,23.525635094611));
#46431=CARTESIAN_POINT('',(196.,-9.00240473580835,23.0926223927187));
#46432=CARTESIAN_POINT('Origin',(190.,-5.7005973050323,25.2915246721535));
#46433=CARTESIAN_POINT('',(190.,-6.0048094716167,25.400635094611));
#46434=CARTESIAN_POINT('Origin',(190.,-19.4282032302755,17.650635094611));
#46435=CARTESIAN_POINT('',(190.,-9.15396622993757,5.17027660204442));
#46436=CARTESIAN_POINT('Origin',(190.,-10.3660254037844,16.9544826719043));
#46437=CARTESIAN_POINT('Origin',(190.,-5.57179676972449,25.650635094611));
#46438=CARTESIAN_POINT('Origin',(195.5,-12.0139377533461,-8.64435160045998));
#46439=CARTESIAN_POINT('',(195.5,-11.2631397208144,-8.50833024919769));
#46440=CARTESIAN_POINT('',(196.,-11.5793356333198,-8.90312472318567));
#46441=CARTESIAN_POINT('',(195.5,-11.2631397208144,-8.50833024919769));
#46442=CARTESIAN_POINT('',(195.5,-12.0139377533461,-8.64435160045998));
#46443=CARTESIAN_POINT('',(195.5,-12.0139377533461,-8.64435160045998));
#46444=CARTESIAN_POINT('',(196.,-11.5793356333198,-8.90312472318567));
#46445=CARTESIAN_POINT('Origin',(190.,-11.6385387370803,-8.57634092482884));
#46446=CARTESIAN_POINT('',(190.,-11.2631397208144,-8.5083302491977));
#46447=CARTESIAN_POINT('',(190.,-12.0139377533461,-8.64435160045998));
#46448=CARTESIAN_POINT('',(190.,-0.410901631705511,-6.54224080151617));
#46449=CARTESIAN_POINT('',(190.,-12.0139377533461,-8.64435160045998));
#46450=CARTESIAN_POINT('',(190.,-11.2631397208144,-8.50833024919769));
#46451=CARTESIAN_POINT('Origin',(195.5,-18.9951905283833,-17.900635094611));
#46452=CARTESIAN_POINT('',(195.5,-19.110417899636,-17.2646137433487));
#46453=CARTESIAN_POINT('',(196.,-18.6670488735913,-17.5127374981478));
#46454=CARTESIAN_POINT('',(195.5,-19.110417899636,-17.2646137433487));
#46455=CARTESIAN_POINT('',(195.5,-18.9951905283833,-17.900635094611));
#46456=CARTESIAN_POINT('',(195.5,-18.9951905283833,-17.900635094611));
#46457=CARTESIAN_POINT('',(196.,-18.6670488735913,-17.5127374981478));
#46458=CARTESIAN_POINT('Origin',(195.5,-1.73686027918559,-14.0083302491977));
#46459=CARTESIAN_POINT('',(195.5,-1.47925920856997,-14.7265510941127));
#46460=CARTESIAN_POINT('',(196.,-1.9206643666802,-14.4795611789942));
#46461=CARTESIAN_POINT('',(195.5,-1.47925920856997,-14.7265510941127));
#46462=CARTESIAN_POINT('',(195.5,-1.73686027918559,-14.0083302491977));
#46463=CARTESIAN_POINT('',(195.5,-1.73686027918559,-14.0083302491977));
#46464=CARTESIAN_POINT('',(196.,-1.9206643666802,-14.4795611789942));
#46465=CARTESIAN_POINT('Origin',(190.,-1.60805974387778,-14.3674406716552));
#46466=CARTESIAN_POINT('',(190.,-1.47925920856997,-14.7265510941127));
#46467=CARTESIAN_POINT('',(190.,-1.73686027918559,-14.0083302491977));
#46468=CARTESIAN_POINT('',(190.,-3.22940520398334,-9.84694662451034));
#46469=CARTESIAN_POINT('',(190.,-1.73686027918559,-14.0083302491977));
#46470=CARTESIAN_POINT('',(190.,-1.47925920856997,-14.7265510941127));
#46471=CARTESIAN_POINT('Origin',(195.75,-4.2434301395928,-12.8498366001438));
#46472=CARTESIAN_POINT('',(196.,-4.3684301395928,-13.0663429510899));
#46473=CARTESIAN_POINT('',(195.5,-4.1184301395928,-12.6333302491977));
#46474=CARTESIAN_POINT('Origin',(190.,-18.6670488735913,-17.5127374981478));
#46475=CARTESIAN_POINT('',(190.5,-19.110417899636,-17.2646137433487));
#46476=CARTESIAN_POINT('',(190.5,-18.9951905283833,-17.900635094611));
#46477=CARTESIAN_POINT('',(190.5,-19.110417899636,-17.2646137433487));
#46478=CARTESIAN_POINT('',(190.,-18.6670488735913,-17.5127374981478));
#46479=CARTESIAN_POINT('',(190.,-18.6670488735913,-17.5127374981478));
#46480=CARTESIAN_POINT('',(190.5,-18.9951905283833,-17.900635094611));
#46481=CARTESIAN_POINT('Origin',(190.25,-13.3680367752315,-10.6825549777769));
#46482=CARTESIAN_POINT('',(190.,-13.1750260996004,-10.8414476430966));
#46483=CARTESIAN_POINT('',(190.5,-13.5610474508627,-10.5236623124571));
#46484=CARTESIAN_POINT('Origin',(195.5,-5.39638513844791,-25.182414249696));
#46485=CARTESIAN_POINT('',(195.5,-6.00480947161672,-25.400635094611));
#46486=CARTESIAN_POINT('',(196.,-5.83295112640873,-24.9225072872897));
#46487=CARTESIAN_POINT('',(195.5,-6.00480947161672,-25.400635094611));
#46488=CARTESIAN_POINT('',(195.5,-5.39638513844791,-25.182414249696));
#46489=CARTESIAN_POINT('',(195.5,-5.39638513844791,-25.182414249696));
#46490=CARTESIAN_POINT('',(196.,-5.83295112640874,-24.9225072872896));
#46491=CARTESIAN_POINT('Origin',(190.,-5.83295112640874,-24.9225072872897));
#46492=CARTESIAN_POINT('',(190.5,-6.00480947161672,-25.400635094611));
#46493=CARTESIAN_POINT('',(190.5,-5.39638513844791,-25.182414249696));
#46494=CARTESIAN_POINT('',(190.5,-6.00480947161672,-25.400635094611));
#46495=CARTESIAN_POINT('',(190.,-5.83295112640874,-24.9225072872897));
#46496=CARTESIAN_POINT('',(190.,-5.83295112640874,-24.9225072872897));
#46497=CARTESIAN_POINT('',(190.5,-5.39638513844791,-25.182414249696));
#46498=CARTESIAN_POINT('Origin',(190.25,-16.0556079660839,-19.3091287436648));
#46499=CARTESIAN_POINT('',(190.5,-16.1806079660839,-19.525635094611));
#46500=CARTESIAN_POINT('',(190.,-15.9306079660839,-19.0926223927187));
#46501=CARTESIAN_POINT('Origin',(190.25,-4.67248270213506,-22.5375143249309));
#46502=CARTESIAN_POINT('',(190.5,-4.43837227967758,-22.6252201405692));
#46503=CARTESIAN_POINT('',(190.,-4.90659312459254,-22.4498085092926));
#46504=CARTESIAN_POINT('Origin',(190.,-5.70059730503231,-25.2915246721535));
#46505=CARTESIAN_POINT('',(190.,-6.00480947161672,-25.400635094611));
#46506=CARTESIAN_POINT('',(190.,-5.39638513844791,-25.182414249696));
#46507=CARTESIAN_POINT('Origin',(195.75,-4.67248270213506,-22.5375143249309));
#46508=CARTESIAN_POINT('',(196.,-4.90659312459254,-22.4498085092926));
#46509=CARTESIAN_POINT('',(195.5,-4.43837227967758,-22.6252201405692));
#46510=CARTESIAN_POINT('Origin',(195.75,-16.0556079660839,-19.3091287436648));
#46511=CARTESIAN_POINT('',(196.,-15.9306079660839,-19.0926223927187));
#46512=CARTESIAN_POINT('',(195.5,-16.1806079660839,-19.525635094611));
#46513=CARTESIAN_POINT('Origin',(190.,-19.0528042140097,-17.5826244189798));
#46514=CARTESIAN_POINT('',(190.,-19.110417899636,-17.2646137433487));
#46515=CARTESIAN_POINT('',(190.,-18.9951905283833,-17.900635094611));
#46516=CARTESIAN_POINT('Origin',(195.75,-13.3680367752315,-10.6825549777769));
#46517=CARTESIAN_POINT('',(196.,-13.1750260996004,-10.8414476430966));
#46518=CARTESIAN_POINT('',(195.5,-13.5610474508627,-10.5236623124571));
#46519=CARTESIAN_POINT('Origin',(190.,-11.6961524227066,-8.25833024919769));
#46520=CARTESIAN_POINT('',(190.,-5.28794082615313,-0.47412417933778));
#46521=CARTESIAN_POINT('Origin',(190.,-1.30384757729338,-14.2583302491977));
#46522=CARTESIAN_POINT('',(190.,-0.151923788646696,-14.9233937586588));
#46523=CARTESIAN_POINT('Origin',(196.,-10.3660254037844,-16.9544826719043));
#46524=CARTESIAN_POINT('Origin',(190.,-19.4282032302755,-17.650635094611));
#46525=CARTESIAN_POINT('Ctrl Pts',(168.1,4.71844785465692E-15,25.));
#46526=CARTESIAN_POINT('Ctrl Pts',(168.1,0.490342890750044,25.));
#46527=CARTESIAN_POINT('Ctrl Pts',(168.197927739773,1.01300388320702,24.9841804475316));
#46528=CARTESIAN_POINT('Ctrl Pts',(168.595968837042,1.9730248402679,24.926626355682));
#46529=CARTESIAN_POINT('Ctrl Pts',(168.895370153156,2.41044277844561,24.886002008101));
#46530=CARTESIAN_POINT('Ctrl Pts',(169.587124183002,3.10037920374213,24.8094680053816));
#46531=CARTESIAN_POINT('Ctrl Pts',(170.463418858553,3.69742950735511,24.727449381457));
#46532=CARTESIAN_POINT('Ctrl Pts',(171.509209330769,3.8953602168609,24.694365273583));
#46533=CARTESIAN_POINT('Ctrl Pts',(172.429820467936,3.89494883801314,24.6944680938334));
#46534=CARTESIAN_POINT('Ctrl Pts',(173.337625674135,3.74893731769736,24.7187859134922));
#46535=CARTESIAN_POINT('Ctrl Pts',(174.346236594584,3.16619529082572,24.8015572991169));
#46536=CARTESIAN_POINT('Ctrl Pts',(174.958007340146,2.56739388230451,24.8693513631287));
#46537=CARTESIAN_POINT('Ctrl Pts',(175.489157477974,1.84426230866362,24.937097682422));
#46538=CARTESIAN_POINT('Ctrl Pts',(175.782240123002,1.08365275900373,24.9819016623594));
#46539=CARTESIAN_POINT('Ctrl Pts',(175.882356256358,0.418804816251774,24.9973027627956));
#46540=CARTESIAN_POINT('Ctrl Pts',(175.909743056997,-0.0151962230191145,
25.0015962526685));
#46541=CARTESIAN_POINT('Ctrl Pts',(175.870653276153,-0.779198836510287,
24.995496028175));
#46542=CARTESIAN_POINT('Ctrl Pts',(175.349399920632,-2.33707446060684,24.9151419492839));
#46543=CARTESIAN_POINT('Ctrl Pts',(174.336500109069,-3.24570229252571,24.790351880959));
#46544=CARTESIAN_POINT('Ctrl Pts',(173.254085442162,-3.6963447003694,24.7252038218524));
#46545=CARTESIAN_POINT('Ctrl Pts',(172.752744962911,-3.8461850836113,24.7021619625942));
#46546=CARTESIAN_POINT('Ctrl Pts',(172.245040749362,-3.89326696112091,24.6947095740839));
#46547=CARTESIAN_POINT('Ctrl Pts',(171.508328520708,-3.89399419357905,24.6944572637537));
#46548=CARTESIAN_POINT('Ctrl Pts',(170.985290745162,-3.79588962505944,24.7105170302552));
#46549=CARTESIAN_POINT('Ctrl Pts',(170.143631676592,-3.44706604659973,24.7613408689562));
#46550=CARTESIAN_POINT('Ctrl Pts',(169.472757569434,-3.03716583184694,24.8179083643489));
#46551=CARTESIAN_POINT('Ctrl Pts',(168.855166000548,-2.3552917259163,24.8917927252736));
#46552=CARTESIAN_POINT('Ctrl Pts',(168.267431880558,-1.33721306717284,24.9721836184323));
#46553=CARTESIAN_POINT('Ctrl Pts',(168.1,-0.55163791047639,25.));
#46554=CARTESIAN_POINT('Ctrl Pts',(168.1,-5.27355936696949E-15,25.));
#46555=CARTESIAN_POINT('Ctrl Pts',(168.266666666667,5.18104078158406E-15,
24.8333333333333));
#46556=CARTESIAN_POINT('Ctrl Pts',(168.266794313848,0.46646552227959,24.8332945640787));
#46557=CARTESIAN_POINT('Ctrl Pts',(168.359180904007,0.963922026904903,24.8188633380089));
#46558=CARTESIAN_POINT('Ctrl Pts',(168.736647912911,1.87993410901415,24.7661135751049));
#46559=CARTESIAN_POINT('Ctrl Pts',(169.021233517307,2.29895226345512,24.7288087600252));
#46560=CARTESIAN_POINT('Ctrl Pts',(169.681526448759,2.96173987210032,24.6583672833831));
#46561=CARTESIAN_POINT('Ctrl Pts',(170.520653439136,3.53818245366667,24.5826826921013));
#46562=CARTESIAN_POINT('Ctrl Pts',(171.527523707823,3.73046459774516,24.552046576372));
#46563=CARTESIAN_POINT('Ctrl Pts',(172.413771265711,3.73012216169543,24.5521081449956));
#46564=CARTESIAN_POINT('Ctrl Pts',(173.287906724152,3.5882347276893,24.5746675296835));
#46565=CARTESIAN_POINT('Ctrl Pts',(174.254886758977,3.02511186587481,24.6510708296085));
#46566=CARTESIAN_POINT('Ctrl Pts',(174.838876351617,2.44963017461608,24.7134857403187));
#46567=CARTESIAN_POINT('Ctrl Pts',(175.34440855413,1.7566933645737,24.7757283812278));
#46568=CARTESIAN_POINT('Ctrl Pts',(175.62192885337,1.03127566426168,24.8167727108676));
#46569=CARTESIAN_POINT('Ctrl Pts',(175.716614807647,0.398528431220379,24.8308669619708));
#46570=CARTESIAN_POINT('Ctrl Pts',(175.74268254159,-0.0144929189767075,
24.834825400553));
#46571=CARTESIAN_POINT('Ctrl Pts',(175.705398994411,-0.741374199846019,
24.8291900085961));
#46572=CARTESIAN_POINT('Ctrl Pts',(175.212629384802,-2.22576153108993,24.7557075376013));
#46573=CARTESIAN_POINT('Ctrl Pts',(174.246508948037,-3.10188851295124,24.6407628837638));
#46574=CARTESIAN_POINT('Ctrl Pts',(173.206751709011,-3.53753804437446,24.5805554974687));
#46575=CARTESIAN_POINT('Ctrl Pts',(172.724760251488,-3.68273779709261,24.5592626343764));
#46576=CARTESIAN_POINT('Ctrl Pts',(172.235889172339,-3.72837740200832,24.5523529001695));
#46577=CARTESIAN_POINT('Ctrl Pts',(171.526624153034,-3.72910914453677,24.5521281243884));
#46578=CARTESIAN_POINT('Ctrl Pts',(171.023033964314,-3.63384469616512,24.5669908902667));
#46579=CARTESIAN_POINT('Ctrl Pts',(170.21475055214,-3.29646898944012,24.6139400570373));
#46580=CARTESIAN_POINT('Ctrl Pts',(169.571724746233,-2.90061882815568,24.6661617079234));
#46581=CARTESIAN_POINT('Ctrl Pts',(168.983106184116,-2.24590741304073,24.7341018810264));
#46582=CARTESIAN_POINT('Ctrl Pts',(168.424797307501,-1.27242652685453,24.8078743314681));
#46583=CARTESIAN_POINT('Ctrl Pts',(168.266819442733,-0.524653038198594,
24.8332660143837));
#46584=CARTESIAN_POINT('Ctrl Pts',(168.266666666667,-4.92661467177413E-15,
24.8333333333333));
#46585=CARTESIAN_POINT('Ctrl Pts',(168.433333333333,5.64363370851121E-15,
24.6666666666667));
#46586=CARTESIAN_POINT('Ctrl Pts',(168.433205686152,0.442806217695906,24.6667054359213));
#46587=CARTESIAN_POINT('Ctrl Pts',(168.520379536409,0.91470391372393,24.6535646536479));
#46588=CARTESIAN_POINT('Ctrl Pts',(168.877269223955,1.78698013807251,24.6056117012029));
#46589=CARTESIAN_POINT('Ctrl Pts',(169.146992671644,2.1872659561253,24.5716344807208));
#46590=CARTESIAN_POINT('Ctrl Pts',(169.775922003246,2.82331390133092,24.5072699203476));
#46591=CARTESIAN_POINT('Ctrl Pts',(170.577934640553,3.37899466011285,24.4379056542893));
#46592=CARTESIAN_POINT('Ctrl Pts',(171.545724932034,3.56573461402839,24.4097113651223));
#46593=CARTESIAN_POINT('Ctrl Pts',(172.397850870814,3.56527124811576,24.4098336919766));
#46594=CARTESIAN_POINT('Ctrl Pts',(173.238134781157,3.42758948674762,24.4305206134708));
#46595=CARTESIAN_POINT('Ctrl Pts',(174.163594379135,2.88409824873316,24.5006229869098));
#46596=CARTESIAN_POINT('Ctrl Pts',(174.719788670977,2.33179149336597,24.5576379696713));
#46597=CARTESIAN_POINT('Ctrl Pts',(175.199753282856,1.66921727355042,24.6143923044647));
#46598=CARTESIAN_POINT('Ctrl Pts',(175.461540937543,0.978935543629066,24.6516390819393));
#46599=CARTESIAN_POINT('Ctrl Pts',(175.550908639782,0.378121403509141,24.6644241544695));
#46600=CARTESIAN_POINT('Ctrl Pts',(175.575182231976,-0.013759292292757,
24.6679615551863));
#46601=CARTESIAN_POINT('Ctrl Pts',(175.54045160512,-0.703288512377423,24.6629300098085));
#46602=CARTESIAN_POINT('Ctrl Pts',(175.075553895695,-2.11484158369124,24.5962216033143));
#46603=CARTESIAN_POINT('Ctrl Pts',(174.156435039991,-2.95775050705498,24.4912024202838));
#46604=CARTESIAN_POINT('Ctrl Pts',(173.159523604679,-3.37904065905067,24.435945095832));
#46605=CARTESIAN_POINT('Ctrl Pts',(172.696689494759,-3.51943249259346,24.4163697846433));
#46606=CARTESIAN_POINT('Ctrl Pts',(172.22679180891,-3.56372681457438,24.4100388485919));
#46607=CARTESIAN_POINT('Ctrl Pts',(171.544865156729,-3.56444742418653,24.4098140012409));
#46608=CARTESIAN_POINT('Ctrl Pts',(171.060891525884,-3.47208196124947,24.4234898517845));
#46609=CARTESIAN_POINT('Ctrl Pts',(170.285774210988,-3.14615677796927,24.4665898256047));
#46610=CARTESIAN_POINT('Ctrl Pts',(169.670874519592,-2.7645296126956,24.5144289115002));
#46611=CARTESIAN_POINT('Ctrl Pts',(169.110734773122,-2.13677771520377,24.5765207741377));
#46612=CARTESIAN_POINT('Ctrl Pts',(168.581809251079,-1.20782067924886,24.6436651038428));
#46613=CARTESIAN_POINT('Ctrl Pts',(168.433180557267,-0.498281671690027,
24.6667339856163));
#46614=CARTESIAN_POINT('Ctrl Pts',(168.433333333333,-4.57966997657877E-15,
24.6666666666667));
#46615=CARTESIAN_POINT('Ctrl Pts',(168.6,6.10622663543836E-15,24.5));
#46616=CARTESIAN_POINT('Ctrl Pts',(168.6,0.418928849225452,24.5));
#46617=CARTESIAN_POINT('Ctrl Pts',(168.681632700643,0.865622057421811,24.4882475441252));
#46618=CARTESIAN_POINT('Ctrl Pts',(169.017948299824,1.69388940681876,24.4450989206258));
#46619=CARTESIAN_POINT('Ctrl Pts',(169.272856035795,2.07577544113481,24.414441232645));
#46620=CARTESIAN_POINT('Ctrl Pts',(169.870324269003,2.68467456968911,24.3561691983492));
#46621=CARTESIAN_POINT('Ctrl Pts',(170.635169221136,3.21974760642441,24.2931389649336));
#46622=CARTESIAN_POINT('Ctrl Pts',(171.564039309088,3.40083899491265,24.2673926679114));
#46623=CARTESIAN_POINT('Ctrl Pts',(172.38180166859,3.40044457179805,24.2674737431389));
#46624=CARTESIAN_POINT('Ctrl Pts',(173.188415831174,3.26688689673955,24.286402229662));
#46625=CARTESIAN_POINT('Ctrl Pts',(174.072244543528,2.74301482378225,24.3501365174014));
#46626=CARTESIAN_POINT('Ctrl Pts',(174.600657682448,2.21402778567754,24.4017723468613));
#46627=CARTESIAN_POINT('Ctrl Pts',(175.055004359013,1.5816483294605,24.4530230032705));
#46628=CARTESIAN_POINT('Ctrl Pts',(175.301229667911,0.926558448887017,24.4865101304475));
#46629=CARTESIAN_POINT('Ctrl Pts',(175.385167191071,0.357845018477747,24.4979883536447));
#46630=CARTESIAN_POINT('Ctrl Pts',(175.408121716569,-0.01305598825035,24.5011907030708));
#46631=CARTESIAN_POINT('Ctrl Pts',(175.375197323378,-0.665463875713155,
24.4966239902296));
#46632=CARTESIAN_POINT('Ctrl Pts',(174.938783359865,-2.00352865417433,24.4367871916318));
#46633=CARTESIAN_POINT('Ctrl Pts',(174.066443878959,-2.81393672748051,24.3416134230885));
#46634=CARTESIAN_POINT('Ctrl Pts',(173.112189871528,-3.22023400305574,24.2912967714483));
#46635=CARTESIAN_POINT('Ctrl Pts',(172.668704783337,-3.35598520607476,24.2734704564255));
#46636=CARTESIAN_POINT('Ctrl Pts',(172.217640231887,-3.3988372554618,24.2676821746775));
#46637=CARTESIAN_POINT('Ctrl Pts',(171.563160789055,-3.39956237514424,24.2674848618756));
#46638=CARTESIAN_POINT('Ctrl Pts',(171.098634745036,-3.31003703235515,24.279963711796));
#46639=CARTESIAN_POINT('Ctrl Pts',(170.356893086536,-2.99555972080966,24.3191890136858));
#46640=CARTESIAN_POINT('Ctrl Pts',(169.769841696391,-2.62798260900435,24.3626822550747));
#46641=CARTESIAN_POINT('Ctrl Pts',(169.23867495669,-2.0273934023282,24.4188299298905));
#46642=CARTESIAN_POINT('Ctrl Pts',(168.739174678022,-1.14303413893055,24.4793558168787));
#46643=CARTESIAN_POINT('Ctrl Pts',(168.6,-0.471296799412231,24.5));
#46644=CARTESIAN_POINT('Ctrl Pts',(168.6,-4.23272528138341E-15,24.5));
#46645=CARTESIAN_POINT('',(168.6,6.10622663543836E-15,24.5));
#46646=CARTESIAN_POINT('',(168.1,4.71844785465692E-15,25.));
#46647=CARTESIAN_POINT('Ctrl Pts',(168.6,6.10622663543836E-15,24.5));
#46648=CARTESIAN_POINT('Ctrl Pts',(168.6,0.418928849225452,24.5));
#46649=CARTESIAN_POINT('Ctrl Pts',(168.681632700643,0.865622057421811,24.4882475441252));
#46650=CARTESIAN_POINT('Ctrl Pts',(169.017948299824,1.69388940681876,24.4450989206258));
#46651=CARTESIAN_POINT('Ctrl Pts',(169.272856035795,2.07577544113481,24.414441232645));
#46652=CARTESIAN_POINT('Ctrl Pts',(169.870324269003,2.68467456968911,24.3561691983492));
#46653=CARTESIAN_POINT('Ctrl Pts',(170.635169221136,3.21974760642441,24.2931389649336));
#46654=CARTESIAN_POINT('Ctrl Pts',(171.564039309088,3.40083899491265,24.2673926679114));
#46655=CARTESIAN_POINT('Ctrl Pts',(172.38180166859,3.40044457179805,24.2674737431389));
#46656=CARTESIAN_POINT('Ctrl Pts',(173.188415831174,3.26688689673955,24.286402229662));
#46657=CARTESIAN_POINT('Ctrl Pts',(174.072244543528,2.74301482378225,24.3501365174014));
#46658=CARTESIAN_POINT('Ctrl Pts',(174.600657682448,2.21402778567754,24.4017723468613));
#46659=CARTESIAN_POINT('Ctrl Pts',(175.055004359013,1.5816483294605,24.4530230032705));
#46660=CARTESIAN_POINT('Ctrl Pts',(175.301229667911,0.926558448887017,24.4865101304475));
#46661=CARTESIAN_POINT('Ctrl Pts',(175.385167191071,0.357845018477747,24.4979883536447));
#46662=CARTESIAN_POINT('Ctrl Pts',(175.408121716569,-0.01305598825035,24.5011907030708));
#46663=CARTESIAN_POINT('Ctrl Pts',(175.375197323378,-0.665463875713155,
24.4966239902296));
#46664=CARTESIAN_POINT('Ctrl Pts',(174.938783359865,-2.00352865417433,24.4367871916318));
#46665=CARTESIAN_POINT('Ctrl Pts',(174.066443878959,-2.81393672748051,24.3416134230885));
#46666=CARTESIAN_POINT('Ctrl Pts',(173.112189871528,-3.22023400305574,24.2912967714483));
#46667=CARTESIAN_POINT('Ctrl Pts',(172.668704783337,-3.35598520607476,24.2734704564255));
#46668=CARTESIAN_POINT('Ctrl Pts',(172.217640231887,-3.3988372554618,24.2676821746775));
#46669=CARTESIAN_POINT('Ctrl Pts',(171.563160789055,-3.39956237514424,24.2674848618756));
#46670=CARTESIAN_POINT('Ctrl Pts',(171.098634745036,-3.31003703235515,24.279963711796));
#46671=CARTESIAN_POINT('Ctrl Pts',(170.356893086536,-2.99555972080966,24.3191890136858));
#46672=CARTESIAN_POINT('Ctrl Pts',(169.769841696391,-2.62798260900435,24.3626822550747));
#46673=CARTESIAN_POINT('Ctrl Pts',(169.23867495669,-2.0273934023282,24.4188299298905));
#46674=CARTESIAN_POINT('Ctrl Pts',(168.739174678022,-1.14303413893055,24.4793558168787));
#46675=CARTESIAN_POINT('Ctrl Pts',(168.6,-0.471296799412231,24.5));
#46676=CARTESIAN_POINT('Ctrl Pts',(168.6,-4.23272528138341E-15,24.5));
#46677=CARTESIAN_POINT('Origin',(172.,0.,25.));
#46678=CARTESIAN_POINT('',(168.6,-4.163799117101E-16,10.));
#46679=CARTESIAN_POINT('',(168.6,4.163799117101E-16,25.));
#46680=CARTESIAN_POINT('',(175.4,0.,10.));
#46681=CARTESIAN_POINT('Origin',(172.,0.,10.));
#46682=CARTESIAN_POINT('Origin',(172.,0.,10.));
#46683=CARTESIAN_POINT('Origin',(172.,0.,10.));
#46684=CARTESIAN_POINT('',(175.,0.,10.));
#46685=CARTESIAN_POINT('Origin',(172.,0.,10.));
#46686=CARTESIAN_POINT('',(175.,0.,10.));
#46687=CARTESIAN_POINT('Origin',(190.,-5.5717967697245,-25.650635094611));
#46688=CARTESIAN_POINT('',(190.,-0.400087824116491,-11.8459522777201));
#46689=CARTESIAN_POINT('Origin',(190.,-10.3660254037844,-16.9544826719043));
#46690=CARTESIAN_POINT('Origin',(196.,-10.3660254037844,16.9544826719043));
#46691=CARTESIAN_POINT('Origin',(190.,25.,8.));
#46692=CARTESIAN_POINT('',(190.,17.0540540540541,6.67567567567568));
#46693=CARTESIAN_POINT('Origin',(190.,19.,0.));
#46694=CARTESIAN_POINT('Origin',(175.,0.,0.));
#46695=CARTESIAN_POINT('',(190.,6.12323399573677E-16,10.));
#46696=CARTESIAN_POINT('Origin',(190.,0.,0.));
#46697=CARTESIAN_POINT('',(175.,6.12323399573677E-16,10.));
#46698=CARTESIAN_POINT('',(175.,6.12323399573677E-16,10.));
#46699=CARTESIAN_POINT('Origin',(190.,10.,0.));
#46700=CARTESIAN_POINT('',(0.,0.,0.));
#46701=CARTESIAN_POINT('Origin',(-14.75,0.,0.));
#46702=CARTESIAN_POINT('',(-29.0911584740964,-4.93085069296601,0.00239406595250471));
#46703=CARTESIAN_POINT('',(-29.3088415259036,-4.92746336814012,0.00144215323830204));
#46704=CARTESIAN_POINT('',(-14.75,-4.925,-6.03138548580071E-16));
#46705=CARTESIAN_POINT('',(-29.575,2.17167188636589,4.42425492889053));
#46706=CARTESIAN_POINT('Ctrl Pts',(-29.0911584740964,-4.93085069296601,
0.00239406595250471));
#46707=CARTESIAN_POINT('Ctrl Pts',(-29.0987040309128,-4.93188800524103,
0.15750466532186));
#46708=CARTESIAN_POINT('Ctrl Pts',(-29.1062495877292,-4.92523207312776,
0.312531807375031));
#46709=CARTESIAN_POINT('Ctrl Pts',(-29.1137951445456,-4.91059689710246,
0.466805765893802));
#46710=CARTESIAN_POINT('Ctrl Pts',(-29.1933410329187,-4.75631165258633,
2.09317468495417));
#46711=CARTESIAN_POINT('Ctrl Pts',(-29.2728869212918,-3.71524898717827,
3.63583816030893));
#46712=CARTESIAN_POINT('Ctrl Pts',(-29.3524328096649,-2.26290809811278,
4.38440317990658));
#46713=CARTESIAN_POINT('Ctrl Pts',(-29.4266218731099,-0.908371583825934,
5.08255790377123));
#46714=CARTESIAN_POINT('Ctrl Pts',(-29.5008109365549,0.803915241080997,
5.08996618673832));
#46715=CARTESIAN_POINT('Ctrl Pts',(-29.575,2.17494790042119,4.42655504786424));
#46716=CARTESIAN_POINT('',(-29.575,-2.1683958723106,4.4219548099168));
#46717=CARTESIAN_POINT('Origin',(-29.575,0.,0.));
#46718=CARTESIAN_POINT('Ctrl Pts',(-29.575,-2.16839587231058,4.42195480991681));
#46719=CARTESIAN_POINT('Ctrl Pts',(-29.5352270558135,-2.90509583874374,
4.0606989321402));
#46720=CARTESIAN_POINT('Ctrl Pts',(-29.4954541116269,-3.54417075123437,
3.51185369356184));
#46721=CARTESIAN_POINT('Ctrl Pts',(-29.4556811674404,-4.01940836209596,
2.8419582808667));
#46722=CARTESIAN_POINT('Ctrl Pts',(-29.4159082232539,-4.49464597295758,
2.17206286817154));
#46723=CARTESIAN_POINT('Ctrl Pts',(-29.3761352790673,-4.80604628219013,
1.38111728135961));
#46724=CARTESIAN_POINT('Ctrl Pts',(-29.3363623348808,-4.89820932110733,
0.567147712221922));
#46725=CARTESIAN_POINT('Ctrl Pts',(-29.3271887318884,-4.91946666443181,
0.379406175157601));
#46726=CARTESIAN_POINT('Ctrl Pts',(-29.318015128896,-4.929060779183,0.190439782628943));
#46727=CARTESIAN_POINT('Ctrl Pts',(-29.3088415259036,-4.92746336814012,
0.00144215323830204));
#46728=CARTESIAN_POINT('Origin',(-14.75,0.,0.));
#46729=CARTESIAN_POINT('',(-27.5911584740964,-4.91871916148224,0.00298870709768639));
#46730=CARTESIAN_POINT('',(-27.8088415259036,-4.91810465358294,0.00250400581179228));
#46731=CARTESIAN_POINT('',(-14.75,-4.925,-6.03138548580071E-16));
#46732=CARTESIAN_POINT('Ctrl Pts',(-27.5911584740964,-4.91871916148224,
0.00298870709768639));
#46733=CARTESIAN_POINT('Ctrl Pts',(-27.6214287006744,-4.92217786568793,
0.629288456904983));
#46734=CARTESIAN_POINT('Ctrl Pts',(-27.6516989272523,-4.81132058056506,
1.2544097760338));
#46735=CARTESIAN_POINT('Ctrl Pts',(-27.6819691538303,-4.58053680634953,
1.83157791678433));
#46736=CARTESIAN_POINT('Ctrl Pts',(-27.7615150422034,-3.97406958038444,
3.34829442957306));
#46737=CARTESIAN_POINT('Ctrl Pts',(-27.8410609305764,-2.53943282222183,
4.53386340685575));
#46738=CARTESIAN_POINT('Ctrl Pts',(-27.9206068189495,-0.935593024822473,
4.84364324705812));
#46739=CARTESIAN_POINT('Ctrl Pts',(-28.0001527073226,0.668246772576907,
5.1534230872605));
#46740=CARTESIAN_POINT('Ctrl Pts',(-28.0796985956957,2.44128960921305,4.58741379038254));
#46741=CARTESIAN_POINT('Ctrl Pts',(-28.1592444840688,3.56896084480546,3.40568511210877));
#46742=CARTESIAN_POINT('Ctrl Pts',(-28.2387903724418,4.69663208039786,2.22395643383501));
#46743=CARTESIAN_POINT('Ctrl Pts',(-28.3183362608148,5.17893171494654,0.426508374165463));
#46744=CARTESIAN_POINT('Ctrl Pts',(-28.3978821491879,4.79450650284291,-1.16110247139908));
#46745=CARTESIAN_POINT('Ctrl Pts',(-28.477428037561,4.41008129073928,-2.74871331696362));
#46746=CARTESIAN_POINT('Ctrl Pts',(-28.5569739259341,3.15893123198334,-4.12648694842314));
#46747=CARTESIAN_POINT('Ctrl Pts',(-28.6365198143072,1.61540970892298,-4.66128231395555));
#46748=CARTESIAN_POINT('Ctrl Pts',(-28.7160657026803,0.0718881858626222,
-5.19607767948796));
#46749=CARTESIAN_POINT('Ctrl Pts',(-28.7956115910533,-1.76400480150215,
-4.88789477909325));
#46750=CARTESIAN_POINT('Ctrl Pts',(-28.8751574794264,-3.04819738337245,
-3.87876614751291));
#46751=CARTESIAN_POINT('Ctrl Pts',(-28.9471578109831,-4.21057413933529,
-2.96536135006638));
#46752=CARTESIAN_POINT('Ctrl Pts',(-29.0191581425397,-4.92095257284757,
-1.4776841912631));
#46753=CARTESIAN_POINT('Ctrl Pts',(-29.0911584740964,-4.93085069296601,
0.00239406595250471));
#46754=CARTESIAN_POINT('Ctrl Pts',(-29.3088415259036,-4.92746336814012,
0.00144215323830204));
#46755=CARTESIAN_POINT('Ctrl Pts',(-29.2384692405229,-4.91520935345547,
-1.44839114811431));
#46756=CARTESIAN_POINT('Ctrl Pts',(-29.1680969551423,-4.24436898433528,
-2.90006264127696));
#46757=CARTESIAN_POINT('Ctrl Pts',(-29.0977246697616,-3.12788046011008,
-3.81474362504512));
#46758=CARTESIAN_POINT('Ctrl Pts',(-29.0181787813885,-1.86584852470544,
-4.8486607564584));
#46759=CARTESIAN_POINT('Ctrl Pts',(-28.9386328930154,-0.0344076573231608,
-5.19645995170656));
#46760=CARTESIAN_POINT('Ctrl Pts',(-28.8590870046423,1.52027960945058,-4.69387792027941));
#46761=CARTESIAN_POINT('Ctrl Pts',(-28.7795411162692,3.07496687622432,-4.19129588885225));
#46762=CARTESIAN_POINT('Ctrl Pts',(-28.6999952278962,4.35290054238952,-2.83833263074978));
#46763=CARTESIAN_POINT('Ctrl Pts',(-28.6204493395231,4.76944898889192,-1.25865959225591));
#46764=CARTESIAN_POINT('Ctrl Pts',(-28.54090345115,5.18599743539432,0.321013446237961));
#46765=CARTESIAN_POINT('Ctrl Pts',(-28.4613575627769,4.74116066223391,2.12739626512323));
#46766=CARTESIAN_POINT('Ctrl Pts',(-28.3818116744039,3.63804206657526,3.33181334358779));
#46767=CARTESIAN_POINT('Ctrl Pts',(-28.3022657860308,2.53492347091661,4.53623042205235));
#46768=CARTESIAN_POINT('Ctrl Pts',(-28.2227198976577,0.773523052759708,
5.13868176009622));
#46769=CARTESIAN_POINT('Ctrl Pts',(-28.1431740092847,-0.836391940911384,
4.8618460820682));
#46770=CARTESIAN_POINT('Ctrl Pts',(-28.0636281209116,-2.44630693458247,
4.58501040404019));
#46771=CARTESIAN_POINT('Ctrl Pts',(-27.9840822325385,-3.90473650376776,
3.42888770994031));
#46772=CARTESIAN_POINT('Ctrl Pts',(-27.9045363441654,-4.54206616433802,
1.92485926408358));
#46773=CARTESIAN_POINT('Ctrl Pts',(-27.8726380714115,-4.79763833485293,
1.32173683278195));
#46774=CARTESIAN_POINT('Ctrl Pts',(-27.8407397986575,-4.92117374333981,
0.662669505529257));
#46775=CARTESIAN_POINT('Ctrl Pts',(-27.8088415259036,-4.91810465358294,
0.00250400581179228));
#46776=CARTESIAN_POINT('Origin',(-14.75,0.,0.));
#46777=CARTESIAN_POINT('',(-26.0911584740964,-4.92036739665688,-0.00383377046079936));
#46778=CARTESIAN_POINT('',(-26.3088415259036,-4.92121007081632,-0.00410983607026229));
#46779=CARTESIAN_POINT('',(-14.75,-4.925,-6.03138548580071E-16));
#46780=CARTESIAN_POINT('Ctrl Pts',(-26.0911584740964,-4.92036739665688,
-0.00383377046079936));
#46781=CARTESIAN_POINT('Ctrl Pts',(-26.1441533704359,-4.91244432033151,
1.09173065983813));
#46782=CARTESIAN_POINT('Ctrl Pts',(-26.1971482667754,-4.55141276587038,
2.19203324705585));
#46783=CARTESIAN_POINT('Ctrl Pts',(-26.2501431631149,-3.87908362999679,
3.04775276608836));
#46784=CARTESIAN_POINT('Ctrl Pts',(-26.329689051488,-2.86991063247732,4.33219662844735));
#46785=CARTESIAN_POINT('Ctrl Pts',(-26.4092349398611,-1.15937419217738,
5.06558698769252));
#46786=CARTESIAN_POINT('Ctrl Pts',(-26.4887808282342,0.466768297211532,
4.91103020168458));
#46787=CARTESIAN_POINT('Ctrl Pts',(-26.5683267166072,2.09291078660044,4.75647341567663));
#46788=CARTESIAN_POINT('Ctrl Pts',(-26.6478726049803,3.63465932507832,3.71396948441558));
#46789=CARTESIAN_POINT('Ctrl Pts',(-26.7274184933534,4.38378843538607,2.26240825335668));
#46790=CARTESIAN_POINT('Ctrl Pts',(-26.8069643817264,5.13291754569381,0.810847022297775));
#46791=CARTESIAN_POINT('Ctrl Pts',(-26.8865102700995,5.08942722783144,-1.04977150855898));
#46792=CARTESIAN_POINT('Ctrl Pts',(-26.9660561584726,4.27329930907013,-2.46474911465105));
#46793=CARTESIAN_POINT('Ctrl Pts',(-27.0456020468457,3.45717139030882,-3.87972672074312));
#46794=CARTESIAN_POINT('Ctrl Pts',(-27.1251479352187,1.86840587064857,-4.84906340207051));
#46795=CARTESIAN_POINT('Ctrl Pts',(-27.2046938235918,0.236816482345431,
-4.92747617760022));
#46796=CARTESIAN_POINT('Ctrl Pts',(-27.2842397119649,-1.39477290595772,
-5.00588895312993));
#46797=CARTESIAN_POINT('Ctrl Pts',(-27.363785600338,-3.06918616290375,-4.19337782286196));
#46798=CARTESIAN_POINT('Ctrl Pts',(-27.4433314887111,-4.01724394449298,
-2.86319023358059));
#46799=CARTESIAN_POINT('Ctrl Pts',(-27.4926071505062,-4.60452979374673,
-2.03918945724775));
#46800=CARTESIAN_POINT('Ctrl Pts',(-27.5418828123013,-4.91308887859519,
-1.01653899859688));
#46801=CARTESIAN_POINT('Ctrl Pts',(-27.5911584740964,-4.91871916148224,
0.00298870709768639));
#46802=CARTESIAN_POINT('Ctrl Pts',(-27.8088415259036,-4.91810465358294,
0.00250400581179228));
#46803=CARTESIAN_POINT('Ctrl Pts',(-27.7611939102845,-4.91352024206437,
-0.983609324467926));
#46804=CARTESIAN_POINT('Ctrl Pts',(-27.7135462946653,-4.62644968879859,
-1.97217295080227));
#46805=CARTESIAN_POINT('Ctrl Pts',(-27.6658986790462,-4.07499817460332,
-2.78038834104901));
#46806=CARTESIAN_POINT('Ctrl Pts',(-27.5863527906731,-3.15437077234312,
-4.12967330271128));
#46807=CARTESIAN_POINT('Ctrl Pts',(-27.5068069023,-1.49688621586748,-4.97630902842222));
#46808=CARTESIAN_POINT('Ctrl Pts',(-27.427261013927,0.135976152639213,-4.93130021039854));
#46809=CARTESIAN_POINT('Ctrl Pts',(-27.3477151255539,1.7688385211459,-4.88629139237487));
#46810=CARTESIAN_POINT('Ctrl Pts',(-27.2681692371808,3.37707870168364,-3.9496380306166));
#46811=CARTESIAN_POINT('Ctrl Pts',(-27.1886233488077,4.22197683163389,-2.55164722242325));
#46812=CARTESIAN_POINT('Ctrl Pts',(-27.1090774604347,5.06687496158415,-1.1536564142299));
#46813=CARTESIAN_POINT('Ctrl Pts',(-27.0295315720616,5.14843104094691,0.705671840398515));
#46814=CARTESIAN_POINT('Ctrl Pts',(-26.9499856836885,4.42915646105591,2.17225163970649));
#46815=CARTESIAN_POINT('Ctrl Pts',(-26.8704397953154,3.7098818811649,3.63883143901446));
#46816=CARTESIAN_POINT('Ctrl Pts',(-26.7908939069423,2.18977664202013,4.71266278300198));
#46817=CARTESIAN_POINT('Ctrl Pts',(-26.7113480185693,0.567134884896936,
4.90045492678425));
#46818=CARTESIAN_POINT('Ctrl Pts',(-26.6318021301962,-1.05550687222627,
5.08824707056651));
#46819=CARTESIAN_POINT('Ctrl Pts',(-26.5522562418232,-2.7806851473279,4.39000001414349));
#46820=CARTESIAN_POINT('Ctrl Pts',(-26.4727103534501,-3.81592225162572,
3.12646916519825));
#46821=CARTESIAN_POINT('Ctrl Pts',(-26.4180874109346,-4.52680370627415,
2.25882189467213));
#46822=CARTESIAN_POINT('Ctrl Pts',(-26.3634644684191,-4.91235316928586,
1.12462305447093));
#46823=CARTESIAN_POINT('Ctrl Pts',(-26.3088415259036,-4.92121007081632,
-0.00410983607026228));
#46824=CARTESIAN_POINT('Origin',(-14.75,0.,0.));
#46825=CARTESIAN_POINT('',(-24.5911584740964,-4.93264761214373,-0.00145024765580815));
#46826=CARTESIAN_POINT('',(-24.8088415259036,-4.93298564037245,-0.000844910194652536));
#46827=CARTESIAN_POINT('',(-14.75,-4.925,-6.03138548580071E-16));
#46828=CARTESIAN_POINT('Ctrl Pts',(-24.5911584740964,-4.93264761214373,
-0.00145024765580815));
#46829=CARTESIAN_POINT('Ctrl Pts',(-24.6668780401975,-4.9266177416151,1.55388178409041));
#46830=CARTESIAN_POINT('Ctrl Pts',(-24.7425976062985,-4.12958481778531,
3.11453421006534));
#46831=CARTESIAN_POINT('Ctrl Pts',(-24.8183171723996,-2.86343383037207,
4.01706799645064));
#46832=CARTESIAN_POINT('Ctrl Pts',(-24.8978630607726,-1.53330067860747,
4.96520934909558));
#46833=CARTESIAN_POINT('Ctrl Pts',(-24.9774089491457,0.314560165826125,
5.18703834835445));
#46834=CARTESIAN_POINT('Ctrl Pts',(-25.0569548375188,1.83130840270388,4.58065477546433));
#46835=CARTESIAN_POINT('Ctrl Pts',(-25.1365007258919,3.34805663958163,3.9742712025742));
#46836=CARTESIAN_POINT('Ctrl Pts',(-25.2160466142649,4.53369226890353,2.5396750575351));
#46837=CARTESIAN_POINT('Ctrl Pts',(-25.295592502638,4.84357719847932,0.935867858373788));
#46838=CARTESIAN_POINT('Ctrl Pts',(-25.3751383910111,5.15346212805511,-0.667939340787529));
#46839=CARTESIAN_POINT('Ctrl Pts',(-25.4546842793842,4.58759635788477,-2.44095759407106));
#46840=CARTESIAN_POINT('Ctrl Pts',(-25.5342301677572,3.40591819971526,-3.56872660483793));
#46841=CARTESIAN_POINT('Ctrl Pts',(-25.6137760561303,2.22424004154574,-4.69649561560481));
#46842=CARTESIAN_POINT('Ctrl Pts',(-25.6933219445034,0.426749495377071,
-5.17901538385504));
#46843=CARTESIAN_POINT('Ctrl Pts',(-25.7728678328765,-1.16085155874105,
-4.79463371383198));
#46844=CARTESIAN_POINT('Ctrl Pts',(-25.8524137212495,-2.74845261285917,
-4.41025204380892));
#46845=CARTESIAN_POINT('Ctrl Pts',(-25.9319596096226,-4.12616417492674,
-3.15896893551255));
#46846=CARTESIAN_POINT('Ctrl Pts',(-26.0115054979957,-4.661115178591,-1.61557869862796));
#46847=CARTESIAN_POINT('Ctrl Pts',(-26.0380564900293,-4.83967223700271,
-1.10042269594398));
#46848=CARTESIAN_POINT('Ctrl Pts',(-26.0646074820628,-4.92433693997005,
-0.552722898855101));
#46849=CARTESIAN_POINT('Ctrl Pts',(-26.0911584740964,-4.92036739665688,
-0.00383377046079936));
#46850=CARTESIAN_POINT('Ctrl Pts',(-26.3088415259036,-4.92121007081632,
-0.00410983607026228));
#46851=CARTESIAN_POINT('Ctrl Pts',(-26.283918580046,-4.92525123130941,-0.519119599791246));
#46852=CARTESIAN_POINT('Ctrl Pts',(-26.2589956341884,-4.85087080801869,
-1.03299143706225));
#46853=CARTESIAN_POINT('Ctrl Pts',(-26.2340726883308,-4.69319011704004,
-1.5198867036229));
#46854=CARTESIAN_POINT('Ctrl Pts',(-26.1545267999577,-4.18992494466251,
-3.07389708203135));
#46855=CARTESIAN_POINT('Ctrl Pts',(-26.0749809115847,-2.83809866641343,
-4.35310319738077));
#46856=CARTESIAN_POINT('Ctrl Pts',(-25.9954350232116,-1.25869311650182,
-4.76988247643117));
#46857=CARTESIAN_POINT('Ctrl Pts',(-25.9158891348386,0.320712433409791,
-5.18666175548156));
#46858=CARTESIAN_POINT('Ctrl Pts',(-25.8363432464654,2.12769725498392,-4.74101419823293));
#46859=CARTESIAN_POINT('Ctrl Pts',(-25.7567973580924,3.33219893892002,-3.63765499595275));
#46860=CARTESIAN_POINT('Ctrl Pts',(-25.6772514697193,4.53670062285612,-2.53429579367258));
#46861=CARTESIAN_POINT('Ctrl Pts',(-25.5977055813462,5.13871916915418,-0.773224946360884));
#46862=CARTESIAN_POINT('Ctrl Pts',(-25.5181596929732,4.86170857536212,0.836585847286859));
#46863=CARTESIAN_POINT('Ctrl Pts',(-25.4386138046001,4.58469798157006,2.44639664093459));
#46864=CARTESIAN_POINT('Ctrl Pts',(-25.359067916227,3.4286582476879,3.90494738091836));
#46865=CARTESIAN_POINT('Ctrl Pts',(-25.2795220278539,1.92463240018136,4.54223247168555));
#46866=CARTESIAN_POINT('Ctrl Pts',(-25.1999761394808,0.420606552674816,
5.17951756245273));
#46867=CARTESIAN_POINT('Ctrl Pts',(-25.1204302511078,-1.43140540845612,
4.99553700400332));
#46868=CARTESIAN_POINT('Ctrl Pts',(-25.0408843627347,-2.78065642310143,
4.07480491924754));
#46869=CARTESIAN_POINT('Ctrl Pts',(-24.9635367504577,-4.09262045392238,
3.17951756047544));
#46870=CARTESIAN_POINT('Ctrl Pts',(-24.8861891381806,-4.92922749371504,
1.58763673888852));
#46871=CARTESIAN_POINT('Ctrl Pts',(-24.8088415259036,-4.93298564037245,
-0.000844910194652536));
#46872=CARTESIAN_POINT('Origin',(-14.75,0.,0.));
#46873=CARTESIAN_POINT('',(-23.0911584740964,-4.92477578693879,0.00455121266192807));
#46874=CARTESIAN_POINT('',(-23.3088415259036,-4.92376359828451,0.00452755087589233));
#46875=CARTESIAN_POINT('',(-14.75,-4.925,-6.03138548580071E-16));
#46876=CARTESIAN_POINT('Ctrl Pts',(-23.0911584740964,-4.92477578693879,
0.00455121266192807));
#46877=CARTESIAN_POINT('Ctrl Pts',(-23.1100568215859,-4.92836778419939,
0.39435127717714));
#46878=CARTESIAN_POINT('Ctrl Pts',(-23.1289551690754,-4.88600126774917,
0.783379637951124));
#46879=CARTESIAN_POINT('Ctrl Pts',(-23.147853516565,-4.7947032911263,1.1605640760821));
#46880=CARTESIAN_POINT('Ctrl Pts',(-23.227399404938,-4.41041685226391,2.74818813835895));
#46881=CARTESIAN_POINT('Ctrl Pts',(-23.3069452933111,-3.15921646993337,
4.12597456962399));
#46882=CARTESIAN_POINT('Ctrl Pts',(-23.3864911816842,-1.6158582674624,4.66101820240316));
#46883=CARTESIAN_POINT('Ctrl Pts',(-23.4660370700573,-0.0725000649914348,
5.19606183518233));
#46884=CARTESIAN_POINT('Ctrl Pts',(-23.5455829584304,1.76301595761996,4.88836266947564));
#46885=CARTESIAN_POINT('Ctrl Pts',(-23.6251288468034,3.04752024302872,3.87926655341467));
#46886=CARTESIAN_POINT('Ctrl Pts',(-23.7046747351765,4.33202452843749,2.87017043735369));
#46887=CARTESIAN_POINT('Ctrl Pts',(-23.7842206235496,5.06551707664363,1.1596773709384));
#46888=CARTESIAN_POINT('Ctrl Pts',(-23.8637665119226,4.91105798552202,-0.46647410387683));
#46889=CARTESIAN_POINT('Ctrl Pts',(-23.9433124002957,4.75659889440041,-2.09262557869207));
#46890=CARTESIAN_POINT('Ctrl Pts',(-24.0228582886688,3.71418816395107,-3.63443546190725));
#46891=CARTESIAN_POINT('Ctrl Pts',(-24.1024041770419,2.26267151748941,-4.38365215585762));
#46892=CARTESIAN_POINT('Ctrl Pts',(-24.181950065415,0.811154871027751,-5.132868849808));
#46893=CARTESIAN_POINT('Ctrl Pts',(-24.261495953788,-1.04946769144621,-5.08949235449356));
#46894=CARTESIAN_POINT('Ctrl Pts',(-24.3410418421611,-2.4644935804178,-4.2734482583492));
#46895=CARTESIAN_POINT('Ctrl Pts',(-24.4205877305342,-3.87951946938938,
-3.45740416220484));
#46896=CARTESIAN_POINT('Ctrl Pts',(-24.5001336189073,-4.84894868485859,
-1.86869246523057));
#46897=CARTESIAN_POINT('Ctrl Pts',(-24.5796795072803,-4.92746056304542,
-0.237109763727941));
#46898=CARTESIAN_POINT('Ctrl Pts',(-24.5835058295524,-4.93123714728213,
-0.158627250588653));
#46899=CARTESIAN_POINT('Ctrl Pts',(-24.5873321518244,-4.93295231843154,
-0.0800455421075516));
#46900=CARTESIAN_POINT('Ctrl Pts',(-24.5911584740964,-4.93264761214373,
-0.00145024765580815));
#46901=CARTESIAN_POINT('Ctrl Pts',(-24.8088415259036,-4.93298564037245,
-0.000844910194652536));
#46902=CARTESIAN_POINT('Ctrl Pts',(-24.8066432498076,-4.93309244966778,
-0.0459907283445572));
#46903=CARTESIAN_POINT('Ctrl Pts',(-24.8044449737115,-4.93252653505162,
-0.0911338008527958));
#46904=CARTESIAN_POINT('Ctrl Pts',(-24.8022466976155,-4.93127968975541,
-0.136258058327248));
#46905=CARTESIAN_POINT('Ctrl Pts',(-24.7227008092424,-4.88616187360439,
-1.76910534008413));
#46906=CARTESIAN_POINT('Ctrl Pts',(-24.6431549208693,-3.94943617314267,
-3.37731629253574));
#46907=CARTESIAN_POINT('Ctrl Pts',(-24.5636090324963,-2.55140047284839,
-4.22213703896742));
#46908=CARTESIAN_POINT('Ctrl Pts',(-24.4840631441232,-1.15336477255412,
-5.06695778539909));
#46909=CARTESIAN_POINT('Ctrl Pts',(-24.4045172557501,0.705980927572705,
-5.14838832581082));
#46910=CARTESIAN_POINT('Ctrl Pts',(-24.324971367377,2.17252059826335,-4.42902243726831));
#46911=CARTESIAN_POINT('Ctrl Pts',(-24.2454254790039,3.63906026895399,-3.70965654872581));
#46912=CARTESIAN_POINT('Ctrl Pts',(-24.1658795906309,4.71279391020846,-2.18949423122905));
#46913=CARTESIAN_POINT('Ctrl Pts',(-24.0863337022578,4.90048718004666,-0.566842967216153));
#46914=CARTESIAN_POINT('Ctrl Pts',(-24.0067878138847,5.08818044988486,1.05580829679675));
#46915=CARTESIAN_POINT('Ctrl Pts',(-23.9272419255116,4.3898333483068,2.78094850732579));
#46916=CARTESIAN_POINT('Ctrl Pts',(-23.8476960371386,3.12624123694881,3.81611075100284));
#46917=CARTESIAN_POINT('Ctrl Pts',(-23.7681501487655,1.86264912559084,4.85127299467987));
#46918=CARTESIAN_POINT('Ctrl Pts',(-23.6886042603924,0.0338120044529563,
5.19645727150491));
#46919=CARTESIAN_POINT('Ctrl Pts',(-23.6090583720193,-1.52016861672953,
4.69309843356272));
#46920=CARTESIAN_POINT('Ctrl Pts',(-23.5295124836463,-3.07414923791204,
4.18973959562053));
#46921=CARTESIAN_POINT('Ctrl Pts',(-23.4499665952732,-4.35327335913915,
2.83783764291109));
#46922=CARTESIAN_POINT('Ctrl Pts',(-23.3704207069001,-4.76995770197036,
1.25840735017577));
#46923=CARTESIAN_POINT('Ctrl Pts',(-23.3498943132346,-4.8774808817366,0.850843758656771));
#46924=CARTESIAN_POINT('Ctrl Pts',(-23.3293679195691,-4.92757673294028,
0.428129724095519));
#46925=CARTESIAN_POINT('Ctrl Pts',(-23.3088415259036,-4.92376359828451,
0.00452755087589233));
#46926=CARTESIAN_POINT('Origin',(-14.75,0.,0.));
#46927=CARTESIAN_POINT('',(-21.5911584740964,-4.91693164693359,-0.000632398697534842));
#46928=CARTESIAN_POINT('',(-21.8088415259036,-4.91711569616659,-0.00117946379282014));
#46929=CARTESIAN_POINT('',(-14.75,-4.925,-6.03138548580071E-16));
#46930=CARTESIAN_POINT('Ctrl Pts',(-21.5911584740964,-4.91693164693359,
-0.000632398697534842));
#46931=CARTESIAN_POINT('Ctrl Pts',(-21.6327814913475,-4.91594750340395,
0.861347871439622));
#46932=CARTESIAN_POINT('Ctrl Pts',(-21.6744045085985,-4.70055318639053,
1.72378817794021));
#46933=CARTESIAN_POINT('Ctrl Pts',(-21.7160275258496,-4.27359604091789,
2.46423730661521));
#46934=CARTESIAN_POINT('Ctrl Pts',(-21.7955734142227,-3.4576368030521,3.87931212880427));
#46935=CARTESIAN_POINT('Ctrl Pts',(-21.8751193025958,-1.86898324578976,
4.84883661113057));
#46936=CARTESIAN_POINT('Ctrl Pts',(-21.9546651909688,-0.237405254457672,
4.92744633348781));
#46937=CARTESIAN_POINT('Ctrl Pts',(-22.0342110793419,1.39417273687441,5.00605605584506));
#46938=CARTESIAN_POINT('Ctrl Pts',(-22.113756967715,3.06867516227623,4.19375101823326));
#46939=CARTESIAN_POINT('Ctrl Pts',(-22.1933028560881,4.01689627682146,2.86367472410927));
#46940=CARTESIAN_POINT('Ctrl Pts',(-22.2728487444611,4.9651173913667,1.53359842998527));
#46941=CARTESIAN_POINT('Ctrl Pts',(-22.3523946328342,5.18705719505533,-0.314249120650923));
#46942=CARTESIAN_POINT('Ctrl Pts',(-22.4319405212073,4.58076458321006,-1.83103371282965));
#46943=CARTESIAN_POINT('Ctrl Pts',(-22.5114864095804,3.97447197136479,-3.34781830500836));
#46944=CARTESIAN_POINT('Ctrl Pts',(-22.5910322979534,2.53994694398564,-4.5335399387296));
#46945=CARTESIAN_POINT('Ctrl Pts',(-22.6705781863265,0.936158324065459,
-4.84352105564377));
#46946=CARTESIAN_POINT('Ctrl Pts',(-22.7501240746996,-0.667630295854733,
-5.15350217255794));
#46947=CARTESIAN_POINT('Ctrl Pts',(-22.8296699630727,-2.44068250831595,
-4.58774277266501));
#46948=CARTESIAN_POINT('Ctrl Pts',(-22.9092158514458,-3.56852236684944,
-3.40613222607422));
#46949=CARTESIAN_POINT('Ctrl Pts',(-22.9698633923293,-4.42841236656523,
-2.50524626705758));
#46950=CARTESIAN_POINT('Ctrl Pts',(-23.0305109332129,-4.9132485462191,-1.24637378817277));
#46951=CARTESIAN_POINT('Ctrl Pts',(-23.0911584740964,-4.92477578693879,
0.00455121266192807));
#46952=CARTESIAN_POINT('Ctrl Pts',(-23.3088415259036,-4.92376359828451,
0.00452755087589233));
#46953=CARTESIAN_POINT('Ctrl Pts',(-23.249822031196,-4.9127997005681,-1.2134548491438));
#46954=CARTESIAN_POINT('Ctrl Pts',(-23.1908025364885,-4.4561520233695,-2.43877979118426));
#46955=CARTESIAN_POINT('Ctrl Pts',(-23.1317830417809,-3.63745529283231,
-3.33241721991151));
#46956=CARTESIAN_POINT('Ctrl Pts',(-23.0522371534078,-2.53402397642775,
-4.53685286450225));
#46957=CARTESIAN_POINT('Ctrl Pts',(-22.9726912650347,-0.77291677918332,
-5.13876552092253));
#46958=CARTESIAN_POINT('Ctrl Pts',(-22.8931453766617,0.83687745995922,-4.86165832319329));
#46959=CARTESIAN_POINT('Ctrl Pts',(-22.8135994882886,2.44667169910178,-4.58455112546405));
#46960=CARTESIAN_POINT('Ctrl Pts',(-22.7340535999155,3.90515298014245,-3.42842407358526));
#46961=CARTESIAN_POINT('Ctrl Pts',(-22.6545077115424,4.5423478449547,-1.92436004709929));
#46962=CARTESIAN_POINT('Ctrl Pts',(-22.5749618231694,5.17954270976695,-0.42029602061334));
#46963=CARTESIAN_POINT('Ctrl Pts',(-22.4954159347963,4.9954511583508,1.43170498047977));
#46964=CARTESIAN_POINT('Ctrl Pts',(-22.4158700464232,4.07463817966522,2.78090079647325));
#46965=CARTESIAN_POINT('Ctrl Pts',(-22.3363241580501,3.15382520097963,4.13009661246674));
#46966=CARTESIAN_POINT('Ctrl Pts',(-22.2567782696771,1.4962907950246,4.97648724336059));
#46967=CARTESIAN_POINT('Ctrl Pts',(-22.177232381304,-0.136553786680188,
4.93127149915006));
#46968=CARTESIAN_POINT('Ctrl Pts',(-22.0976864929309,-1.76939836838497,
4.88605575493953));
#46969=CARTESIAN_POINT('Ctrl Pts',(-22.0181406045578,-3.37755312583951,
3.94923363562461));
#46970=CARTESIAN_POINT('Ctrl Pts',(-21.9385947161848,-4.22229002887781,
2.55114728056903));
#46971=CARTESIAN_POINT('Ctrl Pts',(-21.8953436527577,-4.68159433887712,
1.79097321179257));
#46972=CARTESIAN_POINT('Ctrl Pts',(-21.8520925893307,-4.91520443767987,
0.894432581458181));
#46973=CARTESIAN_POINT('Ctrl Pts',(-21.8088415259036,-4.91711569616659,
-0.00117946379282014));
#46974=CARTESIAN_POINT('Origin',(-14.75,0.,0.));
#46975=CARTESIAN_POINT('',(-20.0911584740964,-4.92710437571252,-0.00432825790191715));
#46976=CARTESIAN_POINT('',(-20.3088415259036,-4.92810468982102,-0.00410855472338207));
#46977=CARTESIAN_POINT('',(-14.75,-4.925,-6.03138548580071E-16));
#46978=CARTESIAN_POINT('Ctrl Pts',(-20.0911584740964,-4.92710437571252,
-0.00432825790191715));
#46979=CARTESIAN_POINT('Ctrl Pts',(-20.155506161109,-4.91490963574447,1.32130828947872));
#46980=CARTESIAN_POINT('Ctrl Pts',(-20.2198538481216,-4.36214110397647,
2.65590833175386));
#46981=CARTESIAN_POINT('Ctrl Pts',(-20.2842015351343,-3.40634621717809,
3.56831810142706));
#46982=CARTESIAN_POINT('Ctrl Pts',(-20.3637474235073,-2.22480330705116,
4.69622881676794));
#46983=CARTESIAN_POINT('Ctrl Pts',(-20.4432933118804,-0.427370559254853,
5.1789641106682));
#46984=CARTESIAN_POINT('Ctrl Pts',(-20.5228392002535,1.16027654508549,4.79477287920708));
#46985=CARTESIAN_POINT('Ctrl Pts',(-20.6023850886266,2.74792364942585,4.41058164774596));
#46986=CARTESIAN_POINT('Ctrl Pts',(-20.6819309769996,4.12578511031025,3.15946389092347));
#46987=CARTESIAN_POINT('Ctrl Pts',(-20.7614768653727,4.66092129423408,1.61613777667943));
#46988=CARTESIAN_POINT('Ctrl Pts',(-20.8410227537458,5.19605747815791,0.0728116624353919));
#46989=CARTESIAN_POINT('Ctrl Pts',(-20.9205686421189,4.88846838512118,-1.76272280923018));
#46990=CARTESIAN_POINT('Ctrl Pts',(-21.0001145304919,3.87944930013121,-3.04728760571889));
#46991=CARTESIAN_POINT('Ctrl Pts',(-21.079660418865,2.87043021514126,-4.33185240220757));
#46992=CARTESIAN_POINT('Ctrl Pts',(-21.1592063072381,1.1599811381981,-5.06544752351941));
#46993=CARTESIAN_POINT('Ctrl Pts',(-21.2387521956112,-0.466179596436317,
-4.91108594998304));
#46994=CARTESIAN_POINT('Ctrl Pts',(-21.3182980839842,-2.09234033107078,
-4.75672437644668));
#46995=CARTESIAN_POINT('Ctrl Pts',(-21.3978439723573,-3.6342127233965,-3.71440610806206));
#46996=CARTESIAN_POINT('Ctrl Pts',(-21.4773898607304,-4.38351646032473,
-2.26293439284383));
#46997=CARTESIAN_POINT('Ctrl Pts',(-21.5153127318524,-4.74074107152647,
-1.57095676937065));
#46998=CARTESIAN_POINT('Ctrl Pts',(-21.5532356029744,-4.9178283034161,-0.785985524275935));
#46999=CARTESIAN_POINT('Ctrl Pts',(-21.5911584740964,-4.91693164693359,
-0.000632398697534842));
#47000=CARTESIAN_POINT('Ctrl Pts',(-21.8088415259036,-4.91711569616659,
-0.00117946379282014));
#47001=CARTESIAN_POINT('Ctrl Pts',(-21.7725467009576,-4.91871955944082,
-0.752746704602252));
#47002=CARTESIAN_POINT('Ctrl Pts',(-21.7362518760116,-4.75716117024752,
-1.50366003608004));
#47003=CARTESIAN_POINT('Ctrl Pts',(-21.6999570510655,-4.42889215011132,
-2.17278619696736));
#47004=CARTESIAN_POINT('Ctrl Pts',(-21.6204111626925,-3.70943831968447,
-3.63928272865185));
#47005=CARTESIAN_POINT('Ctrl Pts',(-21.5408652743194,-2.18921161020874,
-4.71292520122458));
#47006=CARTESIAN_POINT('Ctrl Pts',(-21.4613193859463,-0.566549092315044,
-4.90052116218762));
#47007=CARTESIAN_POINT('Ctrl Pts',(-21.3817734975732,1.05611342557867,-5.08811712315067));
#47008=CARTESIAN_POINT('Ctrl Pts',(-21.3022276092002,2.78121175189034,-4.38966657250399));
#47009=CARTESIAN_POINT('Ctrl Pts',(-21.2226817208271,3.81629821795521,-3.12601238748351));
#47010=CARTESIAN_POINT('Ctrl Pts',(-21.143135832454,4.85138468402006,-1.86235820246306));
#47011=CARTESIAN_POINT('Ctrl Pts',(-21.0635899440809,5.19645928983812,-0.0335003830688158));
#47012=CARTESIAN_POINT('Ctrl Pts',(-20.9840440557079,4.69300726397856,1.52045005024925));
#47013=CARTESIAN_POINT('Ctrl Pts',(-20.9044981673348,4.189555238119,3.07440048356732));
#47014=CARTESIAN_POINT('Ctrl Pts',(-20.8249522789617,2.83757658058181,4.35344353080922));
#47015=CARTESIAN_POINT('Ctrl Pts',(-20.7454063905886,1.25812130277897,4.77003315738511));
#47016=CARTESIAN_POINT('Ctrl Pts',(-20.6658605022155,-0.321333975023885,
5.186622783961));
#47017=CARTESIAN_POINT('Ctrl Pts',(-20.5863146138425,-2.1282658730924,4.74075898987086));
#47018=CARTESIAN_POINT('Ctrl Pts',(-20.5067687254694,-3.33263534483166,
3.63725544792229));
#47019=CARTESIAN_POINT('Ctrl Pts',(-20.4407929922808,-4.33154503775366,
2.72200443061253));
#47020=CARTESIAN_POINT('Ctrl Pts',(-20.3748172590922,-4.91594471882842,
1.3543550430017));
#47021=CARTESIAN_POINT('Ctrl Pts',(-20.3088415259036,-4.92810468982102,
-0.00410855472338207));
#47022=CARTESIAN_POINT('Origin',(-14.75,0.,0.));
#47023=CARTESIAN_POINT('',(-18.5911584740964,-4.93133925263252,0.00269369058761092));
#47024=CARTESIAN_POINT('',(-18.8088415259036,-4.93057297854711,0.00316028518611533));
#47025=CARTESIAN_POINT('',(-14.75,-4.925,-6.03138548580071E-16));
#47026=CARTESIAN_POINT('Ctrl Pts',(-18.5911584740964,-4.93133925263252,
0.00269369058761092));
#47027=CARTESIAN_POINT('Ctrl Pts',(-18.5986849424975,-4.93235666587827,
0.157401246761113));
#47028=CARTESIAN_POINT('Ctrl Pts',(-18.6062114108986,-4.92571004477723,
0.312020226781154));
#47029=CARTESIAN_POINT('Ctrl Pts',(-18.6137378792997,-4.91111389702246,
0.465885087471429));
#47030=CARTESIAN_POINT('Ctrl Pts',(-18.6932837676727,-4.75684984141161,
2.0920550759408));
#47031=CARTESIAN_POINT('Ctrl Pts',(-18.7728296560458,-3.7146240379434,3.63398997126305));
#47032=CARTESIAN_POINT('Ctrl Pts',(-18.8523755444189,-2.26319725960073,
4.3833807487362));
#47033=CARTESIAN_POINT('Ctrl Pts',(-18.931921432792,-0.811770481258054,
5.13277152620935));
#47034=CARTESIAN_POINT('Ctrl Pts',(-19.0114673211651,1.04885727195908,5.08961818583339));
#47035=CARTESIAN_POINT('Ctrl Pts',(-19.0910132095381,2.46398102306833,4.27374380867811));
#47036=CARTESIAN_POINT('Ctrl Pts',(-19.1705590979112,3.87910477417757,3.45786943152285));
#47037=CARTESIAN_POINT('Ctrl Pts',(-19.2501049862843,4.84872452317893,1.86927401758828));
#47038=CARTESIAN_POINT('Ctrl Pts',(-19.3296508746573,4.92743208790438,0.237700743258566));
#47039=CARTESIAN_POINT('Ctrl Pts',(-19.4091967630304,5.00613965262983,-1.39387253107114));
#47040=CARTESIAN_POINT('Ctrl Pts',(-19.4887426514035,4.19393503307937,-3.068423665796));
#47041=CARTESIAN_POINT('Ctrl Pts',(-19.5682885397766,2.86391560429619,-4.01672454068289));
#47042=CARTESIAN_POINT('Ctrl Pts',(-19.6478344281497,1.53389617551299,-4.9650254155698));
#47043=CARTESIAN_POINT('Ctrl Pts',(-19.7273803165227,-0.313938062502946,
-5.18707603061872));
#47044=CARTESIAN_POINT('Ctrl Pts',(-19.8069262048958,-1.8307590101278,-4.58087437844472));
#47045=CARTESIAN_POINT('Ctrl Pts',(-19.8864720932689,-3.34757995775264,
-3.97467272627071));
#47046=CARTESIAN_POINT('Ctrl Pts',(-19.9660179816419,-4.5333876149864,-2.54021880687379));
#47047=CARTESIAN_POINT('Ctrl Pts',(-20.045563870015,-4.84346490737449,-0.936448778784566));
#47048=CARTESIAN_POINT('Ctrl Pts',(-20.0607620713755,-4.90270891386442,
-0.630029172173884));
#47049=CARTESIAN_POINT('Ctrl Pts',(-20.0759602727359,-4.92998463640529,
-0.317428729934899));
#47050=CARTESIAN_POINT('Ctrl Pts',(-20.0911584740964,-4.92710437571252,
-0.00432825790191715));
#47051=CARTESIAN_POINT('Ctrl Pts',(-20.3088415259036,-4.92810468982102,
-0.00410855472338207));
#47052=CARTESIAN_POINT('Ctrl Pts',(-20.2952713707191,-4.93060580175162,
-0.283522832407918));
#47053=CARTESIAN_POINT('Ctrl Pts',(-20.2817012155346,-4.90889778438975,
-0.562548496769959));
#47054=CARTESIAN_POINT('Ctrl Pts',(-20.2681310603502,-4.86160812861449,
-0.837169002561447));
#47055=CARTESIAN_POINT('Ctrl Pts',(-20.1885851719771,-4.58440439524805,
-2.44694662128967));
#47056=CARTESIAN_POINT('Ctrl Pts',(-20.109039283604,-3.42818988310517,-3.90535856893913));
#47057=CARTESIAN_POINT('Ctrl Pts',(-20.0294933952309,-1.9240876479818,-4.54246323682914));
#47058=CARTESIAN_POINT('Ctrl Pts',(-19.9499475068579,-0.419985412858412,
-5.17956790471916));
#47059=CARTESIAN_POINT('Ctrl Pts',(-19.8704016184848,1.43200454524547,-4.9953652928497));
#47060=CARTESIAN_POINT('Ctrl Pts',(-19.7908557301117,2.78114513946445,-4.07447140722498));
#47061=CARTESIAN_POINT('Ctrl Pts',(-19.7113098417387,4.13028573368341,-3.15357752160028));
#47062=CARTESIAN_POINT('Ctrl Pts',(-19.6317639533656,4.97657696401748,-1.49599236222033));
#47063=CARTESIAN_POINT('Ctrl Pts',(-19.5522180649925,4.93126330142958,0.136849505056872));
#47064=CARTESIAN_POINT('Ctrl Pts',(-19.4726721766194,4.88594963884169,1.76969137233409));
#47065=CARTESIAN_POINT('Ctrl Pts',(-19.3931262882463,3.94903108333184,3.37778994750857));
#47066=CARTESIAN_POINT('Ctrl Pts',(-19.3135803998733,2.55089407358275,4.22244300854623));
#47067=CARTESIAN_POINT('Ctrl Pts',(-19.2340345115002,1.15275706383363,5.06709606958391));
#47068=CARTESIAN_POINT('Ctrl Pts',(-19.1544886231271,-0.706598400154735,
5.14830361648474));
#47069=CARTESIAN_POINT('Ctrl Pts',(-19.074942734754,-2.17305178497508,4.42876184445237));
#47070=CARTESIAN_POINT('Ctrl Pts',(-18.995396846381,-3.63950516979541,3.70922007242002));
#47071=CARTESIAN_POINT('Ctrl Pts',(-18.9158509580079,-4.71305647544771,
2.18892898145449));
#47072=CARTESIAN_POINT('Ctrl Pts',(-18.8363050696348,-4.90055512820742,
0.566255216718109));
#47073=CARTESIAN_POINT('Ctrl Pts',(-18.8271505550577,-4.92213335412174,
0.379510295806119));
#47074=CARTESIAN_POINT('Ctrl Pts',(-18.8179960404807,-4.93197626646748,
0.191409368818455));
#47075=CARTESIAN_POINT('Ctrl Pts',(-18.8088415259036,-4.93057297854711,
0.00316028518611533));
#47076=CARTESIAN_POINT('Origin',(-14.75,0.,0.));
#47077=CARTESIAN_POINT('',(-17.0911584740964,-4.91873477802609,0.00299898967114021));
#47078=CARTESIAN_POINT('',(-17.3088415259036,-4.91816086074912,0.00255430743475421));
#47079=CARTESIAN_POINT('',(-14.75,-4.925,-6.03138548580071E-16));
#47080=CARTESIAN_POINT('Ctrl Pts',(-17.0911584740964,-4.91873477802609,
0.00299898967114021));
#47081=CARTESIAN_POINT('Ctrl Pts',(-17.121409612259,-4.92219933969977,0.628902743871938));
#47082=CARTESIAN_POINT('Ctrl Pts',(-17.1516607504217,-4.81148680932676,
1.25362658234333));
#47083=CARTESIAN_POINT('Ctrl Pts',(-17.1819118885843,-4.58098415721058,
1.83048430084528));
#47084=CARTESIAN_POINT('Ctrl Pts',(-17.2614577769574,-3.97487346688356,
3.34734159845876));
#47085=CARTESIAN_POINT('Ctrl Pts',(-17.3410036653305,-2.54049066060951,
4.53323527492929));
#47086=CARTESIAN_POINT('Ctrl Pts',(-17.4205495537035,-0.936739230126934,
4.84340874168148));
#47087=CARTESIAN_POINT('Ctrl Pts',(-17.5000954420766,0.667012200355664,
5.15358220843367));
#47088=CARTESIAN_POINT('Ctrl Pts',(-17.5796413304497,2.44013225504679,4.58803546546751));
#47089=CARTESIAN_POINT('Ctrl Pts',(-17.6591872188228,3.56811382315476,3.40656019604341));
#47090=CARTESIAN_POINT('Ctrl Pts',(-17.7387331071958,4.69609539126271,2.22508492661932));
#47091=CARTESIAN_POINT('Ctrl Pts',(-17.8182789955689,5.17893847278751,0.427681130737319));
#47092=CARTESIAN_POINT('Ctrl Pts',(-17.897824883942,4.79484245007892,-1.15998900993782));
#47093=CARTESIAN_POINT('Ctrl Pts',(-17.9773707723151,4.41074642737033,-2.74765915061299));
#47094=CARTESIAN_POINT('Ctrl Pts',(-18.0569166606881,3.15971130042833,-4.12559563608129));
#47095=CARTESIAN_POINT('Ctrl Pts',(-18.1364625490612,1.61641728001955,-4.66082436926233));
#47096=CARTESIAN_POINT('Ctrl Pts',(-18.2160084374343,0.0731232596108,-5.19605310244336));
#47097=CARTESIAN_POINT('Ctrl Pts',(-18.2955543258074,-1.76242965426471,
-4.88857408333716));
#47098=CARTESIAN_POINT('Ctrl Pts',(-18.3751002141804,-3.04705495732574,
-3.87963203297581));
#47099=CARTESIAN_POINT('Ctrl Pts',(-18.4471196341524,-4.21013165556918,
-2.96615400490252));
#47100=CARTESIAN_POINT('Ctrl Pts',(-18.5191390541244,-4.92160380860666,
-1.47767503842927));
#47101=CARTESIAN_POINT('Ctrl Pts',(-18.5911584740964,-4.93133925263252,
0.00269369058761092));
#47102=CARTESIAN_POINT('Ctrl Pts',(-18.8088415259036,-4.93057297854711,
0.00316028518611533));
#47103=CARTESIAN_POINT('Ctrl Pts',(-18.7384501521076,-4.91978274344346,
-1.4443344455465));
#47104=CARTESIAN_POINT('Ctrl Pts',(-18.6680587783116,-4.24406537670826,
-2.90058887915162));
#47105=CARTESIAN_POINT('Ctrl Pts',(-18.5976674045156,-3.12578352599411,
-3.8164856718825));
#47106=CARTESIAN_POINT('Ctrl Pts',(-18.5181215161425,-1.86206727115392,
-4.85149635723954));
#47107=CARTESIAN_POINT('Ctrl Pts',(-18.4385756277694,-0.0331887616064278,
-5.19646128944632));
#47108=CARTESIAN_POINT('Ctrl Pts',(-18.3590297393964,1.52073147789346,-4.69291607715336));
#47109=CARTESIAN_POINT('Ctrl Pts',(-18.2794838510233,3.07465171739332,-4.18937086486042));
#47110=CARTESIAN_POINT('Ctrl Pts',(-18.1999379626502,4.35361368684558,-2.83731550806776));
#47111=CARTESIAN_POINT('Ctrl Pts',(-18.1203920742771,4.77010859585846,-1.2578352510475));
#47112=CARTESIAN_POINT('Ctrl Pts',(-18.0408461859041,5.18660350487135,0.321645005972764));
#47113=CARTESIAN_POINT('Ctrl Pts',(-17.961300297531,4.74063135344486,2.12855016322063));
#47114=CARTESIAN_POINT('Ctrl Pts',(-17.8817544091579,3.63705558982148,3.33285345786593));
#47115=CARTESIAN_POINT('Ctrl Pts',(-17.8022085207848,2.53347982619808,4.53715675251125));
#47116=CARTESIAN_POINT('Ctrl Pts',(-17.7226626324118,0.772300450377784,
5.13885818455397));
#47117=CARTESIAN_POINT('Ctrl Pts',(-17.6431167440387,-0.837460542095409,
4.86155791650103));
#47118=CARTESIAN_POINT('Ctrl Pts',(-17.5635708556656,-2.44722153456857,
4.58425764844809));
#47119=CARTESIAN_POINT('Ctrl Pts',(-17.4840249672925,-3.90556414369463,
3.42795568029952));
#47120=CARTESIAN_POINT('Ctrl Pts',(-17.4044790789195,-4.5425786123982,1.92381524197179));
#47121=CARTESIAN_POINT('Ctrl Pts',(-17.3725998945808,-4.79787152683423,
1.32100884574773));
#47122=CARTESIAN_POINT('Ctrl Pts',(-17.3407207102422,-4.92124900075768,
0.662335296357207));
#47123=CARTESIAN_POINT('Ctrl Pts',(-17.3088415259036,-4.91816086074912,
0.00255430743475421));
#47124=CARTESIAN_POINT('Origin',(-14.75,0.,0.));
#47125=CARTESIAN_POINT('',(-15.5911584740964,-4.92035796642718,-0.00383015064837622));
#47126=CARTESIAN_POINT('',(-15.8088415259036,-4.92120003017842,-0.00410675641256026));
#47127=CARTESIAN_POINT('',(-14.75,-4.925,-6.03138548580071E-16));
#47128=CARTESIAN_POINT('Ctrl Pts',(-15.5911584740964,-4.92035796642718,
-0.00383015064837622));
#47129=CARTESIAN_POINT('Ctrl Pts',(-15.6441342820206,-4.9124462735778,1.09134504077847));
#47130=CARTESIAN_POINT('Ctrl Pts',(-15.6971100899448,-4.55169660768519,
2.19124987504687));
#47131=CARTESIAN_POINT('Ctrl Pts',(-15.750085897869,-3.87981475186871,3.04682229797494));
#47132=CARTESIAN_POINT('Ctrl Pts',(-15.829631786242,-2.87094973976422,4.33150810298851));
#47133=CARTESIAN_POINT('Ctrl Pts',(-15.9091776746151,-1.16058865962495,
5.06530836353102));
#47134=CARTESIAN_POINT('Ctrl Pts',(-15.9887235629882,0.465590576831222,
4.91114182640059));
#47135=CARTESIAN_POINT('Ctrl Pts',(-16.0682694513612,2.0917698132874,4.75697528927016));
#47136=CARTESIAN_POINT('Ctrl Pts',(-16.1478153397343,3.63376720606049,3.71484195446679));
#47137=CARTESIAN_POINT('Ctrl Pts',(-16.2273612281074,4.38324502138396,2.26346011821903));
#47138=CARTESIAN_POINT('Ctrl Pts',(-16.3069071164805,5.13272283670744,0.812078281971235));
#47139=CARTESIAN_POINT('Ctrl Pts',(-16.3864530048536,5.08968107458128,-1.04855205572096));
#47140=CARTESIAN_POINT('Ctrl Pts',(-16.4659988932266,4.27389156106992,-2.46372473066101));
#47141=CARTESIAN_POINT('Ctrl Pts',(-16.5455447815997,3.45810204755859,-3.87889740560104));
#47142=CARTESIAN_POINT('Ctrl Pts',(-16.6250906699728,1.86956478266209,-4.84861241778893));
#47143=CARTESIAN_POINT('Ctrl Pts',(-16.7046365583459,0.237996231203316,
-4.92741782460026));
#47144=CARTESIAN_POINT('Ctrl Pts',(-16.7841824467189,-1.39357232025546,
-5.00622323141159));
#47145=CARTESIAN_POINT('Ctrl Pts',(-16.863728335092,-3.06817215827651,-4.19411903284637));
#47146=CARTESIAN_POINT('Ctrl Pts',(-16.9432742234651,-4.01655279009705,
-2.86415647418555));
#47147=CARTESIAN_POINT('Ctrl Pts',(-16.9925689736755,-4.60426621320643,
-2.03997594821106));
#47148=CARTESIAN_POINT('Ctrl Pts',(-17.041863723886,-4.91308921515918,-1.01692194861672));
#47149=CARTESIAN_POINT('Ctrl Pts',(-17.0911584740964,-4.91873477802609,
0.00299898967114021));
#47150=CARTESIAN_POINT('Ctrl Pts',(-17.3088415259036,-4.91816086074912,
0.00255430743475421));
#47151=CARTESIAN_POINT('Ctrl Pts',(-17.2611748218691,-4.91354338201311,
-0.983969839246001));
#47152=CARTESIAN_POINT('Ctrl Pts',(-17.2135081178347,-4.62618522137736,
-1.9729699017009));
#47153=CARTESIAN_POINT('Ctrl Pts',(-17.1658414138002,-4.07430462011665,
-2.78138947246816));
#47154=CARTESIAN_POINT('Ctrl Pts',(-17.0862955254271,-3.15332983085048,
-4.13047484007342));
#47155=CARTESIAN_POINT('Ctrl Pts',(-17.0067496370541,-1.4956939240371,-4.97666666677702));
#47156=CARTESIAN_POINT('Ctrl Pts',(-16.927203748681,0.137145222933267,-4.93125508596819));
#47157=CARTESIAN_POINT('Ctrl Pts',(-16.8476578603079,1.76998436990362,-4.88584350515936));
#47158=CARTESIAN_POINT('Ctrl Pts',(-16.7681119719349,3.37802675703098,-3.94882851683809));
#47159=CARTESIAN_POINT('Ctrl Pts',(-16.6885660835618,4.2225959730343,-2.55064085742682));
#47160=CARTESIAN_POINT('Ctrl Pts',(-16.6090201951887,5.06716518903764,-1.15245319801552));
#47161=CARTESIAN_POINT('Ctrl Pts',(-16.5294743068156,5.14826123391693,0.706907132485781));
#47162=CARTESIAN_POINT('Ctrl Pts',(-16.4499284184425,4.42863152286466,2.17331736517013));
#47163=CARTESIAN_POINT('Ctrl Pts',(-16.3703825300695,3.7090018118124,3.63972759785445));
#47164=CARTESIAN_POINT('Ctrl Pts',(-16.2908366416964,2.18864634482861,4.71318773272181));
#47165=CARTESIAN_POINT('Ctrl Pts',(-16.2112907533233,0.565961339085978,
4.90058907660299));
#47166=CARTESIAN_POINT('Ctrl Pts',(-16.1317448649502,-1.05672366665665,
5.08799042048417));
#47167=CARTESIAN_POINT('Ctrl Pts',(-16.0521989765772,-2.78173821115814,
4.38933297337918));
#47168=CARTESIAN_POINT('Ctrl Pts',(-15.9726530882041,-3.81667311208576,
3.12555465326431));
#47169=CARTESIAN_POINT('Ctrl Pts',(-15.9180492341039,-4.52709869773482,
2.25804071360155));
#47170=CARTESIAN_POINT('Ctrl Pts',(-15.8634453800038,-4.91235438239858,
1.1242382374886));
#47171=CARTESIAN_POINT('Ctrl Pts',(-15.8088415259036,-4.92120003017842,
-0.00410675641256026));
#47172=CARTESIAN_POINT('Origin',(-14.75,0.,0.));
#47173=CARTESIAN_POINT('',(-14.0911584740964,-4.93264269199776,-0.00145718338004752));
#47174=CARTESIAN_POINT('',(-14.3088415259036,-4.93298263358733,-0.000852151517113329));
#47175=CARTESIAN_POINT('',(-14.75,-4.925,-6.03138548580071E-16));
#47176=CARTESIAN_POINT('Ctrl Pts',(-14.0911584740964,-4.93264269199776,
-0.00145718338004752));
#47177=CARTESIAN_POINT('Ctrl Pts',(-14.1668589517821,-4.92658863837471,
1.55348689693233));
#47178=CARTESIAN_POINT('Ctrl Pts',(-14.2425594294679,-4.13001266093176,
3.11377115163446));
#47179=CARTESIAN_POINT('Ctrl Pts',(-14.3182599071536,-2.86439733377493,
4.01638102506703));
#47180=CARTESIAN_POINT('Ctrl Pts',(-14.3978057955267,-1.5344916500192,4.96484141041069));
#47181=CARTESIAN_POINT('Ctrl Pts',(-14.4773516838997,0.313315942832746,
5.18711364580286));
#47182=CARTESIAN_POINT('Ctrl Pts',(-14.5568975722728,1.83020958498003,4.58109391950248));
#47183=CARTESIAN_POINT('Ctrl Pts',(-14.6364434606459,3.3471032271273,3.97507419320211));
#47184=CARTESIAN_POINT('Ctrl Pts',(-14.715989349019,4.53308291856992,2.5407625052092));
#47185=CARTESIAN_POINT('Ctrl Pts',(-14.7955352373921,4.84335255857077,0.937029678100604));
#47186=CARTESIAN_POINT('Ctrl Pts',(-14.8750811257651,5.15362219857162,-0.666703149008015));
#47187=CARTESIAN_POINT('Ctrl Pts',(-14.9546270141382,4.58818178713068,-2.43985711523233));
#47188=CARTESIAN_POINT('Ctrl Pts',(-15.0341729025113,3.40677416265819,-3.56790953205094));
#47189=CARTESIAN_POINT('Ctrl Pts',(-15.1137187908843,2.22536653818572,-4.69596194886955));
#47190=CARTESIAN_POINT('Ctrl Pts',(-15.1932646792574,0.427991700681723,
-5.17891281628248));
#47191=CARTESIAN_POINT('Ctrl Pts',(-15.2728105676305,-1.15970147061867,
-4.79491200370771));
#47192=CARTESIAN_POINT('Ctrl Pts',(-15.3523564560036,-2.74739464191907,
-4.41091119113294));
#47193=CARTESIAN_POINT('Ctrl Pts',(-15.4319023443767,-4.12540614701586,
-3.15995869857046));
#47194=CARTESIAN_POINT('Ctrl Pts',(-15.5114482327497,-4.6607274275294,-1.61669677754691));
#47195=CARTESIAN_POINT('Ctrl Pts',(-15.5380183131986,-4.83953653734212,
-1.10121327193814));
#47196=CARTESIAN_POINT('Ctrl Pts',(-15.5645883936475,-4.92432608553159,
-0.553116590668242));
#47197=CARTESIAN_POINT('Ctrl Pts',(-15.5911584740964,-4.92035796642718,
-0.00383015064837622));
#47198=CARTESIAN_POINT('Ctrl Pts',(-15.8088415259036,-4.92120003017842,
-0.00410675641256026));
#47199=CARTESIAN_POINT('Ctrl Pts',(-15.7838994916307,-4.92524055907015,
-0.519513955654037));
#47200=CARTESIAN_POINT('Ctrl Pts',(-15.7589574573578,-4.85074335816441,
-1.03378245448552));
#47201=CARTESIAN_POINT('Ctrl Pts',(-15.7340154230849,-4.69282487345136,
-1.52101290006915));
#47202=CARTESIAN_POINT('Ctrl Pts',(-15.6544695347118,-4.18918647653558,
-3.07490294016289));
#47203=CARTESIAN_POINT('Ctrl Pts',(-15.5749236463387,-2.83705442535027,
-4.35378382722562));
#47204=CARTESIAN_POINT('Ctrl Pts',(-15.4953777579656,-1.25754919479281,
-4.77018401717759));
#47205=CARTESIAN_POINT('Ctrl Pts',(-15.4158318695926,0.321956035764672,
-5.18658420712955));
#47206=CARTESIAN_POINT('Ctrl Pts',(-15.3362859812195,2.12883444569431,-4.74050369997076));
#47207=CARTESIAN_POINT('Ctrl Pts',(-15.2567400928464,3.33307155891485,-3.63685571864124));
#47208=CARTESIAN_POINT('Ctrl Pts',(-15.1771942044733,4.5373086721354,-2.53320773731172));
#47209=CARTESIAN_POINT('Ctrl Pts',(-15.0976483161003,5.13890448864684,-0.771992281811449));
#47210=CARTESIAN_POINT('Ctrl Pts',(-15.0181024277272,4.86150768690456,0.837752078617765));
#47211=CARTESIAN_POINT('Ctrl Pts',(-14.9385565393541,4.58411088516229,2.44749643904697));
#47212=CARTESIAN_POINT('Ctrl Pts',(-14.859010650981,3.42772146516635,3.90576970440512));
#47213=CARTESIAN_POINT('Ctrl Pts',(-14.779464762608,1.92354282904339,4.5426939716314));
#47214=CARTESIAN_POINT('Ctrl Pts',(-14.6999188742349,0.419364192920443,
5.17961823885768));
#47215=CARTESIAN_POINT('Ctrl Pts',(-14.6203729858618,-1.43260365932953,
4.99519350795208));
#47216=CARTESIAN_POINT('Ctrl Pts',(-14.5408270974887,-2.78163379546954,
4.07413781835645));
#47217=CARTESIAN_POINT('Ctrl Pts',(-14.463498573627,-4.09305932865878,3.17875682095258));
#47218=CARTESIAN_POINT('Ctrl Pts',(-14.3861700497653,-4.92919541411866,
1.58724007886021));
#47219=CARTESIAN_POINT('Ctrl Pts',(-14.3088415259036,-4.93298263358733,
-0.000852151517113329));
#47220=CARTESIAN_POINT('Origin',(-14.75,0.,0.));
#47221=CARTESIAN_POINT('',(-12.5911584740964,-4.92478776395509,0.00455105250847659));
#47222=CARTESIAN_POINT('',(-12.8088415259036,-4.92377532403654,0.00452825219503028));
#47223=CARTESIAN_POINT('',(-14.75,-4.925,-6.03138548580071E-16));
#47224=CARTESIAN_POINT('Ctrl Pts',(-12.5911584740964,-4.92478776395509,
0.00455105250847659));
#47225=CARTESIAN_POINT('Ctrl Pts',(-12.6100377331706,-4.92837678960448,
0.393954978247036));
#47226=CARTESIAN_POINT('Ctrl Pts',(-12.6289169922448,-4.88609691325311,
0.78258860004133));
#47227=CARTESIAN_POINT('Ctrl Pts',(-12.647796251319,-4.79498154009321,1.15941392712904));
#47228=CARTESIAN_POINT('Ctrl Pts',(-12.7273421396921,-4.41107593903318,
2.74713012334508));
#47229=CARTESIAN_POINT('Ctrl Pts',(-12.8068880280651,-3.16020608534884,
4.12521664311483));
#47230=CARTESIAN_POINT('Ctrl Pts',(-12.8864339164382,-1.61697626926029,
4.66063046903576));
#47231=CARTESIAN_POINT('Ctrl Pts',(-12.9659798048113,-0.0737464531717311,
5.19604429495669));
#47232=CARTESIAN_POINT('Ctrl Pts',(-13.0455256931844,1.76184332532101,4.8887854270288));
#47233=CARTESIAN_POINT('Ctrl Pts',(-13.1250715815575,3.04658962766721,3.87999745680921));
#47234=CARTESIAN_POINT('Ctrl Pts',(-13.2046174699305,4.33133593001341,2.87120948658962));
#47235=CARTESIAN_POINT('Ctrl Pts',(-13.2841633583036,5.06523875621307,1.16089241407827));
#47236=CARTESIAN_POINT('Ctrl Pts',(-13.3637092466767,4.91116973811745,-0.465296064516709));
#47237=CARTESIAN_POINT('Ctrl Pts',(-13.4432551350498,4.75710072002183,-2.09148454311171));
#47238=CARTESIAN_POINT('Ctrl Pts',(-13.5228010234228,3.71505985763101,-3.63354442779033));
#47239=CARTESIAN_POINT('Ctrl Pts',(-13.6023469117959,2.26372296869752,-4.38310927826887));
#47240=CARTESIAN_POINT('Ctrl Pts',(-13.681892800169,0.812386079764056,-5.13267412874741));
#47241=CARTESIAN_POINT('Ctrl Pts',(-13.7614386885421,-1.0482468357121,-5.08974394502581));
#47242=CARTESIAN_POINT('Ctrl Pts',(-13.8409845769151,-2.46346842939373,
-4.27403929809212));
#47243=CARTESIAN_POINT('Ctrl Pts',(-13.9205304652882,-3.87869002307536,
-3.45833465115842));
#47244=CARTESIAN_POINT('Ctrl Pts',(-14.0000763536613,-4.84850029496252,
-1.86985554101265));
#47245=CARTESIAN_POINT('Ctrl Pts',(-14.0796222420344,-4.92740354357634,
-0.238291718292194));
#47246=CARTESIAN_POINT('Ctrl Pts',(-14.0834676527217,-4.93121788774538,
-0.159418591229293));
#47247=CARTESIAN_POINT('Ctrl Pts',(-14.0873130634091,-4.93295022404004,
-0.0804447772164642));
#47248=CARTESIAN_POINT('Ctrl Pts',(-14.0911584740964,-4.93264269199776,
-0.00145718338004752));
#47249=CARTESIAN_POINT('Ctrl Pts',(-14.3088415259036,-4.93298263358733,
-0.000852151517113329));
#47250=CARTESIAN_POINT('Ctrl Pts',(-14.3066241613922,-4.93309123059174,
-0.0463900614183807));
#47251=CARTESIAN_POINT('Ctrl Pts',(-14.3044067968809,-4.93251544314009,
-0.0919251555741316));
#47252=CARTESIAN_POINT('Ctrl Pts',(-14.3021894323695,-4.93124685277319,
-0.137440940316469));
#47253=CARTESIAN_POINT('Ctrl Pts',(-14.2226435439964,-4.88573735390672,
-1.77027736110802));
#47254=CARTESIAN_POINT('Ctrl Pts',(-14.1430976556234,-3.94862593614372,
-3.37826355440545));
#47255=CARTESIAN_POINT('Ctrl Pts',(-14.0635517672503,-2.55038763209838,
-4.22274892233722));
#47256=CARTESIAN_POINT('Ctrl Pts',(-13.9840058788772,-1.15214932805305,
-5.06723429026899));
#47257=CARTESIAN_POINT('Ctrl Pts',(-13.9044599905041,0.707215862274635,
-5.14821883283511));
#47258=CARTESIAN_POINT('Ctrl Pts',(-13.8249141021311,2.17358293754952,-4.42850118535088));
#47259=CARTESIAN_POINT('Ctrl Pts',(-13.745368213758,3.6399500128244,-3.70878353786665));
#47260=CARTESIAN_POINT('Ctrl Pts',(-13.6658223253849,4.71331897304647,-2.18836370033207));
#47261=CARTESIAN_POINT('Ctrl Pts',(-13.5862764370118,4.90062300737523,-0.565667459418628));
#47262=CARTESIAN_POINT('Ctrl Pts',(-13.5067305486388,5.08792704170398,1.05702878149484));
#47263=CARTESIAN_POINT('Ctrl Pts',(-13.4271846602657,4.38916615013937,2.78200142578717));
#47264=CARTESIAN_POINT('Ctrl Pts',(-13.3476387718926,3.12532576929452,3.81686053856362));
#47265=CARTESIAN_POINT('Ctrl Pts',(-13.2680928835195,1.86148538844969,4.85171965134006));
#47266=CARTESIAN_POINT('Ctrl Pts',(-13.1885469951465,0.0325655183246379,
5.19646523260064));
#47267=CARTESIAN_POINT('Ctrl Pts',(-13.1090011067734,-1.52129431677496,
4.69273365287321));
#47268=CARTESIAN_POINT('Ctrl Pts',(-13.0294552184003,-3.07515415187458,
4.18900207314577));
#47269=CARTESIAN_POINT('Ctrl Pts',(-12.9499093300272,-4.35395395194874,
2.8367933324303));
#47270=CARTESIAN_POINT('Ctrl Pts',(-12.8703634416541,-4.77025942134235,
1.25726313401576));
#47271=CARTESIAN_POINT('Ctrl Pts',(-12.849856136404,-4.87758493511541,0.850052798028952));
#47272=CARTESIAN_POINT('Ctrl Pts',(-12.8293488311538,-4.92758625344338,
0.427733934129015));
#47273=CARTESIAN_POINT('Ctrl Pts',(-12.8088415259036,-4.92377532403654,
0.00452825219503028));
#47274=CARTESIAN_POINT('Origin',(-14.75,0.,0.));
#47275=CARTESIAN_POINT('',(-11.0911584740964,-4.91693014897725,-0.000625914149278983));
#47276=CARTESIAN_POINT('',(-11.3088415259036,-4.91711289028958,-0.00117313378838655));
#47277=CARTESIAN_POINT('',(-14.75,-4.925,-6.03138548580071E-16));
#47278=CARTESIAN_POINT('Ctrl Pts',(-11.0911584740964,-4.91693014897725,
-0.000625914149278983));
#47279=CARTESIAN_POINT('Ctrl Pts',(-11.1327624029322,-4.91595655984975,
0.8609597041095));
#47280=CARTESIAN_POINT('Ctrl Pts',(-11.1743663317679,-4.70077081773724,
1.72300021548812));
#47281=CARTESIAN_POINT('Ctrl Pts',(-11.2159702606036,-4.27418701974417,
2.46321211926741));
#47282=CARTESIAN_POINT('Ctrl Pts',(-11.2955161489767,-3.45856724232153,
3.87848262660126));
#47283=CARTESIAN_POINT('Ctrl Pts',(-11.3750620373498,-1.87014629263889,
4.84838815470011));
#47284=CARTESIAN_POINT('Ctrl Pts',(-11.4546079257229,-0.238587204524135,
4.92738924483267));
#47285=CARTESIAN_POINT('Ctrl Pts',(-11.5341538140959,1.39297188359064,5.00639033496524));
#47286=CARTESIAN_POINT('Ctrl Pts',(-11.613699702469,3.06766911013748,4.19448698713153));
#47287=CARTESIAN_POINT('Ctrl Pts',(-11.6932455908421,4.01620924559344,2.86463818306347));
#47288=CARTESIAN_POINT('Ctrl Pts',(-11.7727914792152,4.96474938104939,1.53478937899541));
#47289=CARTESIAN_POINT('Ctrl Pts',(-11.8523373675882,5.18713242541439,-0.313004881306989));
#47290=CARTESIAN_POINT('Ctrl Pts',(-11.9318832559613,4.58120366532001,-1.82993486253306));
#47291=CARTESIAN_POINT('Ctrl Pts',(-12.0114291443344,3.97527490522564,-3.34686484375911));
#47292=CARTESIAN_POINT('Ctrl Pts',(-12.0909750327075,2.54103434067188,-4.53293054590886));
#47293=CARTESIAN_POINT('Ctrl Pts',(-12.1705209210806,0.937320122704561,
-4.84329635804258));
#47294=CARTESIAN_POINT('Ctrl Pts',(-12.2500668094536,-0.666394095262762,
-5.1536621701763));
#47295=CARTESIAN_POINT('Ctrl Pts',(-12.3296126978267,-2.43958196664368,
-4.588328092294));
#47296=CARTESIAN_POINT('Ctrl Pts',(-12.4091585861998,-3.56770522811629,
-3.4069881170217));
#47297=CARTESIAN_POINT('Ctrl Pts',(-12.4698252154987,-4.42808201322696,
-2.50602496453717));
#47298=CARTESIAN_POINT('Ctrl Pts',(-12.5304918447975,-4.91325478547539,
-1.24675989764379));
#47299=CARTESIAN_POINT('Ctrl Pts',(-12.5911584740964,-4.92478776395509,
0.00455105250847659));
#47300=CARTESIAN_POINT('Ctrl Pts',(-12.8088415259036,-4.92377532403654,
0.00452825219503028));
#47301=CARTESIAN_POINT('Ctrl Pts',(-12.7498029427807,-4.91280402040514,
-1.21384069126802));
#47302=CARTESIAN_POINT('Ctrl Pts',(-12.6907643596578,-4.45583175677877,
-2.43955966583319));
#47303=CARTESIAN_POINT('Ctrl Pts',(-12.6317257765349,-3.63665583438227,
-3.33328964797749));
#47304=CARTESIAN_POINT('Ctrl Pts',(-12.5521798881619,-2.53293563931553,
-4.53746057544264));
#47305=CARTESIAN_POINT('Ctrl Pts',(-12.4726339997888,-0.771684110468958,
-5.13895077425935));
#47306=CARTESIAN_POINT('Ctrl Pts',(-12.3930881114157,0.838043612127357,
-4.86145743982533));
#47307=CARTESIAN_POINT('Ctrl Pts',(-12.3135422230426,2.44777133472372,-4.58396410539131));
#47308=CARTESIAN_POINT('Ctrl Pts',(-12.2339963346695,3.90597525106984,-3.42748723770652));
#47309=CARTESIAN_POINT('Ctrl Pts',(-12.1544504462965,4.54280931452835,-1.92327040919758));
#47310=CARTESIAN_POINT('Ctrl Pts',(-12.0749045579234,5.17964337798684,-0.419053580688679));
#47311=CARTESIAN_POINT('Ctrl Pts',(-11.9953586695503,4.99510758855781,1.43290320864429));
#47312=CARTESIAN_POINT('Ctrl Pts',(-11.9158127811772,4.07397100194497,2.78187810846774));
#47313=CARTESIAN_POINT('Ctrl Pts',(-11.8362668928042,3.15283441533213,4.13085300829118));
#47314=CARTESIAN_POINT('Ctrl Pts',(-11.7567210044311,1.49509703153545,4.97684601860504));
#47315=CARTESIAN_POINT('Ctrl Pts',(-11.677175116058,-0.137736657205341,
4.93123860184462));
#47316=CARTESIAN_POINT('Ctrl Pts',(-11.5976292276849,-1.77057034594614,
4.88563118508419));
#47317=CARTESIAN_POINT('Ctrl Pts',(-11.5180833393119,-3.37850033963107,
3.94842334124948));
#47318=CARTESIAN_POINT('Ctrl Pts',(-11.4385374509388,-4.22290185645441,
2.55013439759839));
#47319=CARTESIAN_POINT('Ctrl Pts',(-11.3953054759271,-4.68182117990154,
1.79018572008053));
#47320=CARTESIAN_POINT('Ctrl Pts',(-11.3520735009153,-4.91521278868756,
0.894044916314203));
#47321=CARTESIAN_POINT('Ctrl Pts',(-11.3088415259036,-4.91711289028958,
-0.00117313378838655));
#47322=CARTESIAN_POINT('Origin',(-14.75,0.,0.));
#47323=CARTESIAN_POINT('',(-9.59115847409641,-4.92709248349153,-0.00433039759252629));
#47324=CARTESIAN_POINT('',(-9.80884152590359,-4.92809314710804,-0.00411155299795817));
#47325=CARTESIAN_POINT('',(-14.75,-4.925,-6.03138548580071E-16));
#47326=CARTESIAN_POINT('Ctrl Pts',(-9.59115847409641,-4.92709248349153,
-0.00433039759252629));
#47327=CARTESIAN_POINT('Ctrl Pts',(-9.6554870726937,-4.91489864183716,1.32092114795559));
#47328=CARTESIAN_POINT('Ctrl Pts',(-9.71981567129099,-4.36249459000914,
2.65513262914084));
#47329=CARTESIAN_POINT('Ctrl Pts',(-9.78414426988828,-3.40720205913308,
3.56750091135165));
#47330=CARTESIAN_POINT('Ctrl Pts',(-9.86369015826136,-2.2259297373092,4.69569501342137));
#47331=CARTESIAN_POINT('Ctrl Pts',(-9.94323604663443,-0.428612835952052,
5.17886144739986));
#47332=CARTESIAN_POINT('Ctrl Pts',(-10.0227819350075,1.15912637946997,4.79505105923515));
#47333=CARTESIAN_POINT('Ctrl Pts',(-10.1023278233806,2.74686559489197,4.41124067107045));
#47334=CARTESIAN_POINT('Ctrl Pts',(-10.1818737117537,4.12502712437884,3.16045346076258));
#47335=CARTESIAN_POINT('Ctrl Pts',(-10.2614196001267,4.66053349378172,1.61725575515876));
#47336=CARTESIAN_POINT('Ctrl Pts',(-10.3409654884998,5.19603986318461,0.0740580495549087));
#47337=CARTESIAN_POINT('Ctrl Pts',(-10.4205113768729,4.88889107250348,-1.76155015134491));
#47338=CARTESIAN_POINT('Ctrl Pts',(-10.500057265246,3.88018014779652,-3.04635694640356));
#47339=CARTESIAN_POINT('Ctrl Pts',(-10.579603153619,2.87146922308957,-4.3311637414622));
#47340=CARTESIAN_POINT('Ctrl Pts',(-10.6591490419921,1.16119616435681,-5.06516913067968));
#47341=CARTESIAN_POINT('Ctrl Pts',(-10.7386949303652,-0.465001550528919,
-4.91119763217294));
#47342=CARTESIAN_POINT('Ctrl Pts',(-10.8182408187383,-2.09119926541465,
-4.75722613366619));
#47343=CARTESIAN_POINT('Ctrl Pts',(-10.8977867071114,-3.63332163645336,
-3.71527774743521));
#47344=CARTESIAN_POINT('Ctrl Pts',(-10.9773325954844,-4.3829735193914,-2.26398581103529));
#47345=CARTESIAN_POINT('Ctrl Pts',(-11.0152745550218,-4.74054399840997,
-1.5717456330203));
#47346=CARTESIAN_POINT('Ctrl Pts',(-11.0532165145591,-4.91781804298907,
-0.786374942684098));
#47347=CARTESIAN_POINT('Ctrl Pts',(-11.0911584740964,-4.91693014897725,
-0.000625914149278983));
#47348=CARTESIAN_POINT('Ctrl Pts',(-11.3088415259036,-4.91711289028958,
-0.00117313378838655));
#47349=CARTESIAN_POINT('Ctrl Pts',(-11.2725276125423,-4.91870893407279,
-0.753136714034694));
#47350=CARTESIAN_POINT('Ctrl Pts',(-11.2362136991809,-4.7569730771308,-1.5044492332048));
#47351=CARTESIAN_POINT('Ctrl Pts',(-11.1998997858196,-4.42837083191147,
-2.1738485021124));
#47352=CARTESIAN_POINT('Ctrl Pts',(-11.1203538974465,-3.70856525058346,
-3.64017241470453));
#47353=CARTESIAN_POINT('Ctrl Pts',(-11.0408080090734,-2.18808104796575,
-4.71345019642131));
#47354=CARTESIAN_POINT('Ctrl Pts',(-10.9612621207003,-0.565373577716975,
-4.90065692052403));
#47355=CARTESIAN_POINT('Ctrl Pts',(-10.8817162323273,1.05733389253182,-5.08786364462675));
#47356=CARTESIAN_POINT('Ctrl Pts',(-10.8021703439542,2.78226463041168,-4.38899931111538));
#47357=CARTESIAN_POINT('Ctrl Pts',(-10.7226244555811,3.81704795131542,-3.12509687408555));
#47358=CARTESIAN_POINT('Ctrl Pts',(-10.643078567208,4.85183127221915,-1.86119443705574));
#47359=CARTESIAN_POINT('Ctrl Pts',(-10.563532678835,5.1964671761468,-0.0322538965074959));
#47360=CARTESIAN_POINT('Ctrl Pts',(-10.4839867904619,4.6926424154192,1.52157572801001));
#47361=CARTESIAN_POINT('Ctrl Pts',(-10.4044409020888,4.1888176546916,3.07540535252754));
#47362=CARTESIAN_POINT('Ctrl Pts',(-10.3248950137157,2.83653222930873,4.35412406101433));
#47363=CARTESIAN_POINT('Ctrl Pts',(-10.2453491253427,1.25697706871738,4.77033480835247));
#47364=CARTESIAN_POINT('Ctrl Pts',(-10.1658032369696,-0.322578091873937,
5.1865455556906));
#47365=CARTESIAN_POINT('Ctrl Pts',(-10.0862573485965,-2.12940298767373,
4.74024834188012));
#47366=CARTESIAN_POINT('Ctrl Pts',(-10.0067114602234,-3.33350772505308,
3.6364559370453));
#47367=CARTESIAN_POINT('Ctrl Pts',(-9.94075481545016,-4.33190890024233,
2.72123020963015));
#47368=CARTESIAN_POINT('Ctrl Pts',(-9.87479817067687,-4.91593144188893,
1.35396723904141));
#47369=CARTESIAN_POINT('Ctrl Pts',(-9.80884152590359,-4.92809314710804,
-0.00411155299795817));
#47370=CARTESIAN_POINT('Origin',(-14.75,0.,0.));
#47371=CARTESIAN_POINT('',(-8.09115847409641,-4.93134763236354,0.00268789096151988));
#47372=CARTESIAN_POINT('',(-8.3088415259036,-4.93058250867777,0.00315514943839852));
#47373=CARTESIAN_POINT('',(-14.75,-4.925,-6.03138548580071E-16));
#47374=CARTESIAN_POINT('Ctrl Pts',(-8.09115847409641,-4.93134763236354,
0.00268789096151988));
#47375=CARTESIAN_POINT('Ctrl Pts',(-8.09866585408217,-4.93236070319556,
0.157002391239283));
#47376=CARTESIAN_POINT('Ctrl Pts',(-8.10617323406794,-4.92574782328456,
0.311228913952019));
#47377=CARTESIAN_POINT('Ctrl Pts',(-8.11368061405371,-4.91122550856618,
0.464707034867637));
#47378=CARTESIAN_POINT('Ctrl Pts',(-8.19322650242678,-4.7573515302013,2.09091398019483));
#47379=CARTESIAN_POINT('Ctrl Pts',(-8.27277239079985,-3.71549562387871,
3.63309883205044));
#47380=CARTESIAN_POINT('Ctrl Pts',(-8.35231827917293,-2.2642486452318,4.38283774475274));
#47381=CARTESIAN_POINT('Ctrl Pts',(-8.431864167546,-0.813001666584828,5.13257665745506));
#47382=CARTESIAN_POINT('Ctrl Pts',(-8.51141005591908,1.0476363843865,5.089869631004));
#47383=CARTESIAN_POINT('Ctrl Pts',(-8.59095594429216,2.46295580028325,4.27433472602514));
#47384=CARTESIAN_POINT('Ctrl Pts',(-8.67050183266523,3.87827521617993,3.45879982104632));
#47385=CARTESIAN_POINT('Ctrl Pts',(-8.75004772103831,4.84827599700209,1.87043703753978));
#47386=CARTESIAN_POINT('Ctrl Pts',(-8.82959360941138,4.9273749283692,0.238882689898267));
#47387=CARTESIAN_POINT('Ctrl Pts',(-8.90913949778446,5.0064738597363,-1.39267165774325));
#47388=CARTESIAN_POINT('Ctrl Pts',(-8.98868538615753,4.19467094164835,-3.06741756951973));
#47389=CARTESIAN_POINT('Ctrl Pts',(-9.0682312745306,2.86487902205042,-4.01603745167696));
#47390=CARTESIAN_POINT('Ctrl Pts',(-9.14777716290368,1.53508710245243,-4.96465733383422));
#47391=CARTESIAN_POINT('Ctrl Pts',(-9.22732305127675,-0.312693818655589,
-5.18715118637216));
#47392=CARTESIAN_POINT('Ctrl Pts',(-9.30686893964983,-1.82966013350537,
-4.58131339466273));
#47393=CARTESIAN_POINT('Ctrl Pts',(-9.38641482802291,-3.3466264483551,-3.97547560295332));
#47394=CARTESIAN_POINT('Ctrl Pts',(-9.46596071639599,-4.53277815694662,
-2.54130616699661));
#47395=CARTESIAN_POINT('Ctrl Pts',(-9.54550660476906,-4.84324014009708,
-0.937610563937788));
#47396=CARTESIAN_POINT('Ctrl Pts',(-9.56072389454484,-4.9026321471334,-0.630820342557176));
#47397=CARTESIAN_POINT('Ctrl Pts',(-9.57594118432063,-4.9299770049327,-0.317826062571257));
#47398=CARTESIAN_POINT('Ctrl Pts',(-9.59115847409641,-4.92709248349153,
-0.00433039759252629));
#47399=CARTESIAN_POINT('Ctrl Pts',(-9.80884152590359,-4.92809314710804,
-0.00411155299795817));
#47400=CARTESIAN_POINT('Ctrl Pts',(-9.7952522823038,-4.93059885938888,-0.283920563844114));
#47401=CARTESIAN_POINT('Ctrl Pts',(-9.781663038704,-4.90882931597747,-0.563339710114124));
#47402=CARTESIAN_POINT('Ctrl Pts',(-9.7680737951042,-4.86140717526349,-0.838335142623281));
#47403=CARTESIAN_POINT('Ctrl Pts',(-9.68852790673113,-4.58381730913562,
-2.44804622159789));
#47404=CARTESIAN_POINT('Ctrl Pts',(-9.60898201835805,-3.42725299792094,
-3.90618078368793));
#47405=CARTESIAN_POINT('Ctrl Pts',(-9.52943612998497,-1.9229979824355,-4.54292464108855));
#47406=CARTESIAN_POINT('Ctrl Pts',(-9.4498902416119,-0.418742966950077,
-5.17966849848915));
#47407=CARTESIAN_POINT('Ctrl Pts',(-9.37034435323882,1.43320275280612,-4.99502165120035));
#47408=CARTESIAN_POINT('Ctrl Pts',(-9.29079846486575,2.78212241146185,-4.07380417088284));
#47409=CARTESIAN_POINT('Ctrl Pts',(-9.21125257649268,4.1310420701176,-3.15258669056531));
#47410=CARTESIAN_POINT('Ctrl Pts',(-9.13170668811961,4.97693566767287,-1.49479857721911));
#47411=CARTESIAN_POINT('Ctrl Pts',(-9.05216079974653,4.93123033318249,0.138032373598989));
#47412=CARTESIAN_POINT('Ctrl Pts',(-8.97261491137345,4.8855249986921,1.77086332441709));
#47413=CARTESIAN_POINT('Ctrl Pts',(-8.89306902300037,3.94822073215603,3.37873711270705));
#47414=CARTESIAN_POINT('Ctrl Pts',(-8.8135231346273,2.54988115392759,4.22305477538536));
#47415=CARTESIAN_POINT('Ctrl Pts',(-8.73397724625422,1.15154157569918,5.06737243806365));
#47416=CARTESIAN_POINT('Ctrl Pts',(-8.65443135788115,-0.707833314221602,
5.14813397513033));
#47417=CARTESIAN_POINT('Ctrl Pts',(-8.57488546950808,-2.17411405885781,
4.428240462547));
#47418=CARTESIAN_POINT('Ctrl Pts',(-8.495339581135,-3.64039480349401,3.70834694996368));
#47419=CARTESIAN_POINT('Ctrl Pts',(-8.41579369276192,-4.71358140284566,
2.18779838773033));
#47420=CARTESIAN_POINT('Ctrl Pts',(-8.33624780438885,-4.90069081604919,
0.565079693981939));
#47421=CARTESIAN_POINT('Ctrl Pts',(-8.3271123782271,-4.92217934629819,0.378719001918263));
#47422=CARTESIAN_POINT('Ctrl Pts',(-8.31797695206535,-4.93198112784769,
0.191010756085821));
#47423=CARTESIAN_POINT('Ctrl Pts',(-8.3088415259036,-4.93058250867777,0.00315514943839852));
#47424=CARTESIAN_POINT('Origin',(-14.75,0.,0.));
#47425=CARTESIAN_POINT('',(-6.5911584740964,-4.91874206214364,0.00300395193210873));
#47426=CARTESIAN_POINT('',(-6.8088415259036,-4.91816702752264,0.00255975366377111));
#47427=CARTESIAN_POINT('',(-14.75,-4.925,-6.03138548580071E-16));
#47428=CARTESIAN_POINT('Ctrl Pts',(-6.5911584740964,-4.91874206214364,0.00300395193210873));
#47429=CARTESIAN_POINT('Ctrl Pts',(-6.62139052384371,-4.92221047690888,
0.628510441243254));
#47430=CARTESIAN_POINT('Ctrl Pts',(-6.65162257359103,-4.81164202146414,
1.2528364358832));
#47431=CARTESIAN_POINT('Ctrl Pts',(-6.68185462333834,-4.5814231074921,1.8293853978311));
#47432=CARTESIAN_POINT('Ctrl Pts',(-6.76140051171141,-3.97567628631209,
3.34638804078933));
#47433=CARTESIAN_POINT('Ctrl Pts',(-6.84094640008449,-2.54157798418442,
4.53262575168735));
#47434=CARTESIAN_POINT('Ctrl Pts',(-6.92049228845757,-0.937901001819111,
4.8431839047693));
#47435=CARTESIAN_POINT('Ctrl Pts',(-7.00003817683064,0.665775980546221,
5.15374205785124));
#47436=CARTESIAN_POINT('Ctrl Pts',(-7.07958406520371,2.43903164314918,4.58862065311707));
#47437=CARTESIAN_POINT('Ctrl Pts',(-7.15912995357679,3.5672965817681,3.40741598897341));
#47438=CARTESIAN_POINT('Ctrl Pts',(-7.23867584194987,4.69556152038701,2.22621132482977));
#47439=CARTESIAN_POINT('Ctrl Pts',(-7.31822173032295,5.17883573502188,0.428923401276672));
#47440=CARTESIAN_POINT('Ctrl Pts',(-7.39776761869602,4.79512056112791,-1.15883882763304));
#47441=CARTESIAN_POINT('Ctrl Pts',(-7.4773135070691,4.41140538723394,-2.74660105654276));
#47442=CARTESIAN_POINT('Ctrl Pts',(-7.55685939544217,3.16070082481106,-4.12483759080913));
#47443=CARTESIAN_POINT('Ctrl Pts',(-7.63640528381525,1.61753523524406,-4.66043650177258));
#47444=CARTESIAN_POINT('Ctrl Pts',(-7.71595117218832,0.0743696456770546,
-5.19603541273603));
#47445=CARTESIAN_POINT('Ctrl Pts',(-7.7954970605614,-1.76125697103409,-4.88899670039663));
#47446=CARTESIAN_POINT('Ctrl Pts',(-7.87504294893448,-3.04612425418612,
-3.88036282482753));
#47447=CARTESIAN_POINT('Ctrl Pts',(-7.94708145732179,-4.20972836304737,
-2.96692177349214));
#47448=CARTESIAN_POINT('Ctrl Pts',(-8.0191199657091,-4.92162651637264,-1.47806657246253));
#47449=CARTESIAN_POINT('Ctrl Pts',(-8.09115847409641,-4.93134763236354,
0.00268789096151988));
#47450=CARTESIAN_POINT('Ctrl Pts',(-8.3088415259036,-4.93058250867777,0.00315514943839852));
#47451=CARTESIAN_POINT('Ctrl Pts',(-8.23843106369227,-4.91980277925207,
-1.44472476977317));
#47452=CARTESIAN_POINT('Ctrl Pts',(-8.16802060148095,-4.24367279446414,
-2.90135853255996));
#47453=CARTESIAN_POINT('Ctrl Pts',(-8.09761013926962,-3.12486796763837,
-3.8172353503401));
#47454=CARTESIAN_POINT('Ctrl Pts',(-8.01806425089654,-1.86090347896865,
-4.85194287565023));
#47455=CARTESIAN_POINT('Ctrl Pts',(-7.93851836252347,-0.0319422745738374,
-5.19646910100704));
#47456=CARTESIAN_POINT('Ctrl Pts',(-7.85897247415039,1.52185713377351,-4.69255116109043));
#47457=CARTESIAN_POINT('Ctrl Pts',(-7.77942658577732,3.07565654212083,-4.18863322117384));
#47458=CARTESIAN_POINT('Ctrl Pts',(-7.69988069740424,4.35429415442072,-2.83627111598379));
#47459=CARTESIAN_POINT('Ctrl Pts',(-7.62033480903117,4.77041017820713,-1.25669099889733));
#47460=CARTESIAN_POINT('Ctrl Pts',(-7.54078892065809,5.18652620199355,0.322889118189166));
#47461=CARTESIAN_POINT('Ctrl Pts',(-7.46124303228501,4.7401206372665,2.12968724717213));
#47462=CARTESIAN_POINT('Ctrl Pts',(-7.38169714391194,3.63625602663207,3.33372579013805));
#47463=CARTESIAN_POINT('Ctrl Pts',(-7.30215125553886,2.53239141599764,4.53776433310397));
#47464=CARTESIAN_POINT('Ctrl Pts',(-7.22260536716579,0.771067759455849,
5.13904329005283));
#47465=CARTESIAN_POINT('Ctrl Pts',(-7.14305947879271,-0.838626670106471,
4.86135689322456));
#47466=CARTESIAN_POINT('Ctrl Pts',(-7.06351359041964,-2.44832109966874,
4.58367049639629));
#47467=CARTESIAN_POINT('Ctrl Pts',(-6.98396770204656,-3.90638630225154,
3.42701874579095));
#47468=CARTESIAN_POINT('Ctrl Pts',(-6.90442181367349,-4.54303995130782,
1.92272554874775));
#47469=CARTESIAN_POINT('Ctrl Pts',(-6.87256171775019,-4.79803548588176,
1.32021891346095));
#47470=CARTESIAN_POINT('Ctrl Pts',(-6.8407016218269,-4.92126012648956,0.661943615096396));
#47471=CARTESIAN_POINT('Ctrl Pts',(-6.8088415259036,-4.91816702752264,0.00255975366377111));
#47472=CARTESIAN_POINT('Origin',(-14.75,0.,0.));
#47473=CARTESIAN_POINT('',(-5.0911584740964,-4.92034850444268,-0.00382654489779644));
#47474=CARTESIAN_POINT('',(-5.30884152590359,-4.92118977299025,-0.00410386901592228));
#47475=CARTESIAN_POINT('',(-14.75,-4.925,-6.03138548580071E-16));
#47476=CARTESIAN_POINT('Ctrl Pts',(-5.0911584740964,-4.92034850444268,-0.00382654489779644));
#47477=CARTESIAN_POINT('Ctrl Pts',(-5.14411519360526,-4.91244809502025,
1.09095932864311));
#47478=CARTESIAN_POINT('Ctrl Pts',(-5.19707191311412,-4.55198007497204,
2.19046632634003));
#47479=CARTESIAN_POINT('Ctrl Pts',(-5.25002863262299,-3.88054548599257,
3.0458915476704));
#47480=CARTESIAN_POINT('Ctrl Pts',(-5.32957452099606,-2.87198866147391,
4.3308193112958));
#47481=CARTESIAN_POINT('Ctrl Pts',(-5.40912040936913,-1.16180365248812,
5.06502982514693));
#47482=CARTESIAN_POINT('Ctrl Pts',(-5.4886662977422,0.464412516539281,4.91125336903979));
#47483=CARTESIAN_POINT('Ctrl Pts',(-5.56821218611528,2.09062868556668,4.75747691293265));
#47484=CARTESIAN_POINT('Ctrl Pts',(-5.64775807448836,3.63287601463573,3.71571348686722));
#47485=CARTESIAN_POINT('Ctrl Pts',(-5.72730396286143,4.38270195487139,2.26451147037829));
#47486=CARTESIAN_POINT('Ctrl Pts',(-5.80684985123451,5.13252789510707,0.813309453889311));
#47487=CARTESIAN_POINT('Ctrl Pts',(-5.88639573960759,5.08993244650934,-1.04733115302316));
#47488=CARTESIAN_POINT('Ctrl Pts',(-5.96594162798066,4.27448241666476,-2.46269947196908));
#47489=CARTESIAN_POINT('Ctrl Pts',(-6.04548751635374,3.45903238682021,-3.87806779091495));
#47490=CARTESIAN_POINT('Ctrl Pts',(-6.12503340472681,1.87072777572881,-4.84816382189425));
#47491=CARTESIAN_POINT('Ctrl Pts',(-6.20457929309989,0.239178174554097,
-4.92736059443231));
#47492=CARTESIAN_POINT('Ctrl Pts',(-6.28412518147296,-1.39237142662062,
-5.00655736697037));
#47493=CARTESIAN_POINT('Ctrl Pts',(-6.36367106984604,-3.06716601787869,
-4.19485488106719));
#47494=CARTESIAN_POINT('Ctrl Pts',(-6.44321695821912,-4.01586564339155,
-2.86511985060641));
#47495=CARTESIAN_POINT('Ctrl Pts',(-6.49253079684488,-4.604004404473,-2.04076123134479));
#47496=CARTESIAN_POINT('Ctrl Pts',(-6.54184463547064,-4.91308446209832,
-1.01730814503372));
#47497=CARTESIAN_POINT('Ctrl Pts',(-6.5911584740964,-4.91874206214364,0.00300395193210873));
#47498=CARTESIAN_POINT('Ctrl Pts',(-6.8088415259036,-4.91816702752264,0.00255975366377111));
#47499=CARTESIAN_POINT('Ctrl Pts',(-6.76115573345382,-4.91353750990542,
-0.984356357220146));
#47500=CARTESIAN_POINT('Ctrl Pts',(-6.71346994100404,-4.62593290938502,
-1.97375585426302));
#47501=CARTESIAN_POINT('Ctrl Pts',(-6.66578414855426,-4.07363732517796,
-2.78236670443132));
#47502=CARTESIAN_POINT('Ctrl Pts',(-6.58623826018119,-3.15233895446205,
-4.13123111708606));
#47503=CARTESIAN_POINT('Ctrl Pts',(-6.5066923718081,-1.49450011750048,-4.97702529891446));
#47504=CARTESIAN_POINT('Ctrl Pts',(-6.42714648343503,0.138328089510376,
-4.93122204682461));
#47505=CARTESIAN_POINT('Ctrl Pts',(-6.34760059506195,1.77115629652118,-4.88541879473476));
#47506=CARTESIAN_POINT('Ctrl Pts',(-6.26805470668888,3.37897387358129,-3.94801810872673));
#47507=CARTESIAN_POINT('Ctrl Pts',(-6.18850881831581,4.22320767910246,-2.54962790101466));
#47508=CARTESIAN_POINT('Ctrl Pts',(-6.10896292994273,5.06744148462366,-1.15123769330255));
#47509=CARTESIAN_POINT('Ctrl Pts',(-6.02941704156966,5.14809151860588,0.708142036113649));
#47510=CARTESIAN_POINT('Ctrl Pts',(-5.94987115319658,4.42811007730965,2.17437960764566));
#47511=CARTESIAN_POINT('Ctrl Pts',(-5.8703252648235,3.70812863601341,3.64061717917766));
#47512=CARTESIAN_POINT('Ctrl Pts',(-5.79077937645043,2.18751571943878,4.71371259282546));
#47513=CARTESIAN_POINT('Ctrl Pts',(-5.71123348807735,0.564785808115402,
4.9007246942176));
#47514=CARTESIAN_POINT('Ctrl Pts',(-5.63168759970428,-1.05794410320798,
5.08773679560975));
#47515=CARTESIAN_POINT('Ctrl Pts',(-5.5521417113312,-2.78279100928007,4.38866558474619));
#47516=CARTESIAN_POINT('Ctrl Pts',(-5.47259582295812,-3.81742273544663,
3.1246390494413));
#47517=CARTESIAN_POINT('Ctrl Pts',(-5.41801105727328,-4.5273919305612,2.25725804886157));
#47518=CARTESIAN_POINT('Ctrl Pts',(-5.36342629158844,-4.9123547098068,1.12385261058705));
#47519=CARTESIAN_POINT('Ctrl Pts',(-5.30884152590359,-4.92118977299025,
-0.00410386901592228));
#47520=CARTESIAN_POINT('Origin',(-14.75,0.,0.));
#47521=CARTESIAN_POINT('',(-3.5911584740964,-4.93263795678916,-0.00146375725000258));
#47522=CARTESIAN_POINT('',(-3.80884152590359,-4.93297963225018,-0.000859328946059894));
#47523=CARTESIAN_POINT('',(-14.75,-4.925,-6.03138548580071E-16));
#47524=CARTESIAN_POINT('Ctrl Pts',(-3.5911584740964,-4.93263795678916,-0.00146375725000258));
#47525=CARTESIAN_POINT('Ctrl Pts',(-3.66683986336681,-4.9265598841513,1.55309257837791));
#47526=CARTESIAN_POINT('Ctrl Pts',(-3.74252125263721,-4.13044035554753,
3.11300803879703));
#47527=CARTESIAN_POINT('Ctrl Pts',(-3.81820264190762,-2.8653605731944,4.01569365331712));
#47528=CARTESIAN_POINT('Ctrl Pts',(-3.8977485302807,-1.53568235084381,4.96447286866741));
#47529=CARTESIAN_POINT('Ctrl Pts',(-3.97729441865377,0.31207168483266,5.18718866129924));
#47530=CARTESIAN_POINT('Ctrl Pts',(-4.05684030702685,1.82911060574424,4.58153289102084));
#47531=CARTESIAN_POINT('Ctrl Pts',(-4.13638619539992,3.34614952665579,3.97587712074245));
#47532=CARTESIAN_POINT('Ctrl Pts',(-4.215932083773,4.53247333280247,2.54184978755386));
#47533=CARTESIAN_POINT('Ctrl Pts',(-4.29547797214607,4.84312767798418,0.938191390916231));
#47534=CARTESIAN_POINT('Ctrl Pts',(-4.37502386051915,5.15378202316589,-0.665467005721419));
#47535=CARTESIAN_POINT('Ctrl Pts',(-4.45456974889223,4.58876690738262,-2.43875646580811));
#47536=CARTESIAN_POINT('Ctrl Pts',(-4.53411563726531,3.40762989303727,-3.56709221570014));
#47537=CARTESIAN_POINT('Ctrl Pts',(-4.61366152563838,2.22649287869195,-4.69542796559215));
#47538=CARTESIAN_POINT('Ctrl Pts',(-4.69320741401145,0.429233965784571,
-5.17881000528951));
#47539=CARTESIAN_POINT('Ctrl Pts',(-4.77275330238453,-1.15855126458436,
-4.79519005809945));
#47540=CARTESIAN_POINT('Ctrl Pts',(-4.8522991907576,-2.74633649495327,-4.4115701109094));
#47541=CARTESIAN_POINT('Ctrl Pts',(-4.93184507913068,-4.12464804278375,
-3.16094817683195));
#47542=CARTESIAN_POINT('Ctrl Pts',(-5.01139096750375,-4.66033949667325,
-1.6178147030934));
#47543=CARTESIAN_POINT('Ctrl Pts',(-5.03798013636797,-4.83940080100846,
-1.10200380007321));
#47544=CARTESIAN_POINT('Ctrl Pts',(-5.06456930523218,-4.92431524033904,
-0.553510262690519));
#47545=CARTESIAN_POINT('Ctrl Pts',(-5.0911584740964,-4.92034850444268,-0.00382654489779644));
#47546=CARTESIAN_POINT('Ctrl Pts',(-5.30884152590359,-4.92118977299025,
-0.00410386901592228));
#47547=CARTESIAN_POINT('Ctrl Pts',(-5.28388040321536,-4.92522996796614,
-0.519908227999806));
#47548=CARTESIAN_POINT('Ctrl Pts',(-5.25891928052713,-4.85061618972318,
-1.03457312761624));
#47549=CARTESIAN_POINT('Ctrl Pts',(-5.2339581578389,-4.69245989025258,-1.52213853308082));
#47550=CARTESIAN_POINT('Ctrl Pts',(-5.15441226946583,-4.18844877263093,
-3.07590772055185));
#47551=CARTESIAN_POINT('Ctrl Pts',(-5.07486638109275,-2.83600999112659,
-4.35446423574767));
#47552=CARTESIAN_POINT('Ctrl Pts',(-4.99532049271967,-1.25640492385531,
-4.77048553279394));
#47553=CARTESIAN_POINT('Ctrl Pts',(-4.9157746043466,0.323200143415984,-5.18650682984021));
#47554=CARTESIAN_POINT('Ctrl Pts',(-4.83622871597352,2.1299714964542,-4.73999290873692));
#47555=CARTESIAN_POINT('Ctrl Pts',(-4.75668282760045,3.33394384188576,-3.63605609952002));
#47556=CARTESIAN_POINT('Ctrl Pts',(-4.67713693922737,4.53791618731733,-2.53211929030309));
#47557=CARTESIAN_POINT('Ctrl Pts',(-4.5975910508543,5.13908952514219,-0.770759592972526));
#47558=CARTESIAN_POINT('Ctrl Pts',(-4.51804516248122,4.86130659629173,0.83891818762146));
#47559=CARTESIAN_POINT('Ctrl Pts',(-4.43849927410815,4.58352366744127,2.44859596821542));
#47560=CARTESIAN_POINT('Ctrl Pts',(-4.35895338573507,3.42678447191547,3.90659183207286));
#47561=CARTESIAN_POINT('Ctrl Pts',(-4.27940749736199,1.92245310317772,4.54315525853296));
#47562=CARTESIAN_POINT('Ctrl Pts',(-4.19986160898891,0.418121734439937,
5.17971868499307));
#47563=CARTESIAN_POINT('Ctrl Pts',(-4.12031572061584,-1.43380180750975,
4.99484967405592));
#47564=CARTESIAN_POINT('Ctrl Pts',(-4.04076983224277,-2.78261097786045,
4.07347043921392));
#47565=CARTESIAN_POINT('Ctrl Pts',(-3.96346039679638,-4.09349803459511,
3.17799601640553));
#47566=CARTESIAN_POINT('Ctrl Pts',(-3.88615096134998,-4.92916340173032,
1.58684352759606));
#47567=CARTESIAN_POINT('Ctrl Pts',(-3.80884152590359,-4.93297963225018,
-0.000859328946059894));
#47568=CARTESIAN_POINT('Origin',(-14.75,0.,0.));
#47569=CARTESIAN_POINT('',(-2.09115847409639,-4.92479967433243,0.00455076259524401));
#47570=CARTESIAN_POINT('',(-2.3088415259036,-4.92378694620037,0.00452865572044409));
#47571=CARTESIAN_POINT('',(-14.75,-4.925,-6.03138548580071E-16));
#47572=CARTESIAN_POINT('Ctrl Pts',(-2.09115847409639,-4.92479967433243,
0.00455076259524401));
#47573=CARTESIAN_POINT('Ctrl Pts',(-2.11001864475527,-4.92838960899571,
0.393565332838783));
#47574=CARTESIAN_POINT('Ctrl Pts',(-2.12887881541415,-4.8861997157664,0.781810208141141));
#47575=CARTESIAN_POINT('Ctrl Pts',(-2.14773898607303,-4.79526872833564,
1.15827977445631));
#47576=CARTESIAN_POINT('Ctrl Pts',(-2.22728487444611,-4.41175225297358,
2.74610242143037));
#47577=CARTESIAN_POINT('Ctrl Pts',(-2.30683076281919,-3.16119502426286,
4.12445761712042));
#47578=CARTESIAN_POINT('Ctrl Pts',(-2.38637665119226,-1.61808937757221,
4.66023409988841));
#47579=CARTESIAN_POINT('Ctrl Pts',(-2.46592253956534,-0.0749837308815521,
5.19601058265641));
#47580=CARTESIAN_POINT('Ctrl Pts',(-2.54546842793841,1.76067033378902,4.88920835250233));
#47581=CARTESIAN_POINT('Ctrl Pts',(-2.62501431631149,3.04565633625721,3.88073249588954));
#47582=CARTESIAN_POINT('Ctrl Pts',(-2.70456020468456,4.33064233872542,2.87225663927674));
#47583=CARTESIAN_POINT('Ctrl Pts',(-2.78410609305764,5.06496027899121,1.16210715620522));
#47584=CARTESIAN_POINT('Ctrl Pts',(-2.86365198143071,4.91128251100273,-0.464120269161797));
#47585=CARTESIAN_POINT('Ctrl Pts',(-2.94319786980379,4.75760474301426,-2.09034769452876));
#47586=CARTESIAN_POINT('Ctrl Pts',(-3.02274375817687,3.71593126677153,-3.63265306219127));
#47587=CARTESIAN_POINT('Ctrl Pts',(-3.10228964654994,2.26477361062453,-4.38256496537029));
#47588=CARTESIAN_POINT('Ctrl Pts',(-3.18183553492302,0.813615954477467,
-5.13247686854935));
#47589=CARTESIAN_POINT('Ctrl Pts',(-3.26138142329609,-1.04702588157384,
-5.08999530724491));
#47590=CARTESIAN_POINT('Ctrl Pts',(-3.34092731166917,-2.46244278226107,
-4.27463070863102));
#47591=CARTESIAN_POINT('Ctrl Pts',(-3.42047320004224,-3.87785968294825,
-3.45926611001717));
#47592=CARTESIAN_POINT('Ctrl Pts',(-3.50001908841532,-4.84805164827134,
-1.87101847409385));
#47593=CARTESIAN_POINT('Ctrl Pts',(-3.57956497678839,-4.92734642642051,
-0.239473337097873));
#47594=CARTESIAN_POINT('Ctrl Pts',(-3.58342947589106,-4.93119872608391,
-0.160209595792822));
#47595=CARTESIAN_POINT('Ctrl Pts',(-3.58729397499373,-4.93294831983193,
-0.0808436632215555));
#47596=CARTESIAN_POINT('Ctrl Pts',(-3.5911584740964,-4.93263795678916,-0.00146375725000258));
#47597=CARTESIAN_POINT('Ctrl Pts',(-3.80884152590359,-4.93297963225018,
-0.000859328946059894));
#47598=CARTESIAN_POINT('Ctrl Pts',(-3.80660507297691,-4.93309003041654,
-0.0467893332167884));
#47599=CARTESIAN_POINT('Ctrl Pts',(-3.80436862005022,-4.93250428457465,
-0.0927164506168972));
#47600=CARTESIAN_POINT('Ctrl Pts',(-3.80213216712354,-4.93121376103269,
-0.138623755771863));
#47601=CARTESIAN_POINT('Ctrl Pts',(-3.72258627875046,-4.8853125751026,-1.77144925716878));
#47602=CARTESIAN_POINT('Ctrl Pts',(-3.64304039037739,-3.94781540449082,
-3.37921080121581));
#47603=CARTESIAN_POINT('Ctrl Pts',(-3.56349450200431,-2.54937460381079,
-4.2233606619699));
#47604=CARTESIAN_POINT('Ctrl Pts',(-3.48394861363124,-1.15093380313076,
-5.06751052272398));
#47605=CARTESIAN_POINT('Ctrl Pts',(-3.40440272525816,0.708450627617543,
-5.14804870018514));
#47606=CARTESIAN_POINT('Ctrl Pts',(-3.32485683688509,2.17464508120495,-4.42797949508699));
#47607=CARTESIAN_POINT('Ctrl Pts',(-3.24531094851201,3.64083953479237,-3.70791028998884));
#47608=CARTESIAN_POINT('Ctrl Pts',(-3.16576506013894,4.71384401121892,-2.18723370233138));
#47609=CARTESIAN_POINT('Ctrl Pts',(-3.08621917176586,4.90075868413978,-0.564492267726287));
#47610=CARTESIAN_POINT('Ctrl Pts',(-3.00667328339279,5.08767335706064,1.05824916687883));
#47611=CARTESIAN_POINT('Ctrl Pts',(-2.92712739501971,4.38849822647583,2.78305544843154));
#47612=CARTESIAN_POINT('Ctrl Pts',(-2.84758150664664,3.12440987169467,3.8176107737941));
#47613=CARTESIAN_POINT('Ctrl Pts',(-2.76803561827356,1.86032151691353,4.85216609915665));
#47614=CARTESIAN_POINT('Ctrl Pts',(-2.68848972990048,0.0313199379360557,
5.19647046832902));
#47615=CARTESIAN_POINT('Ctrl Pts',(-2.60894384152741,-1.5224194503301,4.69236732243377));
#47616=CARTESIAN_POINT('Ctrl Pts',(-2.52939795315433,-3.07615883859628,
4.18826417653852));
#47617=CARTESIAN_POINT('Ctrl Pts',(-2.44985206478126,-4.35463603615115,
2.8357535155756));
#47618=CARTESIAN_POINT('Ctrl Pts',(-2.37030617640818,-4.77056178492771,
1.25612130118806));
#47619=CARTESIAN_POINT('Ctrl Pts',(-2.34981795957332,-4.87768959633853,
0.849263725144446));
#47620=CARTESIAN_POINT('Ctrl Pts',(-2.32932974273846,-4.92759608937386,
0.427338996020449));
#47621=CARTESIAN_POINT('Ctrl Pts',(-2.3088415259036,-4.92378694620037,0.00452865572044409));
#47622=CARTESIAN_POINT('Origin',(-14.75,0.,0.));
#47623=CARTESIAN_POINT('',(-0.591158474096391,-4.91621514884034,-0.00190685489401573));
#47624=CARTESIAN_POINT('',(-0.808841525903593,-4.91703434725887,-0.0013692803956027));
#47625=CARTESIAN_POINT('',(-14.75,-4.925,-6.03138548580071E-16));
#47626=CARTESIAN_POINT('Ctrl Pts',(-0.591158474096391,-4.91617236260859,
-0.00191614214703012));
#47627=CARTESIAN_POINT('Ctrl Pts',(-0.632743314516819,-4.91557730725517,
0.859927749670198));
#47628=CARTESIAN_POINT('Ctrl Pts',(-0.674328154937247,-4.70120063118156,
1.72260089528099));
#47629=CARTESIAN_POINT('Ctrl Pts',(-0.715912995357675,-4.27522171387068,
2.46297048332456));
#47630=CARTESIAN_POINT('Ctrl Pts',(-0.795458883730751,-3.46038459863554,
3.87919226053746));
#47631=CARTESIAN_POINT('Ctrl Pts',(-0.875004772103829,-1.87128956129306,
4.84790224489492));
#47632=CARTESIAN_POINT('Ctrl Pts',(-0.954550660476906,-0.23953077630217,
4.92691531448512));
#47633=CARTESIAN_POINT('Ctrl Pts',(-1.03409654884998,1.39222800868875,5.00592838407533));
#47634=CARTESIAN_POINT('Ctrl Pts',(-1.11364243722306,3.06665054132806,4.19524453889832));
#47635=CARTESIAN_POINT('Ctrl Pts',(-1.19318832559614,4.01539704249259,2.86581937781023));
#47636=CARTESIAN_POINT('Ctrl Pts',(-1.27273421396921,4.96414354365708,1.53639421672219));
#47637=CARTESIAN_POINT('Ctrl Pts',(-1.35228010234228,5.1872140133468,-0.311772260276884));
#47638=CARTESIAN_POINT('Ctrl Pts',(-1.43182599071535,4.58170765220235,-1.82894951483846));
#47639=CARTESIAN_POINT('Ctrl Pts',(-1.51137187908843,3.9762012910579,-3.34612676940009));
#47640=CARTESIAN_POINT('Ctrl Pts',(-1.59091776746151,2.54211809907922,-4.53231480152423));
#47641=CARTESIAN_POINT('Ctrl Pts',(-1.67046365583459,0.938447910619046,
-4.84301219015054));
#47642=CARTESIAN_POINT('Ctrl Pts',(-1.75000954420766,-0.665222277841155,
-5.15370957877686));
#47643=CARTESIAN_POINT('Ctrl Pts',(-1.82955543258074,-2.43847946278283,
-4.58891632390535));
#47644=CARTESIAN_POINT('Ctrl Pts',(-1.90910132095381,-3.56687019424698,
-3.40787464734053));
#47645=CARTESIAN_POINT('Ctrl Pts',(-1.96978703866801,-4.42772174548972,
-2.50685558452536));
#47646=CARTESIAN_POINT('Ctrl Pts',(-2.0304727563822,-4.91324846594047,-1.24716794257944));
#47647=CARTESIAN_POINT('Ctrl Pts',(-2.09115847409639,-4.92479967433243,
0.00455076259524401));
#47648=CARTESIAN_POINT('Ctrl Pts',(-2.3088415259036,-4.92378694620037,0.00452865572044409));
#47649=CARTESIAN_POINT('Ctrl Pts',(-2.24978385436538,-4.912807019143,-1.21423012654258));
#47650=CARTESIAN_POINT('Ctrl Pts',(-2.19072618282717,-4.45550843625236,
-2.44034737679679));
#47651=CARTESIAN_POINT('Ctrl Pts',(-2.13166851128896,-3.63585440375436,
-3.33416659713051));
#47652=CARTESIAN_POINT('Ctrl Pts',(-2.05212262291588,-2.53184697380615,
-4.53806851324942));
#47653=CARTESIAN_POINT('Ctrl Pts',(-1.9725767345428,-0.770457813911437,
-5.13911857767506));
#47654=CARTESIAN_POINT('Ctrl Pts',(-1.89303084616973,0.839206332661352,
-4.86124723150085));
#47655=CARTESIAN_POINT('Ctrl Pts',(-1.81348495779665,2.4488704792341,-4.58337588532665));
#47656=CARTESIAN_POINT('Ctrl Pts',(-1.73393906942358,3.90680961248493,-3.42658312855265));
#47657=CARTESIAN_POINT('Ctrl Pts',(-1.65439318105051,4.54327701636474,-1.9221980209477));
#47658=CARTESIAN_POINT('Ctrl Pts',(-1.57484729267743,5.17974442024456,-0.417812913342702));
#47659=CARTESIAN_POINT('Ctrl Pts',(-1.49530140430435,4.99474009475331,1.43416454509326));
#47660=CARTESIAN_POINT('Ctrl Pts',(-1.41575551593128,4.0732911268349,2.78288857953561));
#47661=CARTESIAN_POINT('Ctrl Pts',(-1.3362096275582,3.15184215891648,4.13161261397798));
#47662=CARTESIAN_POINT('Ctrl Pts',(-1.25666373918512,1.49394854857088,4.97708322442672));
#47663=CARTESIAN_POINT('Ctrl Pts',(-1.17711785081204,-0.138895601305483,
4.93114147431309));
#47664=CARTESIAN_POINT('Ctrl Pts',(-1.09757196243897,-1.77173975118177,
4.88519972419945));
#47665=CARTESIAN_POINT('Ctrl Pts',(-1.0180260740659,-3.37953444058883,3.94784561352353));
#47666=CARTESIAN_POINT('Ctrl Pts',(-0.938480185692825,-4.22355933348682,
2.54924407639987));
#47667=CARTESIAN_POINT('Ctrl Pts',(-0.895267299096415,-4.6820714291754,
1.7894611277975));
#47668=CARTESIAN_POINT('Ctrl Pts',(-0.852054412500004,-4.91518370582573,
0.893557208022445));
#47669=CARTESIAN_POINT('Ctrl Pts',(-0.808841525903593,-4.91703434725887,
-0.0013692803956027));
#47670=CARTESIAN_POINT('Origin',(-32.3478126690739,0.,0.));
#47671=CARTESIAN_POINT('',(-0.0978126690738565,-4.06323934281354,-0.00157601073016207));
#47672=CARTESIAN_POINT('',(0.,-4.0705,-4.82875428449296E-13));
#47673=CARTESIAN_POINT('',(-32.3478126690739,-4.0705,-4.82875428449296E-13));
#47674=CARTESIAN_POINT('',(0.,-3.73359974356529,-1.6214817929441));
#47675=CARTESIAN_POINT('Ctrl Pts',(-0.0978126690738567,-4.06320398010117,
-0.00158368662129781));
#47676=CARTESIAN_POINT('Ctrl Pts',(-0.0652084460492417,-4.06358958070638,
-0.560065388179513));
#47677=CARTESIAN_POINT('Ctrl Pts',(-0.0326042230246268,-3.95536025262438,
-1.1181257750272));
#47678=CARTESIAN_POINT('Ctrl Pts',(-1.16714363868065E-14,-3.73764785372991,
-1.62671566533116));
#47679=CARTESIAN_POINT('Origin',(0.,0.,0.));
#47680=CARTESIAN_POINT('Origin',(-32.3478126690739,0.,0.));
#47681=CARTESIAN_POINT('',(-1.59781266907385,-4.07033443134419,0.00376119373461055));
#47682=CARTESIAN_POINT('',(-1.30218733092609,-4.06391640822685,-0.00113170677241647));
#47683=CARTESIAN_POINT('',(-32.3478126690739,-4.0705,-4.82875428449296E-13));
#47684=CARTESIAN_POINT('Ctrl Pts',(-1.59781266907385,-4.07033443134419,
0.00376119373461031));
#47685=CARTESIAN_POINT('Ctrl Pts',(-1.53712695135966,-4.06078738692598,
-1.0307811391412));
#47686=CARTESIAN_POINT('Ctrl Pts',(-1.3968953452724,-3.13350059127503,-3.43660489264461));
#47687=CARTESIAN_POINT('Ctrl Pts',(-1.17711785081205,0.915788038447374,
-4.72632807804377));
#47688=CARTESIAN_POINT('Ctrl Pts',(-0.938480185692821,4.47158639354322,
-1.78518388428051));
#47689=CARTESIAN_POINT('Ctrl Pts',(-0.699842520573601,3.91848486245357,
2.79733082310517));
#47690=CARTESIAN_POINT('Ctrl Pts',(-0.461204855454373,-0.233233057815519,
4.80741524450186));
#47691=CARTESIAN_POINT('Ctrl Pts',(-0.260528238287788,-3.54660683376317,
2.78758749144531));
#47692=CARTESIAN_POINT('Ctrl Pts',(-0.139397509494285,-4.06271216836188,
0.7107281025446));
#47693=CARTESIAN_POINT('Ctrl Pts',(-0.0978126690738567,-4.06320398010117,
-0.00158368662129781));
#47694=CARTESIAN_POINT('',(0.,-2.75129702511903,2.99988915288068));
#47695=CARTESIAN_POINT('Origin',(0.,0.,0.));
#47696=CARTESIAN_POINT('Ctrl Pts',(-1.30218733092609,-4.06391640822685,
-0.00113170677241654));
#47697=CARTESIAN_POINT('Ctrl Pts',(-1.26585432914943,-4.06520244032274,
-0.623026454755739));
#47698=CARTESIAN_POINT('Ctrl Pts',(-1.1499754389997,-3.63835675138479,-2.6046490156767));
#47699=CARTESIAN_POINT('Ctrl Pts',(-0.9545506604769,-0.551158953576692,
-4.78140835552346));
#47700=CARTESIAN_POINT('Ctrl Pts',(-0.715912995357679,3.72696190987269,
-3.05177387808086));
#47701=CARTESIAN_POINT('Ctrl Pts',(-0.477275330238447,4.57725222884596,
1.49154630755727));
#47702=CARTESIAN_POINT('Ctrl Pts',(-0.278410609305757,1.78830202401348,
4.11849926473408));
#47703=CARTESIAN_POINT('Ctrl Pts',(-0.119318832559607,-1.02190788268887,
4.1117895186236));
#47704=CARTESIAN_POINT('Ctrl Pts',(-0.0397729441865359,-2.25151393523441,
3.45825666525491));
#47705=CARTESIAN_POINT('Ctrl Pts',(0.,-2.75129702511903,2.99988915288068));
#47706=CARTESIAN_POINT('Origin',(-32.3478126690739,0.,0.));
#47707=CARTESIAN_POINT('',(-3.09781266907385,-4.07681275190056,-0.00120979165237837));
#47708=CARTESIAN_POINT('',(-2.8021873309261,-4.06949741411341,0.00374292245829216));
#47709=CARTESIAN_POINT('',(-32.3478126690739,-4.0705,-4.82875428449296E-13));
#47710=CARTESIAN_POINT('Ctrl Pts',(-3.09781266907385,-4.07681275190056,
-0.00120979165237874));
#47711=CARTESIAN_POINT('Ctrl Pts',(-3.09394816997118,-4.07706926616768,
-0.0668170824659285));
#47712=CARTESIAN_POINT('Ctrl Pts',(-3.01053778249544,-4.04585841086343,
-1.48261925960601));
#47713=CARTESIAN_POINT('Ctrl Pts',(-2.84758150664664,-2.40317998874982,
-4.17175730007125));
#47714=CARTESIAN_POINT('Ctrl Pts',(-2.60894384152741,2.21026727641583,-4.27709000786183));
#47715=CARTESIAN_POINT('Ctrl Pts',(-2.37030617640818,4.79308872923565,-0.452955592184536));
#47716=CARTESIAN_POINT('Ctrl Pts',(-2.13166851128895,2.97235298759993,3.78734702964848));
#47717=CARTESIAN_POINT('Ctrl Pts',(-1.89303084616973,-1.57913728868941,
4.54806082325786));
#47718=CARTESIAN_POINT('Ctrl Pts',(-1.71507889876469,-3.89136234884321,
1.99954296889815));
#47719=CARTESIAN_POINT('Ctrl Pts',(-1.61667283973273,-4.0733015032319,0.325280748694308));
#47720=CARTESIAN_POINT('Ctrl Pts',(-1.59781266907385,-4.07033443134419,
0.00376119373461031));
#47721=CARTESIAN_POINT('Ctrl Pts',(-2.8021873309261,-4.06949741411341,0.00374292245829196));
#47722=CARTESIAN_POINT('Ctrl Pts',(-2.7431296593879,-4.06042253226819,-1.00355811778553));
#47723=CARTESIAN_POINT('Ctrl Pts',(-2.60452609947661,-3.17339021123584,
-3.38188525686312));
#47724=CARTESIAN_POINT('Ctrl Pts',(-2.38637665119226,0.819002242401078,
-4.74423481374027));
#47725=CARTESIAN_POINT('Ctrl Pts',(-2.14773898607304,4.43395122223712,-1.87597598138563));
#47726=CARTESIAN_POINT('Ctrl Pts',(-1.90910132095381,3.97523440584382,2.71598802545506));
#47727=CARTESIAN_POINT('Ctrl Pts',(-1.67046365583458,-0.135500177452599,
4.81232596646912));
#47728=CARTESIAN_POINT('Ctrl Pts',(-1.46815899249201,-3.51506103565612,
2.84202137248833));
#47729=CARTESIAN_POINT('Ctrl Pts',(-1.34540021752251,-4.06238685777956,
0.738522764518305));
#47730=CARTESIAN_POINT('Ctrl Pts',(-1.30218733092609,-4.06391640822685,
-0.00113170677241654));
#47731=CARTESIAN_POINT('Origin',(-32.3478126690739,0.,0.));
#47732=CARTESIAN_POINT('',(-4.59781266907386,-4.0666555507277,-0.00316262964624325));
#47733=CARTESIAN_POINT('',(-4.30218733092609,-4.0770951458019,-0.000710233193596532));
#47734=CARTESIAN_POINT('',(-32.3478126690739,-4.0705,-4.82875428449296E-13));
#47735=CARTESIAN_POINT('Ctrl Pts',(-4.59781266907386,-4.0666555507277,-0.00316262964624277));
#47736=CARTESIAN_POINT('Ctrl Pts',(-4.57122350020965,-4.06993404787816,
-0.457474827265511));
#47737=CARTESIAN_POINT('Ctrl Pts',(-4.46508844297236,-3.78979273029454,
-2.26701044287803));
#47738=CARTESIAN_POINT('Ctrl Pts',(-4.27940749736198,-1.13066914665236,
-4.67978735413588));
#47739=CARTESIAN_POINT('Ctrl Pts',(-4.04076983224278,3.32562064318893,-3.48124526728007));
#47740=CARTESIAN_POINT('Ctrl Pts',(-3.80213216712354,4.72657132062792,0.915612446800854));
#47741=CARTESIAN_POINT('Ctrl Pts',(-3.56349450200431,1.78509047620951,4.4712723004521));
#47742=CARTESIAN_POINT('Ctrl Pts',(-3.32872133598775,-2.72220888913037,
3.92799287505321));
#47743=CARTESIAN_POINT('Ctrl Pts',(-3.17349405834426,-4.07178924029207,
1.28362707416973));
#47744=CARTESIAN_POINT('Ctrl Pts',(-3.09781266907385,-4.07681275190056,
-0.00120979165237874));
#47745=CARTESIAN_POINT('Ctrl Pts',(-4.30218733092609,-4.0770951458019,-0.000710233193597031));
#47746=CARTESIAN_POINT('Ctrl Pts',(-4.29995087799942,-4.07718638960619,
-0.038671265149509));
#47747=CARTESIAN_POINT('Ctrl Pts',(-4.21816853669967,-4.05948324093355,
-1.42673845965056));
#47748=CARTESIAN_POINT('Ctrl Pts',(-4.05684030702684,-2.48802037989938,
-4.12171998606955));
#47749=CARTESIAN_POINT('Ctrl Pts',(-3.81820264190762,2.12230915839156,-4.32141378384957));
#47750=CARTESIAN_POINT('Ctrl Pts',(-3.5795649767884,4.78281558760628,-0.550907763508576));
#47751=CARTESIAN_POINT('Ctrl Pts',(-3.34092731166917,3.04921617498962,3.72573627855867));
#47752=CARTESIAN_POINT('Ctrl Pts',(-3.10228964654994,-1.48577931367711,
4.57943634031457));
#47753=CARTESIAN_POINT('Ctrl Pts',(-2.92270965296892,-3.87125352580713,
2.05582519611215));
#47754=CARTESIAN_POINT('Ctrl Pts',(-2.82267554776097,-4.07264566127848,
0.35319459559373));
#47755=CARTESIAN_POINT('Ctrl Pts',(-2.8021873309261,-4.06949741411341,0.00374292245829196));
#47756=CARTESIAN_POINT('Origin',(-32.3478126690739,0.,0.));
#47757=CARTESIAN_POINT('',(-6.09781266907385,-4.06532783024481,0.00248275864732798));
#47758=CARTESIAN_POINT('',(-5.80218733092609,-4.06735085704707,-0.00339183732646908));
#47759=CARTESIAN_POINT('',(-32.3478126690739,-4.0705,-4.82875428449296E-13));
#47760=CARTESIAN_POINT('Ctrl Pts',(-6.09781266907385,-4.06532783024481,
0.00248275864732861));
#47761=CARTESIAN_POINT('Ctrl Pts',(-6.0484988304481,-4.06065183816668,-0.840802599870245));
#47762=CARTESIAN_POINT('Ctrl Pts',(-5.91963910344927,-3.39313702767653,
-3.05113638265515));
#47763=CARTESIAN_POINT('Ctrl Pts',(-5.71123348807733,0.233422028762872,
-4.80877700124299));
#47764=CARTESIAN_POINT('Ctrl Pts',(-5.47259582295814,4.171611218274,-2.40343127894775));
#47765=CARTESIAN_POINT('Ctrl Pts',(-5.23395815783889,4.27722630874114,2.21001293857749));
#47766=CARTESIAN_POINT('Ctrl Pts',(-4.99532049271968,0.453235799314355,
4.7930574212978));
#47767=CARTESIAN_POINT('Ctrl Pts',(-4.78327199646466,-3.31468772914499,
3.17542596303663));
#47768=CARTESIAN_POINT('Ctrl Pts',(-4.65076938858272,-4.06012588239192,
0.901675116191023));
#47769=CARTESIAN_POINT('Ctrl Pts',(-4.59781266907386,-4.0666555507277,-0.00316262964624277));
#47770=CARTESIAN_POINT('Ctrl Pts',(-5.80218733092609,-4.06735085704707,
-0.00339183732646849));
#47771=CARTESIAN_POINT('Ctrl Pts',(-5.77722620823787,-4.07069006794027,
-0.429702830878314));
#47772=CARTESIAN_POINT('Ctrl Pts',(-5.67271919717658,-3.81249861092392,
-2.21063503182293));
#47773=CARTESIAN_POINT('Ctrl Pts',(-5.48866629774222,-1.22616783934351,
-4.65567735364785));
#47774=CARTESIAN_POINT('Ctrl Pts',(-5.25002863262297,3.25370797337249,-3.54854948612432));
#47775=CARTESIAN_POINT('Ctrl Pts',(-5.01139096750376,4.74431268704714,0.818728472038551));
#47776=CARTESIAN_POINT('Ctrl Pts',(-4.77275330238453,1.87618665939981,4.43381811498155));
#47777=CARTESIAN_POINT('Ctrl Pts',(-4.53635209019197,-2.67261016863284,
3.97973264573628));
#47778=CARTESIAN_POINT('Ctrl Pts',(-4.3794967663725,-4.07394104096335,1.31152214803601));
#47779=CARTESIAN_POINT('Ctrl Pts',(-4.30218733092609,-4.0770951458019,-0.000710233193597031));
#47780=CARTESIAN_POINT('Origin',(-32.3478126690739,0.,0.));
#47781=CARTESIAN_POINT('',(-7.59781266907386,-4.07574630203772,0.00222153505732406));
#47782=CARTESIAN_POINT('',(-7.3021873309261,-4.06485256559003,0.00211562990566405));
#47783=CARTESIAN_POINT('',(-32.3478126690739,-4.0705,-4.82875428449296E-13));
#47784=CARTESIAN_POINT('Ctrl Pts',(-7.59781266907386,-4.07574630203772,
0.00222153505732401));
#47785=CARTESIAN_POINT('Ctrl Pts',(-7.52577416068655,-4.06771182434402,
-1.22161827070251));
#47786=CARTESIAN_POINT('Ctrl Pts',(-7.37418976392616,-2.82963048299844,
-3.81092663700425));
#47787=CARTESIAN_POINT('Ctrl Pts',(-7.14305947879272,1.57860706315775,-4.5482767971816));
#47788=CARTESIAN_POINT('Ctrl Pts',(-6.90442181367349,4.6797195025539,-1.13094980465497));
#47789=CARTESIAN_POINT('Ctrl Pts',(-6.66578414855425,3.48144476711953,3.32541191686152));
#47790=CARTESIAN_POINT('Ctrl Pts',(-6.42714648343504,-0.91532914635784,
4.72662613694493));
#47791=CARTESIAN_POINT('Ctrl Pts',(-6.23782265694156,-3.7363609545651,2.39316384250277));
#47792=CARTESIAN_POINT('Ctrl Pts',(-6.12804471882117,-4.06819446624524,
0.519462284483144));
#47793=CARTESIAN_POINT('Ctrl Pts',(-6.09781266907385,-4.06532783024481,
0.00248275864732861));
#47794=CARTESIAN_POINT('Ctrl Pts',(-7.3021873309261,-4.06485256559003,0.0021156299056644));
#47795=CARTESIAN_POINT('Ctrl Pts',(-7.25450153847633,-4.06102628102932,
-0.813568030876496));
#47796=CARTESIAN_POINT('Ctrl Pts',(-7.12726985765349,-3.42680090686785,
-2.99539080099765));
#47797=CARTESIAN_POINT('Ctrl Pts',(-6.92049228845756,0.134999037069343,
-4.81254552210429));
#47798=CARTESIAN_POINT('Ctrl Pts',(-6.68185462333835,4.1215704771241,-2.48826765871595));
#47799=CARTESIAN_POINT('Ctrl Pts',(-6.44321695821911,4.32154162229638,2.12205022265777));
#47800=CARTESIAN_POINT('Ctrl Pts',(-6.20457929309988,0.551193473920355,
4.78278213002022));
#47801=CARTESIAN_POINT('Ctrl Pts',(-5.99090275066888,-3.27821055126197,
3.23074519309206));
#47802=CARTESIAN_POINT('Ctrl Pts',(-5.85677209661095,-4.06004869975013,
0.928861330231892));
#47803=CARTESIAN_POINT('Ctrl Pts',(-5.80218733092609,-4.06735085704707,
-0.00339183732646849));
#47804=CARTESIAN_POINT('Origin',(-32.3478126690739,0.,0.));
#47805=CARTESIAN_POINT('',(-9.09781266907386,-4.07222943229488,-0.00357906261956567));
#47806=CARTESIAN_POINT('',(-8.8021873309261,-4.07511392925337,0.00260772300212458));
#47807=CARTESIAN_POINT('',(-32.3478126690739,-4.0705,-4.82875428449296E-13));
#47808=CARTESIAN_POINT('Ctrl Pts',(-9.09781266907386,-4.07222943229488,
-0.003579062619565));
#47809=CARTESIAN_POINT('Ctrl Pts',(-9.08259537929808,-4.07461348194488,
-0.262682434050171));
#47810=CARTESIAN_POINT('Ctrl Pts',(-8.98783220114923,-3.93387284883695,
-1.87362564859038));
#47811=CARTESIAN_POINT('Ctrl Pts',(-8.8135231346273,-1.78562688897607,-4.47105789459565));
#47812=CARTESIAN_POINT('Ctrl Pts',(-8.57488546950807,2.79593183551325,-3.91938608134342));
#47813=CARTESIAN_POINT('Ctrl Pts',(-8.33624780438884,4.80879098967182,0.233133655034067));
#47814=CARTESIAN_POINT('Ctrl Pts',(-8.09761013926962,2.40368143941586,4.17146708260569));
#47815=CARTESIAN_POINT('Ctrl Pts',(-7.85897247415039,-2.20975644067261,
4.27735882951057));
#47816=CARTESIAN_POINT('Ctrl Pts',(-7.69237331741847,-4.01320701615423,
1.60783980898199));
#47817=CARTESIAN_POINT('Ctrl Pts',(-7.60532004905963,-4.07658360250915,
0.129762077875785));
#47818=CARTESIAN_POINT('Ctrl Pts',(-7.59781266907386,-4.07574630203772,
0.00222153505732401));
#47819=CARTESIAN_POINT('Ctrl Pts',(-8.8021873309261,-4.07511392925337,0.00260772300212448));
#47820=CARTESIAN_POINT('Ctrl Pts',(-8.73177686871478,-4.06620451024253,
-1.1940613554039));
#47821=CARTESIAN_POINT('Ctrl Pts',(-8.58182051813039,-2.87606084879853,
-3.7580704643467));
#47822=CARTESIAN_POINT('Ctrl Pts',(-8.35231827917293,1.48523158453539,-4.57961857379977));
#47823=CARTESIAN_POINT('Ctrl Pts',(-8.1136806140537,4.65560380841346,-1.22644703115444));
#47824=CARTESIAN_POINT('Ctrl Pts',(-7.87504294893448,3.54874460969979,3.25349517231261));
#47825=CARTESIAN_POINT('Ctrl Pts',(-7.63640528381524,-0.818443985601727,
4.74436176780107));
#47826=CARTESIAN_POINT('Ctrl Pts',(-7.44545341114579,-3.71128559220026,
2.44953276936589));
#47827=CARTESIAN_POINT('Ctrl Pts',(-7.33404742684941,-4.06740900403576,
0.547094717816802));
#47828=CARTESIAN_POINT('Ctrl Pts',(-7.3021873309261,-4.06485256559003,0.0021156299056644));
#47829=CARTESIAN_POINT('Origin',(-32.3478126690739,0.,0.));
#47830=CARTESIAN_POINT('',(-10.5978126690739,-4.06383028861155,-0.000517316456022591));
#47831=CARTESIAN_POINT('',(-10.3021873309261,-4.07305647823417,-0.00339818811806003));
#47832=CARTESIAN_POINT('',(-32.3478126690739,-4.0705,-4.82875428449296E-13));
#47833=CARTESIAN_POINT('Ctrl Pts',(-10.5978126690739,-4.06383028861155,
-0.000517316456022585));
#47834=CARTESIAN_POINT('Ctrl Pts',(-10.5598707095365,-4.06456413075875,
-0.649936894253117));
#47835=CARTESIAN_POINT('Ctrl Pts',(-10.4423828616261,-3.6108734382595,-2.65990611006904));
#47836=CARTESIAN_POINT('Ctrl Pts',(-10.2453491253427,-0.453810659605433,
-4.79300302197796));
#47837=CARTESIAN_POINT('Ctrl Pts',(-10.0067114602234,3.78679836713871,-2.97304224828663));
#47838=CARTESIAN_POINT('Ctrl Pts',(-9.76807379510421,4.54837145493611,1.57833430913225));
#47839=CARTESIAN_POINT('Ctrl Pts',(-9.52943612998497,1.131230436189,4.67965167333008));
#47840=CARTESIAN_POINT('Ctrl Pts',(-9.30601575464153,-3.04102820872573,
3.55803793366217));
#47841=CARTESIAN_POINT('Ctrl Pts',(-9.16214126767116,-4.06215125311643,
1.09173797619339));
#47842=CARTESIAN_POINT('Ctrl Pts',(-9.09781266907386,-4.07222943229488,
-0.003579062619565));
#47843=CARTESIAN_POINT('Ctrl Pts',(-10.3021873309261,-4.07305647823417,
-0.00339818811806027));
#47844=CARTESIAN_POINT('Ctrl Pts',(-10.2885980873263,-4.07512744307457,
-0.234659625407061));
#47845=CARTESIAN_POINT('Ctrl Pts',(-10.1954629553534,-3.95181437733735,
-1.8174227959994));
#47846=CARTESIAN_POINT('Ctrl Pts',(-10.0227819350075,-1.8767184363934,-4.43359301827195));
#47847=CARTESIAN_POINT('Ctrl Pts',(-9.78414426988828,2.71516687463254,-3.97576256635973));
#47848=CARTESIAN_POINT('Ctrl Pts',(-9.54550660476906,4.8125536089566,0.134710437930172));
#47849=CARTESIAN_POINT('Ctrl Pts',(-9.30686893964983,2.48851481691486,4.12142125330121));
#47850=CARTESIAN_POINT('Ctrl Pts',(-9.06823127453061,-2.12179106496689,
4.32166886952238));
#47851=CARTESIAN_POINT('Ctrl Pts',(-8.9000040716227,-3.99762873478501,1.66388105000583));
#47852=CARTESIAN_POINT('Ctrl Pts',(-8.81132275708786,-4.07626988444755,
0.157869905105551));
#47853=CARTESIAN_POINT('Ctrl Pts',(-8.8021873309261,-4.07511392925337,0.00260772300212448));
#47854=CARTESIAN_POINT('Origin',(-32.3478126690739,0.,0.));
#47855=CARTESIAN_POINT('',(-12.0978126690739,-4.07032458744755,0.00376143334710477));
#47856=CARTESIAN_POINT('',(-11.8021873309261,-4.06398132384238,-0.00096959209926889));
#47857=CARTESIAN_POINT('',(-32.3478126690739,-4.0705,-4.82875428449296E-13));
#47858=CARTESIAN_POINT('Ctrl Pts',(-12.0978126690739,-4.07032458744755,
0.00376143334710491));
#47859=CARTESIAN_POINT('Ctrl Pts',(-12.037146039775,-4.06079261000553,-1.03044389103757));
#47860=CARTESIAN_POINT('Ctrl Pts',(-11.8969335221031,-3.13401642257978,
-3.43588983608773));
#47861=CARTESIAN_POINT('Ctrl Pts',(-11.677175116058,0.914762246840484,-4.7267358838015));
#47862=CARTESIAN_POINT('Ctrl Pts',(-11.4385374509388,4.47095080603802,-1.78589500627826));
#47863=CARTESIAN_POINT('Ctrl Pts',(-11.1998997858196,3.91955374080681,2.79569679264203));
#47864=CARTESIAN_POINT('Ctrl Pts',(-10.9612621207003,-0.232845280914501,
4.80880496159049));
#47865=CARTESIAN_POINT('Ctrl Pts',(-10.7605664151184,-3.54512857250201,
2.78629205291713));
#47866=CARTESIAN_POINT('Ctrl Pts',(-10.6394165979096,-4.06302561966876,
0.711581010269389));
#47867=CARTESIAN_POINT('Ctrl Pts',(-10.5978126690739,-4.06383028861155,
-0.000517316456022585));
#47868=CARTESIAN_POINT('Ctrl Pts',(-11.8021873309261,-4.06398132384238,
-0.000969592099269029));
#47869=CARTESIAN_POINT('Ctrl Pts',(-11.7658734175648,-4.06530044997824,
-0.622465582635642));
#47870=CARTESIAN_POINT('Ctrl Pts',(-11.6500136158304,-3.63881171341208,
-2.60363619702803));
#47871=CARTESIAN_POINT('Ctrl Pts',(-11.4546079257229,-0.551767098271795,
-4.78271598680431));
#47872=CARTESIAN_POINT('Ctrl Pts',(-11.2159702606036,3.72518553231084,-3.04988719316482));
#47873=CARTESIAN_POINT('Ctrl Pts',(-10.9773325954844,4.57970763196809,1.48495695118139));
#47874=CARTESIAN_POINT('Ctrl Pts',(-10.7386949303652,1.22672621632081,4.65553025243742));
#47875=CARTESIAN_POINT('Ctrl Pts',(-10.5136465088458,-2.99816785865763,
3.6119546083943));
#47876=CARTESIAN_POINT('Ctrl Pts',(-10.3681439756994,-4.06300485973803,
1.11905048660218));
#47877=CARTESIAN_POINT('Ctrl Pts',(-10.3021873309261,-4.07305647823417,
-0.00339818811806027));
#47878=CARTESIAN_POINT('Origin',(-32.3478126690739,0.,0.));
#47879=CARTESIAN_POINT('',(-13.5978126690739,-4.07681666553846,-0.0012043583654883));
#47880=CARTESIAN_POINT('',(-13.3021873309261,-4.06948780842451,0.00374258894561955));
#47881=CARTESIAN_POINT('',(-32.3478126690739,-4.0705,-4.82875428449296E-13));
#47882=CARTESIAN_POINT('Ctrl Pts',(-13.5978126690739,-4.07681666553846,
-0.00120435836548843));
#47883=CARTESIAN_POINT('Ctrl Pts',(-13.5939672583865,-4.07707083999085,
-0.0664874041950833));
#47884=CARTESIAN_POINT('Ctrl Pts',(-13.5105759593261,-4.04602154531668,
-1.48196385087443));
#47885=CARTESIAN_POINT('Ctrl Pts',(-13.3476387718926,-2.40418173141341,
-4.17117876454601));
#47886=CARTESIAN_POINT('Ctrl Pts',(-13.1090011067734,2.20924341525388,-4.27762382820403));
#47887=CARTESIAN_POINT('Ctrl Pts',(-12.8703634416541,4.79297579923065,-0.454098085715957));
#47888=CARTESIAN_POINT('Ctrl Pts',(-12.6317257765349,2.97326932976115,3.78662007285696));
#47889=CARTESIAN_POINT('Ctrl Pts',(-12.3930881114157,-1.57806154943975,
4.54846609634954));
#47890=CARTESIAN_POINT('Ctrl Pts',(-12.2151170755953,-3.89111272737449,
2.00017169269057));
#47891=CARTESIAN_POINT('Ctrl Pts',(-12.1166919281481,-4.07329090803759,
0.325602789635245));
#47892=CARTESIAN_POINT('Ctrl Pts',(-12.0978126690739,-4.07032458744755,
0.00376143334710491));
#47893=CARTESIAN_POINT('Ctrl Pts',(-13.3021873309261,-4.06948780842451,
0.00374258894561951));
#47894=CARTESIAN_POINT('Ctrl Pts',(-13.2431487478032,-4.06042005381897,
-1.00323625051947));
#47895=CARTESIAN_POINT('Ctrl Pts',(-13.1045642763073,-3.17385622399582,
-3.38123201716333));
#47896=CARTESIAN_POINT('Ctrl Pts',(-12.8864339164382,0.817874959696777,
-4.74445989460021));
#47897=CARTESIAN_POINT('Ctrl Pts',(-12.647796251319,4.43348046720131,-1.87698430683722));
#47898=CARTESIAN_POINT('Ctrl Pts',(-12.4091585861998,3.9759253824068,2.71492845112022));
#47899=CARTESIAN_POINT('Ctrl Pts',(-12.1705209210805,-0.134421838351238,
4.81256167862222));
#47900=CARTESIAN_POINT('Ctrl Pts',(-11.9681971693227,-3.51458600877433,
2.84237865671728));
#47901=CARTESIAN_POINT('Ctrl Pts',(-11.8454193059378,-4.06241089469102,
0.738925854183665));
#47902=CARTESIAN_POINT('Ctrl Pts',(-11.8021873309261,-4.06398132384238,
-0.000969592099269029));
#47903=CARTESIAN_POINT('Origin',(-32.3478126690739,0.,0.));
#47904=CARTESIAN_POINT('',(-15.0978126690739,-4.06666337103388,-0.00316560979000432));
#47905=CARTESIAN_POINT('',(-14.8021873309261,-4.07709762639944,-0.00070430106655972));
#47906=CARTESIAN_POINT('',(-32.3478126690739,-4.0705,-4.82875428449296E-13));
#47907=CARTESIAN_POINT('Ctrl Pts',(-15.0978126690739,-4.06666337103388,
-0.00316560979000423));
#47908=CARTESIAN_POINT('Ctrl Pts',(-15.071242588625,-4.06994301140227,-0.457149458338325));
#47909=CARTESIAN_POINT('Ctrl Pts',(-14.965126619803,-3.79006310537379,-2.26634942371038));
#47910=CARTESIAN_POINT('Ctrl Pts',(-14.7794647626079,-1.13179168699179,
-4.67951596436188));
#47911=CARTESIAN_POINT('Ctrl Pts',(-14.5408270974888,3.32478553700414,-3.48204296590229));
#47912=CARTESIAN_POINT('Ctrl Pts',(-14.3021894323695,4.72679073178803,0.914478792178541));
#47913=CARTESIAN_POINT('Ctrl Pts',(-14.0635517672503,1.78616311715816,4.47084370140194));
#47914=CARTESIAN_POINT('Ctrl Pts',(-13.8287595128184,-2.72163337242562,
3.9286021789031));
#47915=CARTESIAN_POINT('Ctrl Pts',(-13.6735131467596,-4.07181300558473,
1.28395297745419));
#47916=CARTESIAN_POINT('Ctrl Pts',(-13.5978126690739,-4.07681666553846,
-0.00120435836548843));
#47917=CARTESIAN_POINT('Ctrl Pts',(-14.8021873309261,-4.07709762639944,
-0.000704301066560046));
#47918=CARTESIAN_POINT('Ctrl Pts',(-14.7999699664147,-4.07718738154795,
-0.0383412680213716));
#47919=CARTESIAN_POINT('Ctrl Pts',(-14.7182067135303,-4.05963949617112,
-1.42608358607219));
#47920=CARTESIAN_POINT('Ctrl Pts',(-14.5568975722728,-2.48900910600372,
-4.12112276102026));
#47921=CARTESIAN_POINT('Ctrl Pts',(-14.3182599071536,2.12127272581082,-4.32192331767929));
#47922=CARTESIAN_POINT('Ctrl Pts',(-14.0796222420344,4.78268288982128,-0.552053907312987));
#47923=CARTESIAN_POINT('Ctrl Pts',(-13.8409845769151,3.05011057970114,3.72500262990027));
#47924=CARTESIAN_POINT('Ctrl Pts',(-13.6023469117959,-1.48468231248816,
4.57979667366944));
#47925=CARTESIAN_POINT('Ctrl Pts',(-13.4227478297996,-3.8710120869076,2.05648068706029));
#47926=CARTESIAN_POINT('Ctrl Pts',(-13.3226946361763,-4.0726375319069,0.353521010938116));
#47927=CARTESIAN_POINT('Ctrl Pts',(-13.3021873309261,-4.06948780842451,
0.00374258894561951));
#47928=CARTESIAN_POINT('Origin',(-32.3478126690739,0.,0.));
#47929=CARTESIAN_POINT('',(-16.5978126690739,-4.06532180994014,0.00247865735123198));
#47930=CARTESIAN_POINT('',(-16.3021873309261,-4.06735933458706,-0.00339422375240483));
#47931=CARTESIAN_POINT('',(-32.3478126690739,-4.0705,-4.82875428449296E-13));
#47932=CARTESIAN_POINT('Ctrl Pts',(-16.5978126690739,-4.06532180994014,
0.00247865735123177));
#47933=CARTESIAN_POINT('Ctrl Pts',(-16.5485179188634,-4.06065576655941,
-0.840483409511789));
#47934=CARTESIAN_POINT('Ctrl Pts',(-16.4196772802799,-3.39353668499773,
-3.05048344280494));
#47935=CARTESIAN_POINT('Ctrl Pts',(-16.2112907533233,0.232268530165553,
-4.80883285354733));
#47936=CARTESIAN_POINT('Ctrl Pts',(-15.9726530882041,4.17103458301497,-2.40443186444421));
#47937=CARTESIAN_POINT('Ctrl Pts',(-15.7340154230849,4.27775630447756,2.20898689062749));
#47938=CARTESIAN_POINT('Ctrl Pts',(-15.4953777579657,0.454385510193501,
4.79294855924697));
#47939=CARTESIAN_POINT('Ctrl Pts',(-15.2833101732953,-3.31426516276753,
3.17607544524493));
#47940=CARTESIAN_POINT('Ctrl Pts',(-15.1507884769981,-4.06012437697437,
0.9019939062919));
#47941=CARTESIAN_POINT('Ctrl Pts',(-15.0978126690739,-4.06666337103388,
-0.00316560979000423));
#47942=CARTESIAN_POINT('Ctrl Pts',(-16.3021873309261,-4.06735933458706,
-0.0033942237524047));
#47943=CARTESIAN_POINT('Ctrl Pts',(-16.2772452966532,-4.07069882146085,
-0.42937696578519));
#47944=CARTESIAN_POINT('Ctrl Pts',(-16.1727573740072,-3.81276059892577,
-2.20997410073169));
#47945=CARTESIAN_POINT('Ctrl Pts',(-15.9887235629882,-1.22728457340874,
-4.65538309025602));
#47946=CARTESIAN_POINT('Ctrl Pts',(-15.7500858978689,3.25285668605437,-3.54932986930775));
#47947=CARTESIAN_POINT('Ctrl Pts',(-15.5114482327497,4.74450893241555,0.817590442335157));
#47948=CARTESIAN_POINT('Ctrl Pts',(-15.2728105676305,1.8772501705311,4.43336790018713));
#47949=CARTESIAN_POINT('Ctrl Pts',(-15.0363902670226,-2.67202280013241,
3.98033711867999));
#47950=CARTESIAN_POINT('Ctrl Pts',(-14.8795158547878,-4.07396749912098,
1.31184989664949));
#47951=CARTESIAN_POINT('Ctrl Pts',(-14.8021873309261,-4.07709762639944,
-0.000704301066560046));
#47952=CARTESIAN_POINT('Origin',(-32.3478126690739,0.,0.));
#47953=CARTESIAN_POINT('',(-18.0978126690739,-4.0757393762113,0.00222632843356818));
#47954=CARTESIAN_POINT('',(-17.8021873309261,-4.06484746876737,0.00211112861108809));
#47955=CARTESIAN_POINT('',(-32.3478126690739,-4.0705,-4.82875428449296E-13));
#47956=CARTESIAN_POINT('Ctrl Pts',(-18.0978126690739,-4.0757393762113,0.00222632843356826));
#47957=CARTESIAN_POINT('Ctrl Pts',(-18.0257932491019,-4.06769305643308,
-1.22129466881777));
#47958=CARTESIAN_POINT('Ctrl Pts',(-17.8742279407568,-2.83018048694797,
-3.8103087610216));
#47959=CARTESIAN_POINT('Ctrl Pts',(-17.6431167440387,1.5775160130308,-4.54865533010503));
#47960=CARTESIAN_POINT('Ctrl Pts',(-17.4044790789195,4.6794480846352,-1.13207230628853));
#47961=CARTESIAN_POINT('Ctrl Pts',(-17.1658414138002,3.48224234046452,3.3245767197852));
#47962=CARTESIAN_POINT('Ctrl Pts',(-16.927203748681,-0.914195334228,4.72684556277623));
#47963=CARTESIAN_POINT('Ctrl Pts',(-16.7378608337722,-3.73607127850369,
2.39382482140684));
#47964=CARTESIAN_POINT('Ctrl Pts',(-16.6280638072365,-4.06818526137017,
0.519786521610059));
#47965=CARTESIAN_POINT('Ctrl Pts',(-16.5978126690739,-4.06532180994014,
0.00247865735123177));
#47966=CARTESIAN_POINT('Ctrl Pts',(-17.8021873309261,-4.06484746876737,
0.00211112861108823));
#47967=CARTESIAN_POINT('Ctrl Pts',(-17.7545206268917,-4.0610311343114,-0.813248574751964));
#47968=CARTESIAN_POINT('Ctrl Pts',(-17.6273080344841,-3.42719055604098,
-2.99473654818825));
#47969=CARTESIAN_POINT('Ctrl Pts',(-17.4205495537035,0.133844637744424,
-4.81257776603306));
#47970=CARTESIAN_POINT('Ctrl Pts',(-17.1819118885843,4.1209734926491,-2.4892562371223));
#47971=CARTESIAN_POINT('Ctrl Pts',(-16.9432742234651,4.32205051844462,2.12101354478971));
#47972=CARTESIAN_POINT('Ctrl Pts',(-16.7046365583459,0.55234071436891,4.78264977563894));
#47973=CARTESIAN_POINT('Ctrl Pts',(-16.4909409274995,-3.27777761810244,
3.23139288635401));
#47974=CARTESIAN_POINT('Ctrl Pts',(-16.3567911850263,-4.06004842914805,
0.929180049887315));
#47975=CARTESIAN_POINT('Ctrl Pts',(-16.3021873309261,-4.06735933458706,
-0.0033942237524047));
#47976=CARTESIAN_POINT('Origin',(-32.3478126690739,0.,0.));
#47977=CARTESIAN_POINT('',(-19.5978126690739,-4.07223926118534,-0.00357729417079465));
#47978=CARTESIAN_POINT('',(-19.3021873309261,-4.07510605262456,0.00261196768466351));
#47979=CARTESIAN_POINT('',(-32.3478126690739,-4.0705,-4.82875428449296E-13));
#47980=CARTESIAN_POINT('Ctrl Pts',(-19.5978126690739,-4.07223926118534,
-0.00357729417079473));
#47981=CARTESIAN_POINT('Ctrl Pts',(-19.5826144677134,-4.07461978933759,
-0.262354039634738));
#47982=CARTESIAN_POINT('Ctrl Pts',(-19.4878703779799,-3.9340869821028,-1.87296646703573));
#47983=CARTESIAN_POINT('Ctrl Pts',(-19.3135803998733,-1.78669931964703,
-4.4706294438965));
#47984=CARTESIAN_POINT('Ctrl Pts',(-19.074942734754,2.79499160370957,-3.92005663462335));
#47985=CARTESIAN_POINT('Ctrl Pts',(-18.8363050696348,4.80884677358576,0.231980153537627));
#47986=CARTESIAN_POINT('Ctrl Pts',(-18.5976674045156,2.4046819888283,4.1708903864842));
#47987=CARTESIAN_POINT('Ctrl Pts',(-18.3590297393964,-2.20873035805718,
4.27788876536757));
#47988=CARTESIAN_POINT('Ctrl Pts',(-18.1924114942491,-4.01302793193152,
1.60849660347309));
#47989=CARTESIAN_POINT('Ctrl Pts',(-18.1053391374749,-4.07658026567666,
0.130091730952273));
#47990=CARTESIAN_POINT('Ctrl Pts',(-18.0978126690739,-4.0757393762113,0.00222632843356826));
#47991=CARTESIAN_POINT('Ctrl Pts',(-19.3021873309261,-4.07510605262456,
0.00261196768466343));
#47992=CARTESIAN_POINT('Ctrl Pts',(-19.2317959571301,-4.06618795069759,
-1.19373875342118));
#47993=CARTESIAN_POINT('Ctrl Pts',(-19.081858694961,-2.87659949644564,-3.75744888720017));
#47994=CARTESIAN_POINT('Ctrl Pts',(-18.8523755444189,1.48413301908516,-4.57997470766269));
#47995=CARTESIAN_POINT('Ctrl Pts',(-18.6137378792997,4.6553094840529,-1.22756374533297));
#47996=CARTESIAN_POINT('Ctrl Pts',(-18.3751002141804,3.54952493031783,3.25264383390203));
#47997=CARTESIAN_POINT('Ctrl Pts',(-18.1364625490612,-0.817305922033317,
4.74455795316888));
#47998=CARTESIAN_POINT('Ctrl Pts',(-17.9454915879764,-3.71098714745764,
2.45019360063996));
#47999=CARTESIAN_POINT('Ctrl Pts',(-17.8340665152647,-4.06739980864662,
0.547418441384662));
#48000=CARTESIAN_POINT('Ctrl Pts',(-17.8021873309261,-4.06484746876737,
0.00211112861108823));
#48001=CARTESIAN_POINT('Origin',(-32.3478126690739,0.,0.));
#48002=CARTESIAN_POINT('',(-21.0978126690739,-4.06383152666866,-0.000522675918812766));
#48003=CARTESIAN_POINT('',(-20.8021873309261,-4.07306601825716,-0.00339571005182004));
#48004=CARTESIAN_POINT('',(-32.3478126690739,-4.0705,-4.82875428449296E-13));
#48005=CARTESIAN_POINT('Ctrl Pts',(-21.0978126690739,-4.06383152666866,
-0.00052267591881365));
#48006=CARTESIAN_POINT('Ctrl Pts',(-21.0598897979519,-4.06457261097563,
-0.649615040927229));
#48007=CARTESIAN_POINT('Ctrl Pts',(-20.9424210384568,-3.6112055683889,-2.65924661123667));
#48008=CARTESIAN_POINT('Ctrl Pts',(-20.7454063905886,-0.454960354245989,
-4.79289402757069));
#48009=CARTESIAN_POINT('Ctrl Pts',(-20.5067687254694,3.78608510831067,-2.97395051002756));
#48010=CARTESIAN_POINT('Ctrl Pts',(-20.2681310603502,4.54874992244621,1.57724323631644));
#48011=CARTESIAN_POINT('Ctrl Pts',(-20.0294933952309,1.13235292151423,4.67938018808041));
#48012=CARTESIAN_POINT('Ctrl Pts',(-19.8060539314722,-3.04053113635729,
3.55867154707108));
#48013=CARTESIAN_POINT('Ctrl Pts',(-19.6621603560865,-4.06216033955295,
1.09205794767961));
#48014=CARTESIAN_POINT('Ctrl Pts',(-19.5978126690739,-4.07223926118534,
-0.00357729417079473));
#48015=CARTESIAN_POINT('Ctrl Pts',(-20.8021873309261,-4.07306601825716,
-0.0033957100518197));
#48016=CARTESIAN_POINT('Ctrl Pts',(-20.7886171757417,-4.07513318091976,
-0.234330901384573));
#48017=CARTESIAN_POINT('Ctrl Pts',(-20.6955011321841,-3.95202089787016,
-1.81676406404286));
#48018=CARTESIAN_POINT('Ctrl Pts',(-20.5228392002535,-1.87778187766528,
-4.43314271832978));
#48019=CARTESIAN_POINT('Ctrl Pts',(-20.2842015351343,2.71421312200688,-3.97641374475733));
#48020=CARTESIAN_POINT('Ctrl Pts',(-20.045563870015,4.81258578377826,0.133556036718511));
#48021=CARTESIAN_POINT('Ctrl Pts',(-19.8069262048958,2.48950335928912,4.12082420945821));
#48022=CARTESIAN_POINT('Ctrl Pts',(-19.5682885397766,-2.12075435614108,
4.32217770366716));
#48023=CARTESIAN_POINT('Ctrl Pts',(-19.4000422484533,-3.99744242114115,
1.66453839875525));
#48024=CARTESIAN_POINT('Ctrl Pts',(-19.3113418455032,-4.07626586652913,
0.158199357517422));
#48025=CARTESIAN_POINT('Ctrl Pts',(-19.3021873309261,-4.07510605262456,
0.00261196768466343));
#48026=CARTESIAN_POINT('Origin',(-32.3478126690739,0.,0.));
#48027=CARTESIAN_POINT('',(-22.5978126690739,-4.07031468847398,0.00376156571352546));
#48028=CARTESIAN_POINT('',(-22.3021873309261,-4.06398364289261,-0.000974823831897398));
#48029=CARTESIAN_POINT('',(-32.3478126690739,-4.0705,-4.82875428449296E-13));
#48030=CARTESIAN_POINT('Ctrl Pts',(-22.5978126690739,-4.07031468847398,
0.00376156571352537));
#48031=CARTESIAN_POINT('Ctrl Pts',(-22.5371651281903,-4.06078745327604,
-1.03012477253975));
#48032=CARTESIAN_POINT('Ctrl Pts',(-22.3969716989337,-3.13448885277667,
-3.4352501825917));
#48033=CARTESIAN_POINT('Ctrl Pts',(-22.177232381304,0.913628408435968,-4.7269551737383));
#48034=CARTESIAN_POINT('Ctrl Pts',(-21.9385947161847,4.47052229104313,-1.7869674112637));
#48035=CARTESIAN_POINT('Ctrl Pts',(-21.6999570510656,3.92022423769407,2.79475652063351));
#48036=CARTESIAN_POINT('Ctrl Pts',(-21.4613193859463,-0.231691776071347,
4.80886067632815));
#48037=CARTESIAN_POINT('Ctrl Pts',(-21.2606045919491,-3.54477519825892,
2.78695006207459));
#48038=CARTESIAN_POINT('Ctrl Pts',(-21.1394356863249,-4.06301813453931,
0.71190182958246));
#48039=CARTESIAN_POINT('Ctrl Pts',(-21.0978126690739,-4.06383152666866,
-0.00052267591881365));
#48040=CARTESIAN_POINT('Ctrl Pts',(-22.3021873309261,-4.06398364289261,
-0.000974823831896773));
#48041=CARTESIAN_POINT('Ctrl Pts',(-22.2658925059801,-4.06530923181794,
-0.622143240829621));
#48042=CARTESIAN_POINT('Ctrl Pts',(-22.150051792661,-3.63913463819147,-2.60297621081044));
#48043=CARTESIAN_POINT('Ctrl Pts',(-21.9546651909688,-0.552914322524486,
-4.78258349567352));
#48044=CARTESIAN_POINT('Ctrl Pts',(-21.7160275258496,3.72445384229878,-3.05078067349642));
#48045=CARTESIAN_POINT('Ctrl Pts',(-21.4773898607304,4.58006369995296,1.4838583643783));
#48046=CARTESIAN_POINT('Ctrl Pts',(-21.2387521956112,1.22784291284316,4.65523586110807));
#48047=CARTESIAN_POINT('Ctrl Pts',(-21.0136846856764,-2.99765973840581,
3.61258525206308));
#48048=CARTESIAN_POINT('Ctrl Pts',(-20.8681630641147,-4.06301583309485,
1.11937100559103));
#48049=CARTESIAN_POINT('Ctrl Pts',(-20.8021873309261,-4.07306601825716,
-0.0033957100518197));
#48050=CARTESIAN_POINT('Origin',(-32.3478126690739,0.,0.));
#48051=CARTESIAN_POINT('',(-24.0978126690739,-4.07682073202661,-0.00119862600692145));
#48052=CARTESIAN_POINT('',(-23.8021873309261,-4.06947811712022,0.00374200930701507));
#48053=CARTESIAN_POINT('',(-32.3478126690739,-4.0705,-4.82875428449296E-13));
#48054=CARTESIAN_POINT('Ctrl Pts',(-24.0978126690739,-4.07682073202661,
-0.0011986260069221));
#48055=CARTESIAN_POINT('Ctrl Pts',(-24.0939863468019,-4.07707257100012,
-0.0661574373907974));
#48056=CARTESIAN_POINT('Ctrl Pts',(-24.0106141361567,-4.04618464425921,
-1.48130837178561));
#48057=CARTESIAN_POINT('Ctrl Pts',(-23.8476960371386,-2.40518220884904,
-4.17060195021093));
#48058=CARTESIAN_POINT('Ctrl Pts',(-23.6090583720194,2.20821726762825,-4.27815364006511));
#48059=CARTESIAN_POINT('Ctrl Pts',(-23.3704207069001,4.7928667366398,-0.455247774302161));
#48060=CARTESIAN_POINT('Ctrl Pts',(-23.1317830417809,2.97417754833123,3.7859067598156));
#48061=CARTESIAN_POINT('Ctrl Pts',(-22.8931453766616,-1.57697045372341,
4.54884449829819));
#48062=CARTESIAN_POINT('Ctrl Pts',(-22.715155252426,-3.89088098364765,2.00083174485514));
#48063=CARTESIAN_POINT('Ctrl Pts',(-22.6167110165634,-4.07328346509314,
0.325930329695141));
#48064=CARTESIAN_POINT('Ctrl Pts',(-22.5978126690739,-4.07031468847398,
0.00376156571352537));
#48065=CARTESIAN_POINT('Ctrl Pts',(-23.8021873309261,-4.06947811712022,
0.00374200930701521));
#48066=CARTESIAN_POINT('Ctrl Pts',(-23.7431678362185,-4.06041648348459,
-1.00291735298318));
#48067=CARTESIAN_POINT('Ctrl Pts',(-23.6046024531379,-3.17431791098803,
-3.38058997938746));
#48068=CARTESIAN_POINT('Ctrl Pts',(-23.3864911816842,0.816736872430108,
-4.74465594332464));
#48069=CARTESIAN_POINT('Ctrl Pts',(-23.1478535165649,4.43303010358293,-1.87804772118901));
#48070=CARTESIAN_POINT('Ctrl Pts',(-22.9092158514458,3.97657650355884,2.71397465949093));
#48071=CARTESIAN_POINT('Ctrl Pts',(-22.6705781863265,-0.13326743518637,
4.81259378419344));
#48072=CARTESIAN_POINT('Ctrl Pts',(-22.4682353461533,-3.5142230495247,2.84303582389633));
#48073=CARTESIAN_POINT('Ctrl Pts',(-22.3454383943532,-4.06240399260436,
0.739246258441231));
#48074=CARTESIAN_POINT('Ctrl Pts',(-22.3021873309261,-4.06398364289261,
-0.000974823831896773));
#48075=CARTESIAN_POINT('Origin',(-32.3478126690739,0.,0.));
#48076=CARTESIAN_POINT('',(-25.5978126690739,-4.06667116509479,-0.00316860155561062));
#48077=CARTESIAN_POINT('',(-25.3021873309261,-4.07710011149971,-0.000698316132069499));
#48078=CARTESIAN_POINT('',(-32.3478126690739,-4.0705,-4.82875428449296E-13));
#48079=CARTESIAN_POINT('Ctrl Pts',(-25.5978126690739,-4.06667116509479,
-0.00316860155561056));
#48080=CARTESIAN_POINT('Ctrl Pts',(-25.5712616770403,-4.06995198256812,
-0.456824073053871));
#48081=CARTESIAN_POINT('Ctrl Pts',(-25.4651647966337,-3.79033356389561,
-2.26568828448685));
#48082=CARTESIAN_POINT('Ctrl Pts',(-25.2795220278539,-1.132913999441,-4.67924443383647));
#48083=CARTESIAN_POINT('Ctrl Pts',(-25.0408843627347,3.32395012330801,-3.48284034246832));
#48084=CARTESIAN_POINT('Ctrl Pts',(-24.8022466976155,4.72700999182265,0.913344916409211));
#48085=CARTESIAN_POINT('Ctrl Pts',(-24.5636090324962,1.78723547660136,4.47041513471273));
#48086=CARTESIAN_POINT('Ctrl Pts',(-24.3287976896491,-2.72105741290232,
3.9292109076427));
#48087=CARTESIAN_POINT('Ctrl Pts',(-24.1735322351749,-4.07183705933901,
1.28427935068815));
#48088=CARTESIAN_POINT('Ctrl Pts',(-24.0978126690739,-4.07682073202661,
-0.0011986260069221));
#48089=CARTESIAN_POINT('Ctrl Pts',(-25.3021873309261,-4.07710011149971,
-0.000698316132069399));
#48090=CARTESIAN_POINT('Ctrl Pts',(-25.2999890548301,-4.0771883891112,-0.0380112202494885));
#48091=CARTESIAN_POINT('Ctrl Pts',(-25.2182448903609,-4.05979569108433,
-1.42542869581234));
#48092=CARTESIAN_POINT('Ctrl Pts',(-25.0569548375188,-2.48999755919744,
-4.12052561435965));
#48093=CARTESIAN_POINT('Ctrl Pts',(-24.8183171723996,2.12023594681246,-4.32243201928095));
#48094=CARTESIAN_POINT('Ctrl Pts',(-24.5796795072803,4.78255033466597,-0.553201127887688));
#48095=CARTESIAN_POINT('Ctrl Pts',(-24.3410418421611,3.05100401366679,3.72427088853368));
#48096=CARTESIAN_POINT('Ctrl Pts',(-24.1024041770419,-1.48358370303888,
4.58015267461461));
#48097=CARTESIAN_POINT('Ctrl Pts',(-23.9227860066302,-3.87077237514414,
2.05714104990295));
#48098=CARTESIAN_POINT('Ctrl Pts',(-23.8227137245916,-4.07262966323526,
0.353848130340812));
#48099=CARTESIAN_POINT('Ctrl Pts',(-23.8021873309261,-4.06947811712022,
0.00374200930701521));
#48100=CARTESIAN_POINT('Origin',(-32.3478126690739,0.,0.));
#48101=CARTESIAN_POINT('',(-27.0978126690739,-4.06530890290629,0.00247015883041497));
#48102=CARTESIAN_POINT('',(-26.8021873309261,-4.0673676331488,-0.00339676908166275));
#48103=CARTESIAN_POINT('',(-32.3478126690739,-4.0705,-4.82875428449296E-13));
#48104=CARTESIAN_POINT('Ctrl Pts',(-27.0978126690739,-4.06530890290629,
0.0024701588304149));
#48105=CARTESIAN_POINT('Ctrl Pts',(-27.0485370072788,-4.06065548839014,
-0.840166902292313));
#48106=CARTESIAN_POINT('Ctrl Pts',(-26.9197154571106,-3.39394710335117,
-3.04982355875152));
#48107=CARTESIAN_POINT('Ctrl Pts',(-26.7113480185693,0.231122040344854,
-4.80889290141546));
#48108=CARTESIAN_POINT('Ctrl Pts',(-26.4727103534501,4.17045404914302,-2.40542998080026));
#48109=CARTESIAN_POINT('Ctrl Pts',(-26.2340726883308,4.27828796113812,2.20795949931288));
#48110=CARTESIAN_POINT('Ctrl Pts',(-25.9954350232116,0.45553419918425,4.79284005902739));
#48111=CARTESIAN_POINT('Ctrl Pts',(-25.7833483501259,-3.31384212136007,
3.1767246763176));
#48112=CARTESIAN_POINT('Ctrl Pts',(-25.6508075654134,-4.06012276262123,
0.902312619466092));
#48113=CARTESIAN_POINT('Ctrl Pts',(-25.5978126690739,-4.06667116509479,
-0.00316860155561056));
#48114=CARTESIAN_POINT('Ctrl Pts',(-26.8021873309261,-4.0673676331488,-0.00339676908166248));
#48115=CARTESIAN_POINT('Ctrl Pts',(-26.7772643850685,-4.07070764203952,
-0.429051031665485));
#48116=CARTESIAN_POINT('Ctrl Pts',(-26.6727955508379,-3.81302358814286,
-2.20931218578228));
#48117=CARTESIAN_POINT('Ctrl Pts',(-26.4887808282342,-1.22840035655279,
-4.65508935177024));
#48118=CARTESIAN_POINT('Ctrl Pts',(-26.2501431631149,3.25200474977257,-3.55010962682765));
#48119=CARTESIAN_POINT('Ctrl Pts',(-26.0115054979957,4.74470515142096,0.816452129912828));
#48120=CARTESIAN_POINT('Ctrl Pts',(-25.7728678328764,1.87831343359306,4.43291758398628));
#48121=CARTESIAN_POINT('Ctrl Pts',(-25.5364284438533,-2.67143520246076,
3.98094140217226));
#48122=CARTESIAN_POINT('Ctrl Pts',(-25.3795349432031,-4.07399401282602,
1.31217773515604));
#48123=CARTESIAN_POINT('Ctrl Pts',(-25.3021873309261,-4.07710011149971,
-0.000698316132069399));
#48124=CARTESIAN_POINT('Origin',(-32.3478126690739,0.,0.));
#48125=CARTESIAN_POINT('',(-28.5978126690739,-4.07533558288693,0.00197868943318482));
#48126=CARTESIAN_POINT('',(-28.3021873309261,-4.06480101368718,0.00206955444756823));
#48127=CARTESIAN_POINT('',(-32.3478126690739,-4.0705,-4.82875428449296E-13));
#48128=CARTESIAN_POINT('Ctrl Pts',(-28.5978126690739,-4.07533558288693,
0.00197868943318465));
#48129=CARTESIAN_POINT('Ctrl Pts',(-28.5258123375172,-4.0671548117311,-1.22130223361166));
#48130=CARTESIAN_POINT('Ctrl Pts',(-28.3742661175874,-2.83137270070474,
-3.80928172890928));
#48131=CARTESIAN_POINT('Ctrl Pts',(-28.1431740092847,1.57677629758835,-4.54925739906848));
#48132=CARTESIAN_POINT('Ctrl Pts',(-27.9045363441654,4.67899334175034,-1.13307817052668));
#48133=CARTESIAN_POINT('Ctrl Pts',(-27.6658986790463,3.48313507021902,3.32368060727122));
#48134=CARTESIAN_POINT('Ctrl Pts',(-27.4272610139269,-0.913111142894123,
4.72709634916456));
#48135=CARTESIAN_POINT('Ctrl Pts',(-27.2378990106029,-3.7357712242627,2.39447925508501));
#48136=CARTESIAN_POINT('Ctrl Pts',(-27.1280828956518,-4.06816751315389,
0.520105312452931));
#48137=CARTESIAN_POINT('Ctrl Pts',(-27.0978126690739,-4.06530890290629,
0.0024701588304149));
#48138=CARTESIAN_POINT('Ctrl Pts',(-28.3021873309261,-4.06480101368718,
0.00206955444756761));
#48139=CARTESIAN_POINT('Ctrl Pts',(-28.254539715307,-4.06101200920254,-0.812950610202758));
#48140=CARTESIAN_POINT('Ctrl Pts',(-28.1273462113148,-3.42764719991074,
-2.99402214660032));
#48141=CARTESIAN_POINT('Ctrl Pts',(-27.9206068189495,0.132734120902733,
-4.81264906024345));
#48142=CARTESIAN_POINT('Ctrl Pts',(-27.6819691538303,4.12035340306242,-2.4902241816421));
#48143=CARTESIAN_POINT('Ctrl Pts',(-27.4433314887111,4.32257108085691,2.11996606838733));
#48144=CARTESIAN_POINT('Ctrl Pts',(-27.2046938235918,0.55348171480276,4.78252270942354));
#48145=CARTESIAN_POINT('Ctrl Pts',(-26.9909791043302,-3.27734231397027,
3.2320385418624));
#48146=CARTESIAN_POINT('Ctrl Pts',(-26.8568102734416,-4.06004742651346,
0.929498100146529));
#48147=CARTESIAN_POINT('Ctrl Pts',(-26.8021873309261,-4.0673676331488,-0.00339676908166248));
#48148=CARTESIAN_POINT('Ctrl Pts',(-30.0683458050225,-1.79217368492187,
3.65473442716069));
#48149=CARTESIAN_POINT('Ctrl Pts',(-30.028572860836,-2.40105433738203,3.3561573610714));
#48150=CARTESIAN_POINT('Ctrl Pts',(-29.9490269724629,-3.45744192369399,
2.44891896771775));
#48151=CARTESIAN_POINT('Ctrl Pts',(-29.7899351957168,-4.48692818459232,
-0.165939112378094));
#48152=CARTESIAN_POINT('Ctrl Pts',(-29.5910704747841,-3.05580029857719,
-3.71995065683383));
#48153=CARTESIAN_POINT('Ctrl Pts',(-29.3524328096649,1.48524338711596,-4.58231611323432));
#48154=CARTESIAN_POINT('Ctrl Pts',(-29.1137951445456,4.65387018191312,-1.22765401651987));
#48155=CARTESIAN_POINT('Ctrl Pts',(-28.8751574794264,3.55090078994383,3.25125842872222));
#48156=CARTESIAN_POINT('Ctrl Pts',(-28.6365198143072,-0.816478135197904,
4.74503193420896));
#48157=CARTESIAN_POINT('Ctrl Pts',(-28.3978821491879,-4.4326431471991,1.8784345171529));
#48158=CARTESIAN_POINT('Ctrl Pts',(-28.1592444840687,-3.97698621643786,
-2.71342222480818));
#48159=CARTESIAN_POINT('Ctrl Pts',(-27.9206068189495,0.132734120902733,
-4.81264906024345));
#48160=CARTESIAN_POINT('Ctrl Pts',(-27.6819691538303,4.12035340306242,-2.4902241816421));
#48161=CARTESIAN_POINT('Ctrl Pts',(-27.4433314887111,4.32257108085691,2.11996606838733));
#48162=CARTESIAN_POINT('Ctrl Pts',(-27.2046938235918,0.55348171480276,4.78252270942354));
#48163=CARTESIAN_POINT('Ctrl Pts',(-26.9660561584726,-3.72408468243647,
3.05122444962453));
#48164=CARTESIAN_POINT('Ctrl Pts',(-26.7274184933533,-4.58024332037796,
-1.48330752890949));
#48165=CARTESIAN_POINT('Ctrl Pts',(-26.4887808282342,-1.22840035655279,
-4.65508935177024));
#48166=CARTESIAN_POINT('Ctrl Pts',(-26.2501431631149,3.25200474977257,-3.55010962682765));
#48167=CARTESIAN_POINT('Ctrl Pts',(-26.0115054979957,4.74470515142096,0.816452129912828));
#48168=CARTESIAN_POINT('Ctrl Pts',(-25.7728678328764,1.87831343359306,4.43291758398628));
#48169=CARTESIAN_POINT('Ctrl Pts',(-25.5342301677573,-2.71373612241715,
3.97673919017804));
#48170=CARTESIAN_POINT('Ctrl Pts',(-25.295592502638,-4.81260180106317,-0.132978803016981));
#48171=CARTESIAN_POINT('Ctrl Pts',(-25.0569548375188,-2.48999755919744,
-4.12052561435965));
#48172=CARTESIAN_POINT('Ctrl Pts',(-24.8183171723996,2.12023594681246,-4.32243201928095));
#48173=CARTESIAN_POINT('Ctrl Pts',(-24.5796795072803,4.78255033466597,-0.553201127887688));
#48174=CARTESIAN_POINT('Ctrl Pts',(-24.3410418421611,3.05100401366679,3.72427088853368));
#48175=CARTESIAN_POINT('Ctrl Pts',(-24.1024041770419,-1.48358370303888,
4.58015267461461));
#48176=CARTESIAN_POINT('Ctrl Pts',(-23.8637665119226,-4.65516222209766,
1.22812207654118));
#48177=CARTESIAN_POINT('Ctrl Pts',(-23.6251288468034,-3.54991501369184,
-3.25221809482192));
#48178=CARTESIAN_POINT('Ctrl Pts',(-23.3864911816842,0.816736872430108,
-4.74465594332464));
#48179=CARTESIAN_POINT('Ctrl Pts',(-23.1478535165649,4.43303010358293,-1.87804772118901));
#48180=CARTESIAN_POINT('Ctrl Pts',(-22.9092158514458,3.97657650355884,2.71397465949093));
#48181=CARTESIAN_POINT('Ctrl Pts',(-22.6705781863265,-0.13326743518637,
4.81259378419344));
#48182=CARTESIAN_POINT('Ctrl Pts',(-22.4319405212073,-4.12067491146169,
2.48975047251535));
#48183=CARTESIAN_POINT('Ctrl Pts',(-22.1933028560881,-4.32230487333938,
-2.12049515987218));
#48184=CARTESIAN_POINT('Ctrl Pts',(-21.9546651909688,-0.552914322524486,
-4.78258349567352));
#48185=CARTESIAN_POINT('Ctrl Pts',(-21.7160275258496,3.72445384229878,-3.05078067349642));
#48186=CARTESIAN_POINT('Ctrl Pts',(-21.4773898607304,4.58006369995296,1.4838583643783));
#48187=CARTESIAN_POINT('Ctrl Pts',(-21.2387521956112,1.22784291284316,4.65523586110807));
#48188=CARTESIAN_POINT('Ctrl Pts',(-21.0001145304919,-3.25243097005294,
3.54971997856348));
#48189=CARTESIAN_POINT('Ctrl Pts',(-20.7614768653727,-4.74460695685984,
-0.817021398792471));
#48190=CARTESIAN_POINT('Ctrl Pts',(-20.5228392002535,-1.87778187766528,
-4.43314271832978));
#48191=CARTESIAN_POINT('Ctrl Pts',(-20.2842015351343,2.71421312200688,-3.97641374475733));
#48192=CARTESIAN_POINT('Ctrl Pts',(-20.045563870015,4.81258578377826,0.133556036718511));
#48193=CARTESIAN_POINT('Ctrl Pts',(-19.8069262048958,2.48950335928912,4.12082420945821));
#48194=CARTESIAN_POINT('Ctrl Pts',(-19.5682885397766,-2.12075435614108,
4.32217770366716));
#48195=CARTESIAN_POINT('Ctrl Pts',(-19.3296508746574,-4.7826166442574,0.552627519438542));
#48196=CARTESIAN_POINT('Ctrl Pts',(-19.0910132095381,-3.05055731986689,
-3.72463678489262));
#48197=CARTESIAN_POINT('Ctrl Pts',(-18.8523755444189,1.48413301908516,-4.57997470766269));
#48198=CARTESIAN_POINT('Ctrl Pts',(-18.6137378792997,4.6553094840529,-1.22756374533297));
#48199=CARTESIAN_POINT('Ctrl Pts',(-18.3751002141804,3.54952493031783,3.25264383390203));
#48200=CARTESIAN_POINT('Ctrl Pts',(-18.1364625490612,-0.817305922033317,
4.74455795316888));
#48201=CARTESIAN_POINT('Ctrl Pts',(-17.897824883942,-4.43325531722986,1.87751602747407));
#48202=CARTESIAN_POINT('Ctrl Pts',(-17.6591872188228,-3.97625097160617,
-2.71445157480656));
#48203=CARTESIAN_POINT('Ctrl Pts',(-17.4205495537035,0.133844637744424,
-4.81257776603306));
#48204=CARTESIAN_POINT('Ctrl Pts',(-17.1819118885843,4.1209734926491,-2.4892562371223));
#48205=CARTESIAN_POINT('Ctrl Pts',(-16.9432742234651,4.32205051844462,2.12101354478971));
#48206=CARTESIAN_POINT('Ctrl Pts',(-16.7046365583459,0.55234071436891,4.78264977563894));
#48207=CARTESIAN_POINT('Ctrl Pts',(-16.4659988932266,-3.72481971409399,
3.05033395526876));
#48208=CARTESIAN_POINT('Ctrl Pts',(-16.2273612281074,-4.57988569890107,
-1.48440766845576));
#48209=CARTESIAN_POINT('Ctrl Pts',(-15.9887235629882,-1.22728457340874,
-4.65538309025602));
#48210=CARTESIAN_POINT('Ctrl Pts',(-15.7500858978689,3.25285668605437,-3.54932986930775));
#48211=CARTESIAN_POINT('Ctrl Pts',(-15.5114482327497,4.74450893241555,0.817590442335157));
#48212=CARTESIAN_POINT('Ctrl Pts',(-15.2728105676305,1.8772501705311,4.43336790018713));
#48213=CARTESIAN_POINT('Ctrl Pts',(-15.0341729025113,-2.71469001784463,
3.97608818415582));
#48214=CARTESIAN_POINT('Ctrl Pts',(-14.795535237392,-4.81256973098103,-0.134133238289019));
#48215=CARTESIAN_POINT('Ctrl Pts',(-14.5568975722728,-2.48900910600372,
-4.12112276102026));
#48216=CARTESIAN_POINT('Ctrl Pts',(-14.3182599071536,2.12127272581082,-4.32192331767929));
#48217=CARTESIAN_POINT('Ctrl Pts',(-14.0796222420344,4.78268288982128,-0.552053907312987));
#48218=CARTESIAN_POINT('Ctrl Pts',(-13.8409845769151,3.05011057970114,3.72500262990027));
#48219=CARTESIAN_POINT('Ctrl Pts',(-13.6023469117959,-1.48468231248816,
4.57979667366944));
#48220=CARTESIAN_POINT('Ctrl Pts',(-13.3637092466767,-4.65545667971761,
1.22700539707102));
#48221=CARTESIAN_POINT('Ctrl Pts',(-13.1250715815574,-3.5491347955337,-3.25306952650887));
#48222=CARTESIAN_POINT('Ctrl Pts',(-12.8864339164382,0.817874959696777,
-4.74445989460021));
#48223=CARTESIAN_POINT('Ctrl Pts',(-12.647796251319,4.43348046720131,-1.87698430683722));
#48224=CARTESIAN_POINT('Ctrl Pts',(-12.4091585861998,3.9759253824068,2.71492845112022));
#48225=CARTESIAN_POINT('Ctrl Pts',(-12.1705209210805,-0.134421838351238,
4.81256167862222));
#48226=CARTESIAN_POINT('Ctrl Pts',(-11.9318832559613,-4.12127201457121,
2.48876196593426));
#48227=CARTESIAN_POINT('Ctrl Pts',(-11.6932455908421,-4.32179610137161,
-2.12153189920346));
#48228=CARTESIAN_POINT('Ctrl Pts',(-11.4546079257229,-0.551767098271795,
-4.78271598680431));
#48229=CARTESIAN_POINT('Ctrl Pts',(-11.2159702606036,3.72518553231084,-3.04988719316482));
#48230=CARTESIAN_POINT('Ctrl Pts',(-10.9773325954844,4.57970763196809,1.48495695118139));
#48231=CARTESIAN_POINT('Ctrl Pts',(-10.7386949303652,1.22672621632081,4.65553025243742));
#48232=CARTESIAN_POINT('Ctrl Pts',(-10.500057265246,-3.25328235526483,3.54893970899639));
#48233=CARTESIAN_POINT('Ctrl Pts',(-10.2614196001267,-4.74441083972299,
-0.81815947411722));
#48234=CARTESIAN_POINT('Ctrl Pts',(-10.0227819350075,-1.8767184363934,-4.43359301827195));
#48235=CARTESIAN_POINT('Ctrl Pts',(-9.78414426988828,2.71516687463254,-3.97576256635973));
#48236=CARTESIAN_POINT('Ctrl Pts',(-9.54550660476906,4.8125536089566,0.134710437930172));
#48237=CARTESIAN_POINT('Ctrl Pts',(-9.30686893964983,2.48851481691486,4.12142125330121));
#48238=CARTESIAN_POINT('Ctrl Pts',(-9.06823127453061,-2.12179106496689,
4.32166886952238));
#48239=CARTESIAN_POINT('Ctrl Pts',(-8.82959360941138,-4.78274906658767,
0.551480287245675));
#48240=CARTESIAN_POINT('Ctrl Pts',(-8.59095594429215,-3.04966379566106,
-3.72536842132379));
#48241=CARTESIAN_POINT('Ctrl Pts',(-8.35231827917293,1.48523158453539,-4.57961857379977));
#48242=CARTESIAN_POINT('Ctrl Pts',(-8.1136806140537,4.65560380841346,-1.22644703115444));
#48243=CARTESIAN_POINT('Ctrl Pts',(-7.87504294893448,3.54874460969979,3.25349517231261));
#48244=CARTESIAN_POINT('Ctrl Pts',(-7.63640528381524,-0.818443985601727,
4.74436176780107));
#48245=CARTESIAN_POINT('Ctrl Pts',(-7.39776761869602,-4.43370555338651,
1.87645255916802));
#48246=CARTESIAN_POINT('Ctrl Pts',(-7.1591299535768,-3.97559973603849,-2.71540528831811));
#48247=CARTESIAN_POINT('Ctrl Pts',(-6.92049228845756,0.134999037069343,
-4.81254552210429));
#48248=CARTESIAN_POINT('Ctrl Pts',(-6.68185462333835,4.1215704771241,-2.48826765871595));
#48249=CARTESIAN_POINT('Ctrl Pts',(-6.44321695821911,4.32154162229638,2.12205022265777));
#48250=CARTESIAN_POINT('Ctrl Pts',(-6.20457929309988,0.551193473920355,
4.78278213002022));
#48251=CARTESIAN_POINT('Ctrl Pts',(-5.96594162798067,-3.72555129633323,
3.04944038556121));
#48252=CARTESIAN_POINT('Ctrl Pts',(-5.72730396286143,-4.57952950032639,
-1.48550620942175));
#48253=CARTESIAN_POINT('Ctrl Pts',(-5.48866629774222,-1.22616783934351,
-4.65567735364785));
#48254=CARTESIAN_POINT('Ctrl Pts',(-5.25002863262297,3.25370797337249,-3.54854948612432));
#48255=CARTESIAN_POINT('Ctrl Pts',(-5.01139096750376,4.74431268704714,0.818728472038551));
#48256=CARTESIAN_POINT('Ctrl Pts',(-4.77275330238453,1.87618665939981,4.43381811498155));
#48257=CARTESIAN_POINT('Ctrl Pts',(-4.5341156372653,-2.71564366192391,3.97543680999486));
#48258=CARTESIAN_POINT('Ctrl Pts',(-4.29547797214608,-4.812537476128,-0.135287479444116));
#48259=CARTESIAN_POINT('Ctrl Pts',(-4.05684030702684,-2.48802037989938,
-4.12171998606955));
#48260=CARTESIAN_POINT('Ctrl Pts',(-3.81820264190762,2.12230915839156,-4.32141378384957));
#48261=CARTESIAN_POINT('Ctrl Pts',(-3.5795649767884,4.78281558760628,-0.550907763508576));
#48262=CARTESIAN_POINT('Ctrl Pts',(-3.34092731166917,3.04921617498962,3.72573627855867));
#48263=CARTESIAN_POINT('Ctrl Pts',(-3.10228964654994,-1.48577931367711,
4.57943634031457));
#48264=CARTESIAN_POINT('Ctrl Pts',(-2.86365198143072,-4.65575379041631,
1.22589645476151));
#48265=CARTESIAN_POINT('Ctrl Pts',(-2.62501431631149,-3.54834876796527,
-3.25393575552032));
#48266=CARTESIAN_POINT('Ctrl Pts',(-2.38637665119226,0.819002242401078,
-4.74423481374027));
#48267=CARTESIAN_POINT('Ctrl Pts',(-2.14773898607304,4.43395122223712,-1.87597598138563));
#48268=CARTESIAN_POINT('Ctrl Pts',(-1.90910132095381,3.97523440584382,2.71598802545506));
#48269=CARTESIAN_POINT('Ctrl Pts',(-1.67046365583458,-0.135500177452599,
4.81232596646912));
#48270=CARTESIAN_POINT('Ctrl Pts',(-1.43182599071536,-4.12201486774593,
2.48816358626208));
#48271=CARTESIAN_POINT('Ctrl Pts',(-1.19318832559613,-4.32100676816269,
-2.12331775762679));
#48272=CARTESIAN_POINT('Ctrl Pts',(-0.9545506604769,-0.551158953576692,
-4.78140835552346));
#48273=CARTESIAN_POINT('Ctrl Pts',(-0.715912995357679,3.72696190987269,
-3.05177387808086));
#48274=CARTESIAN_POINT('Ctrl Pts',(-0.477275330238447,4.57725222884596,
1.49154630755727));
#48275=CARTESIAN_POINT('Ctrl Pts',(-0.278410609305757,1.78830202401348,
4.11849926473408));
#48276=CARTESIAN_POINT('Ctrl Pts',(-0.119318832559607,-1.02190788268887,
4.1117895186236));
#48277=CARTESIAN_POINT('Ctrl Pts',(-0.0397729441865359,-2.25151393523441,
3.45825666525491));
#48278=CARTESIAN_POINT('Ctrl Pts',(0.,-2.75129702511903,2.99988915288068));
#48279=CARTESIAN_POINT('Ctrl Pts',(-29.9038972033484,-1.91758108071807,
3.91047455474608));
#48280=CARTESIAN_POINT('Ctrl Pts',(-29.8641242591618,-2.56906817116925,
3.59100455142768));
#48281=CARTESIAN_POINT('Ctrl Pts',(-29.7845783707887,-3.69937650370433,
2.62028213013966));
#48282=CARTESIAN_POINT('Ctrl Pts',(-29.6254865940426,-4.80090108994663,
-0.177550705673484));
#48283=CARTESIAN_POINT('Ctrl Pts',(-29.4266218731099,-3.26962999641403,
-3.98025429162597));
#48284=CARTESIAN_POINT('Ctrl Pts',(-29.1879842079907,1.58917332809701,-4.90296379114112));
#48285=CARTESIAN_POINT('Ctrl Pts',(-28.9493465428715,4.97952485746032,-1.31355913522901));
#48286=CARTESIAN_POINT('Ctrl Pts',(-28.7107088777522,3.79937515632038,3.47876531381764));
#48287=CARTESIAN_POINT('Ctrl Pts',(-28.472071212633,-0.873611211930994,
5.07706565551933));
#48288=CARTESIAN_POINT('Ctrl Pts',(-28.2334335475137,-4.74281745578375,
2.00987801671541));
#48289=CARTESIAN_POINT('Ctrl Pts',(-27.9947958823946,-4.25527592056482,
-2.90329400887223));
#48290=CARTESIAN_POINT('Ctrl Pts',(-27.7561582172753,0.142022194137876,
-5.14941429154002));
#48291=CARTESIAN_POINT('Ctrl Pts',(-27.5175205521561,4.40867522944874,-2.66447767738084));
#48292=CARTESIAN_POINT('Ctrl Pts',(-27.2788828870369,4.62504309400783,2.26831074393387));
#48293=CARTESIAN_POINT('Ctrl Pts',(-27.0402452219176,0.59221161082695,5.1171798486122));
#48294=CARTESIAN_POINT('Ctrl Pts',(-26.8016075567984,-3.98467759576748,
3.26473395232318));
#48295=CARTESIAN_POINT('Ctrl Pts',(-26.5629698916792,-4.90074595455584,
-1.58710200816697));
#48296=CARTESIAN_POINT('Ctrl Pts',(-26.3243322265599,-1.31435770042331,
-4.9808293387569));
#48297=CARTESIAN_POINT('Ctrl Pts',(-26.0856945614408,3.47956385870106,-3.79852863154653));
#48298=CARTESIAN_POINT('Ctrl Pts',(-25.8470568963215,5.07671600609805,0.873583386925484));
#48299=CARTESIAN_POINT('Ctrl Pts',(-25.6084192312023,2.00974846033062,4.74311109629157));
#48300=CARTESIAN_POINT('Ctrl Pts',(-25.3697815660831,-2.90362987147378,
4.25501160863666));
#48301=CARTESIAN_POINT('Ctrl Pts',(-25.1311439009638,-5.14936372539749,
-0.14228399788883));
#48302=CARTESIAN_POINT('Ctrl Pts',(-24.8925062358446,-2.66423519702527,
-4.40885949123555));
#48303=CARTESIAN_POINT('Ctrl Pts',(-24.6538685707254,2.26859950710815,-4.62489430159482));
#48304=CARTESIAN_POINT('Ctrl Pts',(-24.4152309056061,5.11720940693162,-0.591911389835893));
#48305=CARTESIAN_POINT('Ctrl Pts',(-24.1765932404869,3.26449809135411,3.98487683164073));
#48306=CARTESIAN_POINT('Ctrl Pts',(-23.9379555753677,-1.58739750758757,
4.90064896585306));
#48307=CARTESIAN_POINT('Ctrl Pts',(-23.6993179102485,-4.9809073081872,1.31405994776134));
#48308=CARTESIAN_POINT('Ctrl Pts',(-23.4606802451292,-3.79832040035196,
-3.47979213257527));
#48309=CARTESIAN_POINT('Ctrl Pts',(-23.22204258001,0.873888054307114,-5.07666335466403));
#48310=CARTESIAN_POINT('Ctrl Pts',(-22.9834049148908,4.74323148944965,-2.00946415469484));
#48311=CARTESIAN_POINT('Ctrl Pts',(-22.7447672497716,4.25483753801745,2.90388510018491));
#48312=CARTESIAN_POINT('Ctrl Pts',(-22.5061295846524,-0.142592827101065,
5.14935514754711));
#48313=CARTESIAN_POINT('Ctrl Pts',(-22.2674919195331,-4.40901923540582,
2.66397082044679));
#48314=CARTESIAN_POINT('Ctrl Pts',(-22.0288542544139,-4.624758258613,-2.26887685860782));
#48315=CARTESIAN_POINT('Ctrl Pts',(-21.7902165892947,-0.591604515260647,
-5.11724488838146));
#48316=CARTESIAN_POINT('Ctrl Pts',(-21.5515789241754,3.98507258759985,-3.26425912295005));
#48317=CARTESIAN_POINT('Ctrl Pts',(-21.3129412590562,4.90055376518737,1.58769138836067));
#48318=CARTESIAN_POINT('Ctrl Pts',(-21.074303593937,1.31376124957698,4.98098610008909));
#48319=CARTESIAN_POINT('Ctrl Pts',(-20.8356659288178,-3.4800199037556,3.7981117176359));
#48320=CARTESIAN_POINT('Ctrl Pts',(-20.5970282636985,-5.0766109403702,-0.874192490408381));
#48321=CARTESIAN_POINT('Ctrl Pts',(-20.3583905985793,-2.00917970876428,
-4.74335198441606));
#48322=CARTESIAN_POINT('Ctrl Pts',(-20.11975293346,2.90414024912104,-4.25466339016496));
#48323=CARTESIAN_POINT('Ctrl Pts',(-19.8811152683409,5.14934658730268,0.142901623532206));
#48324=CARTESIAN_POINT('Ctrl Pts',(-19.6424776032216,2.66370641546674,4.40917898053317));
#48325=CARTESIAN_POINT('Ctrl Pts',(-19.4038399381024,-2.26915419214175,
4.62462219023996));
#48326=CARTESIAN_POINT('Ctrl Pts',(-19.1652022729832,-5.11728035653827,
0.591297643122014));
#48327=CARTESIAN_POINT('Ctrl Pts',(-18.9265646078639,-3.26402014014505,
-3.985268331606));
#48328=CARTESIAN_POINT('Ctrl Pts',(-18.6879269427447,1.58798526203712,-4.90045854565949));
#48329=CARTESIAN_POINT('Ctrl Pts',(-18.4492892776255,4.98106487480121,-1.31346254731367));
#48330=CARTESIAN_POINT('Ctrl Pts',(-18.2106516125063,3.79790302088468,3.48024766275753));
#48331=CARTESIAN_POINT('Ctrl Pts',(-17.9720139473871,-0.874496923169711,
5.07655850764482));
#48332=CARTESIAN_POINT('Ctrl Pts',(-17.7333762822678,-4.74347246242682,
2.00889525569968));
#48333=CARTESIAN_POINT('Ctrl Pts',(-17.4947386171486,-4.25448922695873,
-2.90439538766098));
#48334=CARTESIAN_POINT('Ctrl Pts',(-17.2561009520293,0.143210419421708,
-5.14933800851558));
#48335=CARTESIAN_POINT('Ctrl Pts',(-17.0174632869101,4.40933870981885,-2.66344200092047));
#48336=CARTESIAN_POINT('Ctrl Pts',(-16.7788256217909,4.62448610522848,2.26943151752217));
#48337=CARTESIAN_POINT('Ctrl Pts',(-16.5401879566717,0.590990768860884,
5.11731580628902));
#48338=CARTESIAN_POINT('Ctrl Pts',(-16.3015502915524,-3.98546406128254,
3.2637811456039));
#48339=CARTESIAN_POINT('Ctrl Pts',(-16.0629126264332,-4.90036330850768,
-1.58827913000388));
#48340=CARTESIAN_POINT('Ctrl Pts',(-15.824274961314,-1.31316384032749,-4.98114363160013));
#48341=CARTESIAN_POINT('Ctrl Pts',(-15.5856372961948,3.48047540924424,-3.79769431047581));
#48342=CARTESIAN_POINT('Ctrl Pts',(-15.3469996310755,5.07650605666312,0.874801352786364));
#48343=CARTESIAN_POINT('Ctrl Pts',(-15.1083619659563,2.00861079541087,4.74359292337918));
#48344=CARTESIAN_POINT('Ctrl Pts',(-14.8697243008371,-2.90465051575626,
4.25431504845271));
#48345=CARTESIAN_POINT('Ctrl Pts',(-14.6310866357179,-5.1493294112106,-0.143519214796206));
#48346=CARTESIAN_POINT('Ctrl Pts',(-14.3924489705986,-2.66317757679605,
-4.4094984232478));
#48347=CARTESIAN_POINT('Ctrl Pts',(-14.1538113054794,2.26970883474132,-4.62435000358661));
#48348=CARTESIAN_POINT('Ctrl Pts',(-13.9151736403602,5.11735123763705,-0.590683892474468));
#48349=CARTESIAN_POINT('Ctrl Pts',(-13.676535975241,3.26354213932567,3.98565977662667));
#48350=CARTESIAN_POINT('Ctrl Pts',(-13.4378983101217,-1.58857299225892,
4.90026805373337));
#48351=CARTESIAN_POINT('Ctrl Pts',(-13.1992606450025,-4.98122237048603,
1.31286512861896));
#48352=CARTESIAN_POINT('Ctrl Pts',(-12.9606229798833,-3.79748558640983,
-3.48070314321456));
#48353=CARTESIAN_POINT('Ctrl Pts',(-12.7219853147641,0.87510577925706,-5.0764535874255));
#48354=CARTESIAN_POINT('Ctrl Pts',(-12.4833476496448,4.74371336727283,-2.00832632789875));
#48355=CARTESIAN_POINT('Ctrl Pts',(-12.2447099845256,4.25414085464746,2.90490563340592));
#48356=CARTESIAN_POINT('Ctrl Pts',(-12.0060723194064,-0.143828009654572,
5.14932079538778));
#48357=CARTESIAN_POINT('Ctrl Pts',(-11.7674346542871,-4.40965812081948,
2.66291314309442));
#48358=CARTESIAN_POINT('Ctrl Pts',(-11.5287969891679,-4.6242138853148,-2.26998614379823));
#48359=CARTESIAN_POINT('Ctrl Pts',(-11.2901593240487,-0.590377013963862,
-5.11738665058224));
#48360=CARTESIAN_POINT('Ctrl Pts',(-11.0515216589295,3.98585547763773,-3.26330312131122));
#48361=CARTESIAN_POINT('Ctrl Pts',(-10.8128839938102,4.90017278133687,1.58886684880117));
#48362=CARTESIAN_POINT('Ctrl Pts',(-10.574246328691,1.31256641218918,4.98130109145864));
#48363=CARTESIAN_POINT('Ctrl Pts',(-10.3356086635718,-3.48093086466773,
3.79727684868749));
#48364=CARTESIAN_POINT('Ctrl Pts',(-10.0969709984526,-5.07640109993208,
-0.875410202580779));
#48365=CARTESIAN_POINT('Ctrl Pts',(-9.85833333333333,-2.00804185316436,
-4.74383379410727));
#48366=CARTESIAN_POINT('Ctrl Pts',(-9.61969566821411,2.90516074060913,-4.25396664554368));
#48367=CARTESIAN_POINT('Ctrl Pts',(-9.38105800309488,5.14931216104712,0.14413680399584));
#48368=CARTESIAN_POINT('Ctrl Pts',(-9.14242033797565,2.66264869981656,4.40981780253313));
#48369=CARTESIAN_POINT('Ctrl Pts',(-8.90378267285642,-2.27026344469205,
4.62407775041392));
#48370=CARTESIAN_POINT('Ctrl Pts',(-8.6651450077372,-5.11742204512421,0.590070133329444));
#48371=CARTESIAN_POINT('Ctrl Pts',(-8.42650734261798,-3.26306409156187,
-3.98605116431367));
#48372=CARTESIAN_POINT('Ctrl Pts',(-8.18786967749874,1.58916069963059,-4.90007749132113));
#48373=CARTESIAN_POINT('Ctrl Pts',(-7.94923201237953,4.98137979451584,-1.31226769103422));
#48374=CARTESIAN_POINT('Ctrl Pts',(-7.71059434726029,3.79706809731301,3.48115857359343));
#48375=CARTESIAN_POINT('Ctrl Pts',(-7.47195668214107,-0.875714622763106,
5.07634859420128));
#48376=CARTESIAN_POINT('Ctrl Pts',(-7.23331901702185,-4.74395420386913,
2.00775737117387));
#48377=CARTESIAN_POINT('Ctrl Pts',(-6.99468135190261,-4.25379242116686,
-2.90541583729795));
#48378=CARTESIAN_POINT('Ctrl Pts',(-6.7560436867834,0.144445597866564,-5.14930350831713));
#48379=CARTESIAN_POINT('Ctrl Pts',(-6.51740602166415,4.40997746829655,-2.66238424671687));
#48380=CARTESIAN_POINT('Ctrl Pts',(-6.27876835654495,4.62394159906029,2.27054073694845));
#48381=CARTESIAN_POINT('Ctrl Pts',(-6.04013069142569,0.58976325023493,5.11745742217124));
#48382=CARTESIAN_POINT('Ctrl Pts',(-5.80149302630649,-3.9862468360062,3.26282504833503));
#48383=CARTESIAN_POINT('Ctrl Pts',(-5.56285536118725,-4.89998218492935,
-1.58945454139984));
#48384=CARTESIAN_POINT('Ctrl Pts',(-5.32421769606804,-1.31196896276975,
-4.98145848607974));
#48385=CARTESIAN_POINT('Ctrl Pts',(-5.08558003094879,3.48138626541249,-3.79685931996075));
#48386=CARTESIAN_POINT('Ctrl Pts',(-4.84694236582958,5.07629607902044,0.876019016145047));
#48387=CARTESIAN_POINT('Ctrl Pts',(-4.60830470071035,2.00747286506312,4.74407464196444));
#48388=CARTESIAN_POINT('Ctrl Pts',(-4.36966703559112,-2.90567089110244,
4.25361809436949));
#48389=CARTESIAN_POINT('Ctrl Pts',(-4.1310293704719,-5.14929489932346,-0.144754224003302));
#48390=CARTESIAN_POINT('Ctrl Pts',(-3.89239170535267,-2.66211966455929,
-4.41013743913397));
#48391=CARTESIAN_POINT('Ctrl Pts',(-3.65375404023344,2.27081779171631,-4.62380481511515));
#48392=CARTESIAN_POINT('Ctrl Pts',(-3.41511637511422,5.11749322095267,-0.589457547230361));
#48393=CARTESIAN_POINT('Ctrl Pts',(-3.17647870999498,3.26258514862341,3.98644476236722));
#48394=CARTESIAN_POINT('Ctrl Pts',(-2.93784104487577,-1.58974675613189,
4.89988250604351));
#48395=CARTESIAN_POINT('Ctrl Pts',(-2.69920337975654,-4.98154027151287,
1.31167858804524));
#48396=CARTESIAN_POINT('Ctrl Pts',(-2.46056571463731,-3.79664455654379,
-3.48162998662147));
#48397=CARTESIAN_POINT('Ctrl Pts',(-2.22192804951808,0.876311943595137,
-5.07621275652709));
#48398=CARTESIAN_POINT('Ctrl Pts',(-1.98329038439886,4.74421706340335,-2.00724744484995));
#48399=CARTESIAN_POINT('Ctrl Pts',(-1.74465271927963,4.25340152698323,2.90603935147979));
#48400=CARTESIAN_POINT('Ctrl Pts',(-1.5060150541604,-0.144981805559941,
5.14906858927122));
#48401=CARTESIAN_POINT('Ctrl Pts',(-1.26737738904118,-4.41045295516259,
2.66227289179059));
#48402=CARTESIAN_POINT('Ctrl Pts',(-1.02873972392195,-4.62336931849601,
-2.27189696770677));
#48403=CARTESIAN_POINT('Ctrl Pts',(-0.790102058802722,-0.589726314329404,
-5.11598751777173));
#48404=CARTESIAN_POINT('Ctrl Pts',(-0.551464393683503,3.98775615726128,
-3.26532182704867));
#48405=CARTESIAN_POINT('Ctrl Pts',(-0.312826728564268,4.89754556132347,
1.5959172955446));
#48406=CARTESIAN_POINT('Ctrl Pts',(-0.11396200763158,1.91343850024653,4.40669134774724));
#48407=CARTESIAN_POINT('Ctrl Pts',(0.0451297691145716,-1.09341591083915,
4.39951208699472));
#48408=CARTESIAN_POINT('Ctrl Pts',(0.124675657487642,-2.40906367586066,
3.7002482568252));
#48409=CARTESIAN_POINT('Ctrl Pts',(0.164448601674178,-2.94381909922654,
3.20980646698106));
#48410=CARTESIAN_POINT('Ctrl Pts',(-29.7394486016742,-2.04298847651428,
4.16621468233147));
#48411=CARTESIAN_POINT('Ctrl Pts',(-29.6996756574876,-2.73708200495646,
3.82585174178397));
#48412=CARTESIAN_POINT('Ctrl Pts',(-29.6201297691146,-3.94131108371467,
2.79164529256157));
#48413=CARTESIAN_POINT('Ctrl Pts',(-29.4610379923684,-5.11487399530094,
-0.189162298968872));
#48414=CARTESIAN_POINT('Ctrl Pts',(-29.2621732714358,-3.48345969425087,
-4.2405579264181));
#48415=CARTESIAN_POINT('Ctrl Pts',(-29.0235356063165,1.69310326907807,-5.22361146904792));
#48416=CARTESIAN_POINT('Ctrl Pts',(-28.7848979411973,5.30517953300752,-1.39946425393815));
#48417=CARTESIAN_POINT('Ctrl Pts',(-28.546260276078,4.04784952269694,3.70627219891307));
#48418=CARTESIAN_POINT('Ctrl Pts',(-28.3076226109588,-0.930744288664083,
5.4090993768297));
#48419=CARTESIAN_POINT('Ctrl Pts',(-28.0689849458396,-5.05299176436839,
2.14132151627792));
#48420=CARTESIAN_POINT('Ctrl Pts',(-27.8303472807204,-4.53356562469179,
-3.09316579293629));
#48421=CARTESIAN_POINT('Ctrl Pts',(-27.5917096156012,0.151310267373015,
-5.48617952283658));
#48422=CARTESIAN_POINT('Ctrl Pts',(-27.3530719504819,4.69699705583506,-2.83873117311958));
#48423=CARTESIAN_POINT('Ctrl Pts',(-27.1144342853627,4.92751510715875,2.4166554194804));
#48424=CARTESIAN_POINT('Ctrl Pts',(-26.8757966202434,0.630941506851146,
5.45183698780086));
#48425=CARTESIAN_POINT('Ctrl Pts',(-26.6371589551242,-4.2452705090985,3.47824345502183));
#48426=CARTESIAN_POINT('Ctrl Pts',(-26.398521290005,-5.22124858873371,-1.69089648742445));
#48427=CARTESIAN_POINT('Ctrl Pts',(-26.1598836248858,-1.40031504429382,
-5.30656932574355));
#48428=CARTESIAN_POINT('Ctrl Pts',(-25.9212459597666,3.70712296762955,-4.0469476362654));
#48429=CARTESIAN_POINT('Ctrl Pts',(-25.6826082946473,5.40872686077514,0.930714643938138));
#48430=CARTESIAN_POINT('Ctrl Pts',(-25.4439706295281,2.14118348706817,5.05330460859686));
#48431=CARTESIAN_POINT('Ctrl Pts',(-25.2053329644089,-3.09352362053041,
4.53328402709528));
#48432=CARTESIAN_POINT('Ctrl Pts',(-24.9666952992896,-5.4861256497318,-0.151589192760673));
#48433=CARTESIAN_POINT('Ctrl Pts',(-24.7280576341705,-2.8384728348531,-4.69719336811145));
#48434=CARTESIAN_POINT('Ctrl Pts',(-24.4894199690512,2.41696306740383,-4.92735658390869));
#48435=CARTESIAN_POINT('Ctrl Pts',(-24.250782303932,5.45186847919727,-0.6306216517841));
#48436=CARTESIAN_POINT('Ctrl Pts',(-24.0121446388127,3.47799216904142,4.24548277474778));
#48437=CARTESIAN_POINT('Ctrl Pts',(-23.7735069736936,-1.69121131213625,
5.22114525709151));
#48438=CARTESIAN_POINT('Ctrl Pts',(-23.5348693085742,-5.30665239427673,
1.39999781898149));
#48439=CARTESIAN_POINT('Ctrl Pts',(-23.2962316434551,-4.04672578701207,
-3.70736617032861));
#48440=CARTESIAN_POINT('Ctrl Pts',(-23.0575939783358,0.931039236184116,
-5.40867076600343));
#48441=CARTESIAN_POINT('Ctrl Pts',(-22.8189563132166,5.05343287531637,-2.14088058820066));
#48442=CARTESIAN_POINT('Ctrl Pts',(-22.5803186480974,4.53309857247606,3.09379554087889));
#48443=CARTESIAN_POINT('Ctrl Pts',(-22.3416809829782,-0.151918219015756,
5.48611651090078));
#48444=CARTESIAN_POINT('Ctrl Pts',(-22.1030433178589,-4.69736355934995,
2.83819116837823));
#48445=CARTESIAN_POINT('Ctrl Pts',(-21.8644056527397,-4.92721164388661,
-2.41725855734347));
#48446=CARTESIAN_POINT('Ctrl Pts',(-21.6257679876205,-0.630294707996812,
-5.45190628108939));
#48447=CARTESIAN_POINT('Ctrl Pts',(-21.3871303225012,4.24569133290092,-3.47773757240369));
#48448=CARTESIAN_POINT('Ctrl Pts',(-21.1484926573821,5.22104383042178,1.69152441234305));
#48449=CARTESIAN_POINT('Ctrl Pts',(-20.9098549922628,1.39967958631079,5.3067363390701));
#48450=CARTESIAN_POINT('Ctrl Pts',(-20.6712173271436,-3.70760883745824,
4.04650345670832));
#48451=CARTESIAN_POINT('Ctrl Pts',(-20.4325796620243,-5.40861492388057,
-0.931363582024293));
#48452=CARTESIAN_POINT('Ctrl Pts',(-20.1939419969051,-2.14057753986328,
-5.05356125050234));
#48453=CARTESIAN_POINT('Ctrl Pts',(-19.9553043317859,3.09406737623519,-4.5329130355726));
#48454=CARTESIAN_POINT('Ctrl Pts',(-19.7166666666667,5.48610739082711,0.152247210345901));
#48455=CARTESIAN_POINT('Ctrl Pts',(-19.4780290015475,2.83790947164436,4.69753375160813));
#48456=CARTESIAN_POINT('Ctrl Pts',(-19.2393913364282,-2.41755402814241,
4.92706667681276));
#48457=CARTESIAN_POINT('Ctrl Pts',(-19.000753671309,-5.45194406881915,0.62996776680549));
#48458=CARTESIAN_POINT('Ctrl Pts',(-18.7621160061898,-3.4774829604232,-4.24589987831939));
#48459=CARTESIAN_POINT('Ctrl Pts',(-18.5234783410705,1.69183750498908,-5.22094238365629));
#48460=CARTESIAN_POINT('Ctrl Pts',(-18.2848406759513,5.30682026554953,-1.39936134929439));
#48461=CARTESIAN_POINT('Ctrl Pts',(-18.0462030108321,4.04628111145152,3.70785149161303));
#48462=CARTESIAN_POINT('Ctrl Pts',(-17.8075653457129,-0.931687924306101,
5.40855906212076));
#48463=CARTESIAN_POINT('Ctrl Pts',(-17.5689276805936,-5.05368960762378,
2.14027448392529));
#48464=CARTESIAN_POINT('Ctrl Pts',(-17.3302900154744,-4.53272748231129,
-3.0943392005154));
#48465=CARTESIAN_POINT('Ctrl Pts',(-17.0916523503552,0.152576201098992,
-5.4860982509981));
#48466=CARTESIAN_POINT('Ctrl Pts',(-16.8530146852359,4.6977039269886,-2.83762776471865));
#48467=CARTESIAN_POINT('Ctrl Pts',(-16.6143770201167,4.92692169201234,2.41784949025462));
#48468=CARTESIAN_POINT('Ctrl Pts',(-16.3757393549975,0.62964082335285,5.45198183693909));
#48469=CARTESIAN_POINT('Ctrl Pts',(-16.1371016898783,-4.24610840847109,
3.47722833593904));
#48470=CARTESIAN_POINT('Ctrl Pts',(-15.898464024759,-5.2208409181143,-1.69215059155202));
#48471=CARTESIAN_POINT('Ctrl Pts',(-15.6598263596398,-1.39904310724623,
-5.30690417294424));
#48472=CARTESIAN_POINT('Ctrl Pts',(-15.4211886945206,3.70809413243411,-4.04605875164388));
#48473=CARTESIAN_POINT('Ctrl Pts',(-15.1825510294014,5.40850318091069,0.932012263237568));
#48474=CARTESIAN_POINT('Ctrl Pts',(-14.9439133642821,2.13997142029063,5.05381794657124));
#48475=CARTESIAN_POINT('Ctrl Pts',(-14.7052756991629,-3.09461101366789,
4.53254191274959));
#48476=CARTESIAN_POINT('Ctrl Pts',(-14.4666380340437,-5.48608909144016,
-0.152905191303383));
#48477=CARTESIAN_POINT('Ctrl Pts',(-14.2280003689245,-2.83734604758839,
-4.69787408547534));
#48478=CARTESIAN_POINT('Ctrl Pts',(-13.9893627038052,2.41814494367183,-4.92677668949392));
#48479=CARTESIAN_POINT('Ctrl Pts',(-13.750725038686,5.45201958545282,-0.629313877635948));
#48480=CARTESIAN_POINT('Ctrl Pts',(-13.5120873735668,3.47697369895021,4.24631692335307));
#48481=CARTESIAN_POINT('Ctrl Pts',(-13.2734497084476,-1.69246367202968,
5.2207394337973));
#48482=CARTESIAN_POINT('Ctrl Pts',(-13.0348120433283,-5.30698806125446,
1.3987248601669));
#48483=CARTESIAN_POINT('Ctrl Pts',(-12.7961743782091,-4.04583637728596,
-3.70833675992024));
#48484=CARTESIAN_POINT('Ctrl Pts',(-12.5575367130899,0.932336598817344,
-5.40844728025078));
#48485=CARTESIAN_POINT('Ctrl Pts',(-12.3188990479706,5.05394626734435,-2.13966834896028));
#48486=CARTESIAN_POINT('Ctrl Pts',(-12.0802613828514,4.53235632688813,3.09488281569163));
#48487=CARTESIAN_POINT('Ctrl Pts',(-11.8416237177322,-0.153234180957902,
5.48607991215335));
#48488=CARTESIAN_POINT('Ctrl Pts',(-11.602986052613,-4.69804422706777,2.83706432025457));
#48489=CARTESIAN_POINT('Ctrl Pts',(-11.3643483874937,-4.92663166925799,
-2.41844038839298));
#48490=CARTESIAN_POINT('Ctrl Pts',(-11.1257107223745,-0.628986929655938,
-5.45205731436018));
#48491=CARTESIAN_POINT('Ctrl Pts',(-10.8870730572553,4.24652542296462,-3.47671904945761));
#48492=CARTESIAN_POINT('Ctrl Pts',(-10.6484353921361,5.22063793070565,1.69277674642096));
#48493=CARTESIAN_POINT('Ctrl Pts',(-10.4097977270168,1.39840660805754,5.30707193047986));
#48494=CARTESIAN_POINT('Ctrl Pts',(-10.1711600618976,-3.70857937407062,
4.04561398837858));
#48495=CARTESIAN_POINT('Ctrl Pts',(-9.93252239677838,-5.40839136014118,
-0.93266093104433));
#48496=CARTESIAN_POINT('Ctrl Pts',(-9.69388473165915,-2.13936526993532,
-5.05407456994261));
#48497=CARTESIAN_POINT('Ctrl Pts',(-9.45524706653993,3.09515460658571,-4.53217072472762));
#48498=CARTESIAN_POINT('Ctrl Pts',(-9.21660940142069,5.48607071313765,0.153563170061505));
#48499=CARTESIAN_POINT('Ctrl Pts',(-8.97797173630149,2.83678258271826,4.69821435176505));
#48500=CARTESIAN_POINT('Ctrl Pts',(-8.73933407118223,-2.41873582441721,
4.92648663130547));
#48501=CARTESIAN_POINT('Ctrl Pts',(-8.50069640606304,-5.45209502366077,
0.628659979413207));
#48502=CARTESIAN_POINT('Ctrl Pts',(-8.26205874094379,-3.47646438746268,
-4.24673390730354));
#48503=CARTESIAN_POINT('Ctrl Pts',(-8.02342107582457,1.69308981472579,-5.22053640884249));
#48504=CARTESIAN_POINT('Ctrl Pts',(-7.78478341070535,5.30715578061822,-1.398088350914));
#48505=CARTESIAN_POINT('Ctrl Pts',(-7.54614574558612,4.04539158492623,3.70882197487425));
#48506=CARTESIAN_POINT('Ctrl Pts',(-7.30750808046689,-0.932985259924489,
5.40833542060147));
#48507=CARTESIAN_POINT('Ctrl Pts',(-7.06887041534766,-5.05420285435175,
2.13906218317974));
#48508=CARTESIAN_POINT('Ctrl Pts',(-6.83023275022844,-4.53198510629524,
-3.09542638627781));
#48509=CARTESIAN_POINT('Ctrl Pts',(-6.5915950851092,0.153892158663785,-5.48606149452997));
#48510=CARTESIAN_POINT('Ctrl Pts',(-6.35295741998999,4.69838445946899,-2.83650083471779));
#48511=CARTESIAN_POINT('Ctrl Pts',(-6.11431975487076,4.92634157582419,2.41903125123913));
#48512=CARTESIAN_POINT('Ctrl Pts',(-5.87568208975152,0.628333026549508,
5.45213271432227));
#48513=CARTESIAN_POINT('Ctrl Pts',(-5.63704442463231,-4.24694237567916,
3.47620971110884));
#48514=CARTESIAN_POINT('Ctrl Pts',(-5.39840675951308,-5.22043486953231,
-1.69340287337793));
#48515=CARTESIAN_POINT('Ctrl Pts',(-5.15976909439385,-1.39777008619599,
-5.30723961851162));
#48516=CARTESIAN_POINT('Ctrl Pts',(-4.92113142927462,3.70906455745249,-4.04516915379718));
#48517=CARTESIAN_POINT('Ctrl Pts',(-4.6824937641554,5.40827947099373,0.933309560251545));
#48518=CARTESIAN_POINT('Ctrl Pts',(-4.44385609903617,2.13875907072644,5.05433116894732));
#48519=CARTESIAN_POINT('Ctrl Pts',(-4.20521843391694,-3.09569812028096,
4.53179937874414));
#48520=CARTESIAN_POINT('Ctrl Pts',(-3.96658076879772,-5.48605232251892,
-0.154220968562498));
#48521=CARTESIAN_POINT('Ctrl Pts',(-3.72794310367849,-2.83621894921919,
-4.69855489219838));
#48522=CARTESIAN_POINT('Ctrl Pts',(-3.48930543855926,2.41932642504106,-4.92619584638074));
#48523=CARTESIAN_POINT('Ctrl Pts',(-3.25066777344004,5.45217085429907,-0.62800733095214));
#48524=CARTESIAN_POINT('Ctrl Pts',(-3.01203010832081,3.47595412225719,4.24715324617577));
#48525=CARTESIAN_POINT('Ctrl Pts',(-2.77339244320158,-1.69371419858668,
5.22032867177245));
#48526=CARTESIAN_POINT('Ctrl Pts',(-2.53475477808237,-5.30732675260943,
1.39746072132896));
#48527=CARTESIAN_POINT('Ctrl Pts',(-2.29611711296313,-4.04494034512231,
-3.70932421772263));
#48528=CARTESIAN_POINT('Ctrl Pts',(-2.05747944784391,0.933621644789192,
-5.40819069931389));
#48529=CARTESIAN_POINT('Ctrl Pts',(-1.81884178272468,5.05448290456958,-2.13851890831426));
#48530=CARTESIAN_POINT('Ctrl Pts',(-1.58020411760545,4.53156864812263,3.09609067750451));
#48531=CARTESIAN_POINT('Ctrl Pts',(-1.34156645248623,-0.154463433667277,
5.48581121207333));
#48532=CARTESIAN_POINT('Ctrl Pts',(-1.102928787367,-4.69889104257927,2.83638219731909));
#48533=CARTESIAN_POINT('Ctrl Pts',(-0.86429112224777,-4.92573186882932,
-2.42047617778675));
#48534=CARTESIAN_POINT('Ctrl Pts',(-0.625653457128544,-0.628293675082119,
-5.45056668002));
#48535=CARTESIAN_POINT('Ctrl Pts',(-0.387015792009324,4.24855040464988,
-3.47886977601648));
#48536=CARTESIAN_POINT('Ctrl Pts',(-0.14837812689009,5.21783889380097,1.70028828353193));
#48537=CARTESIAN_POINT('Ctrl Pts',(0.0504865940425981,2.03857497647958,
4.69488343076037));
#48538=CARTESIAN_POINT('Ctrl Pts',(0.209578370788749,-1.16492393898944,
4.68723465536585));
#48539=CARTESIAN_POINT('Ctrl Pts',(0.28912425916182,-2.56661341648691,3.94223984839548));
#48540=CARTESIAN_POINT('Ctrl Pts',(0.328897203348356,-3.13634117333406,
3.41972378108145));
#48541=CARTESIAN_POINT('Ctrl Pts',(-29.575,-2.16839587231048,4.42195480991686));
#48542=CARTESIAN_POINT('Ctrl Pts',(-29.5352270558135,-2.90509583874368,
4.06069893214025));
#48543=CARTESIAN_POINT('Ctrl Pts',(-29.4556811674404,-4.18324566372502,
2.96300845498348));
#48544=CARTESIAN_POINT('Ctrl Pts',(-29.2965893906942,-5.42884690065524,
-0.200773892264263));
#48545=CARTESIAN_POINT('Ctrl Pts',(-29.0977246697616,-3.69728939208772,
-4.50086156121024));
#48546=CARTESIAN_POINT('Ctrl Pts',(-28.8590870046423,1.79703321005912,-5.54425914695472));
#48547=CARTESIAN_POINT('Ctrl Pts',(-28.6204493395231,5.63083420855472,-1.48536937264729));
#48548=CARTESIAN_POINT('Ctrl Pts',(-28.3818116744038,4.2963238890735,3.93377908400849));
#48549=CARTESIAN_POINT('Ctrl Pts',(-28.1431740092847,-0.987877365397176,
5.74113309814008));
#48550=CARTESIAN_POINT('Ctrl Pts',(-27.9045363441654,-5.36316607295304,
2.27276501584044));
#48551=CARTESIAN_POINT('Ctrl Pts',(-27.6658986790462,-4.81185532881875,
-3.28303757700034));
#48552=CARTESIAN_POINT('Ctrl Pts',(-27.4272610139269,0.160598340608156,
-5.82294475413315));
#48553=CARTESIAN_POINT('Ctrl Pts',(-27.1886233488077,4.98531888222138,-3.01298466885832));
#48554=CARTESIAN_POINT('Ctrl Pts',(-26.9499856836885,5.22998712030967,2.56500009502694));
#48555=CARTESIAN_POINT('Ctrl Pts',(-26.7113480185693,0.669671402875337,
5.78649412698952));
#48556=CARTESIAN_POINT('Ctrl Pts',(-26.4727103534501,-4.50586342242951,
3.69175295772048));
#48557=CARTESIAN_POINT('Ctrl Pts',(-26.2340726883308,-5.54175122291158,
-1.79469096668193));
#48558=CARTESIAN_POINT('Ctrl Pts',(-25.9954350232117,-1.48627238816434,
-5.6323093127302));
#48559=CARTESIAN_POINT('Ctrl Pts',(-25.7567973580923,3.93468207655805,-4.29536664098428));
#48560=CARTESIAN_POINT('Ctrl Pts',(-25.5181596929732,5.74073771545223,0.987845900950795));
#48561=CARTESIAN_POINT('Ctrl Pts',(-25.2795220278539,2.27261851380574,5.36349812090215));
#48562=CARTESIAN_POINT('Ctrl Pts',(-25.0408843627347,-3.28341736958705,
4.8115564455539));
#48563=CARTESIAN_POINT('Ctrl Pts',(-24.8022466976155,-5.82288757406612,
-0.160894387632515));
#48564=CARTESIAN_POINT('Ctrl Pts',(-24.5636090324963,-3.01271047268094,
-4.98552724498736));
#48565=CARTESIAN_POINT('Ctrl Pts',(-24.324971367377,2.56532662769952,-5.22981886622255));
#48566=CARTESIAN_POINT('Ctrl Pts',(-24.0863337022578,5.78652755146292,-0.669331913732308));
#48567=CARTESIAN_POINT('Ctrl Pts',(-23.8476960371386,3.69148624672874,4.50608871785483));
#48568=CARTESIAN_POINT('Ctrl Pts',(-23.6090583720193,-1.79502511668494,
5.54164154832996));
#48569=CARTESIAN_POINT('Ctrl Pts',(-23.3704207069001,-5.63239748036626,
1.48593569020165));
#48570=CARTESIAN_POINT('Ctrl Pts',(-23.1317830417809,-4.29513117367219,
-3.93494020808196));
#48571=CARTESIAN_POINT('Ctrl Pts',(-22.8931453766617,0.988190418061122,
-5.74067817734282));
#48572=CARTESIAN_POINT('Ctrl Pts',(-22.6545077115424,5.36363426118309,-2.27229702170649));
#48573=CARTESIAN_POINT('Ctrl Pts',(-22.4158700464232,4.81135960693467,3.28370598157288));
#48574=CARTESIAN_POINT('Ctrl Pts',(-22.177232381304,-0.161243610930449,
5.82287787425445));
#48575=CARTESIAN_POINT('Ctrl Pts',(-21.9385947161848,-4.98570788329408,
3.01241151630967));
#48576=CARTESIAN_POINT('Ctrl Pts',(-21.6999570510655,-5.22966502916022,
-2.56564025607911));
#48577=CARTESIAN_POINT('Ctrl Pts',(-21.4613193859463,-0.668984900732974,
-5.78656767379734));
#48578=CARTESIAN_POINT('Ctrl Pts',(-21.2226817208271,4.50631007820199,-3.69121602185732));
#48579=CARTESIAN_POINT('Ctrl Pts',(-20.9840440557079,5.54153389565618,1.79535743632542));
#48580=CARTESIAN_POINT('Ctrl Pts',(-20.7454063905886,1.4855979230446,5.63248657805113));
#48581=CARTESIAN_POINT('Ctrl Pts',(-20.5067687254694,-3.93519777116089,
4.29489519578073));
#48582=CARTESIAN_POINT('Ctrl Pts',(-20.2681310603502,-5.74061890739093,
-0.988534673640199));
#48583=CARTESIAN_POINT('Ctrl Pts',(-20.0294933952309,-2.27197537096228,
-5.36377051658862));
#48584=CARTESIAN_POINT('Ctrl Pts',(-19.7908557301117,3.28399450334934,-4.81116268098024));
#48585=CARTESIAN_POINT('Ctrl Pts',(-19.5522180649925,5.82286819435154,0.161592797159601));
#48586=CARTESIAN_POINT('Ctrl Pts',(-19.3135803998733,3.01211252782197,4.98588852268307));
#48587=CARTESIAN_POINT('Ctrl Pts',(-19.074942734754,-2.56595386414308,5.22951116338557));
#48588=CARTESIAN_POINT('Ctrl Pts',(-18.8363050696348,-5.78660778110002,
0.668637890488963));
#48589=CARTESIAN_POINT('Ctrl Pts',(-18.5976674045156,-3.69094578070135,
-4.50653142503277));
#48590=CARTESIAN_POINT('Ctrl Pts',(-18.3590297393963,1.79568974794104,-5.54142622165309));
#48591=CARTESIAN_POINT('Ctrl Pts',(-18.1203920742771,5.63257565629784,-1.48526015127511));
#48592=CARTESIAN_POINT('Ctrl Pts',(-17.8817544091579,4.29465920201836,3.93545532046853));
#48593=CARTESIAN_POINT('Ctrl Pts',(-17.6431167440387,-0.988878925442489,
5.74055961659669));
#48594=CARTESIAN_POINT('Ctrl Pts',(-17.4044790789195,-5.36390675282074,
2.2716537121509));
#48595=CARTESIAN_POINT('Ctrl Pts',(-17.1658414138002,-4.81096573766385,
-3.28428301336982));
#48596=CARTESIAN_POINT('Ctrl Pts',(-16.927203748681,0.161941982776275,-5.82285849348062));
#48597=CARTESIAN_POINT('Ctrl Pts',(-16.6885660835618,4.98606914415835,-3.01181352851682));
#48598=CARTESIAN_POINT('Ctrl Pts',(-16.4499284184425,5.22935727879621,2.56626746298708));
#48599=CARTESIAN_POINT('Ctrl Pts',(-16.2112907533233,0.668290877844823,
5.78664786758917));
#48600=CARTESIAN_POINT('Ctrl Pts',(-15.9726530882041,-4.50675275565964,
3.69067552627418));
#48601=CARTESIAN_POINT('Ctrl Pts',(-15.7340154230849,-5.5413185277209,-1.79602205310015));
#48602=CARTESIAN_POINT('Ctrl Pts',(-15.4953777579656,-1.48492237416498,
-5.63266471428835));
#48603=CARTESIAN_POINT('Ctrl Pts',(-15.2567400928464,3.93571285562398,-4.29442319281195));
#48604=CARTESIAN_POINT('Ctrl Pts',(-15.0181024277272,5.74050030515826,0.989223173688781));
#48605=CARTESIAN_POINT('Ctrl Pts',(-14.779464762608,2.2713320451704,5.36404296976328));
#48606=CARTESIAN_POINT('Ctrl Pts',(-14.5408270974887,-3.28457151157951,
4.81076877704648));
#48607=CARTESIAN_POINT('Ctrl Pts',(-14.3021894323695,-5.82284877166972,
-0.16229116781057));
#48608=CARTESIAN_POINT('Ctrl Pts',(-14.0635517672503,-3.01151451838073,
-4.98624974770287));
#48609=CARTESIAN_POINT('Ctrl Pts',(-13.824914102131,2.56658105260234,-5.22920337540123));
#48610=CARTESIAN_POINT('Ctrl Pts',(-13.5862764370118,5.78668793326858,-0.667943862797434));
#48611=CARTESIAN_POINT('Ctrl Pts',(-13.3476387718926,3.69040525857474,4.50697407007948));
#48612=CARTESIAN_POINT('Ctrl Pts',(-13.1090011067734,-1.79635435180044,
5.54121081386123));
#48613=CARTESIAN_POINT('Ctrl Pts',(-12.8703634416541,-5.63275375202288,
1.48458459171485));
#48614=CARTESIAN_POINT('Ctrl Pts',(-12.6317257765349,-4.29418716816209,
-3.93597037662593));
#48615=CARTESIAN_POINT('Ctrl Pts',(-12.3930881114157,0.989567418377627,
-5.74044097307606));
#48616=CARTESIAN_POINT('Ctrl Pts',(-12.1544504462965,5.36417916741587,-2.27101037002181));
#48617=CARTESIAN_POINT('Ctrl Pts',(-11.9158127811772,4.81057179912879,3.28485999797732));
#48618=CARTESIAN_POINT('Ctrl Pts',(-11.677175116058,-0.162640352261234,
5.82283902891891));
#48619=CARTESIAN_POINT('Ctrl Pts',(-11.4385374509388,-4.98643033331604,
3.01121549741473));
#48620=CARTESIAN_POINT('Ctrl Pts',(-11.1998997858196,-5.22904945320118,
-2.56689463298775));
#48621=CARTESIAN_POINT('Ctrl Pts',(-10.9612621207004,-0.667596845348008,
-5.78672797813811));
#48622=CARTESIAN_POINT('Ctrl Pts',(-10.7226244555811,4.50719536829151,-3.69013497760401));
#48623=CARTESIAN_POINT('Ctrl Pts',(-10.4839867904619,5.54110308007444,1.79668664404075));
#48624=CARTESIAN_POINT('Ctrl Pts',(-10.2453491253427,1.48424680392591,5.63284276950108));
#48625=CARTESIAN_POINT('Ctrl Pts',(-10.0067114602234,-3.93622788347351,
4.29395112806967));
#48626=CARTESIAN_POINT('Ctrl Pts',(-9.7680737951042,-5.74038162035028,-0.989911659507881));
#48627=CARTESIAN_POINT('Ctrl Pts',(-9.52943612998498,-2.27068868670629,
-5.36431534577795));
#48628=CARTESIAN_POINT('Ctrl Pts',(-9.29079846486575,3.2851484725623,-4.81037480391155));
#48629=CARTESIAN_POINT('Ctrl Pts',(-9.05216079974653,5.82282926522816,0.162989536127165));
#48630=CARTESIAN_POINT('Ctrl Pts',(-8.81352313462729,3.01091646561997,4.98661090099698));
#48631=CARTESIAN_POINT('Ctrl Pts',(-8.57488546950808,-2.56720820414237,
5.22889551219701));
#48632=CARTESIAN_POINT('Ctrl Pts',(-8.33624780438884,-5.78676800219732,
0.667249825496974));
#48633=CARTESIAN_POINT('Ctrl Pts',(-8.09761013926962,-3.6898646833635,-4.50741665029341));
#48634=CARTESIAN_POINT('Ctrl Pts',(-7.85897247415039,1.79701892982099,-5.54099532636385));
#48635=CARTESIAN_POINT('Ctrl Pts',(-7.62033480903117,5.6329317667206,-1.48390901079377));
#48636=CARTESIAN_POINT('Ctrl Pts',(-7.38169714391194,4.29371507253944,3.93648537615507));
#48637=CARTESIAN_POINT('Ctrl Pts',(-7.14305947879271,-0.990255897085868,
5.74032224700168));
#48638=CARTESIAN_POINT('Ctrl Pts',(-6.90442181367349,-5.36445150483438,
2.27036699518559));
#48639=CARTESIAN_POINT('Ctrl Pts',(-6.66578414855427,-4.81017779142361,
-3.28543693525765));
#48640=CARTESIAN_POINT('Ctrl Pts',(-6.42714648343502,0.163338719461003,
-5.82281948074281));
#48641=CARTESIAN_POINT('Ctrl Pts',(-6.18850881831581,4.98679145064144,-3.0106174227187));
#48642=CARTESIAN_POINT('Ctrl Pts',(-5.94987115319658,5.2287415525881,2.56752176552981));
#48643=CARTESIAN_POINT('Ctrl Pts',(-5.71123348807735,0.666902802864079,
5.78680800647329));
#48644=CARTESIAN_POINT('Ctrl Pts',(-5.47259582295812,-4.50763791535213,
3.68959437388266));
#48645=CARTESIAN_POINT('Ctrl Pts',(-5.2339581578389,-5.54088755413527,-1.79735120535602));
#48646=CARTESIAN_POINT('Ctrl Pts',(-4.99532049271967,-1.48357120962223,
-5.63302075094351));
#48647=CARTESIAN_POINT('Ctrl Pts',(-4.75668282760044,3.93674284949249,-4.29347898763361));
#48648=CARTESIAN_POINT('Ctrl Pts',(-4.51804516248123,5.74026286296703,0.990600104358038));
#48649=CARTESIAN_POINT('Ctrl Pts',(-4.27940749736199,2.27004527638976,5.36458769593022));
#48650=CARTESIAN_POINT('Ctrl Pts',(-4.04076983224277,-3.28572534945949,
4.80998066311877));
#48651=CARTESIAN_POINT('Ctrl Pts',(-3.80213216712354,-5.82280974571438,
-0.16368771312168));
#48652=CARTESIAN_POINT('Ctrl Pts',(-3.56349450200431,-3.0103182338791,-4.98697234526281));
#48653=CARTESIAN_POINT('Ctrl Pts',(-3.32485683688509,2.56783505836581,-5.22858687764632));
#48654=CARTESIAN_POINT('Ctrl Pts',(-3.08621917176586,5.78684848764546,-0.666557114673928));
#48655=CARTESIAN_POINT('Ctrl Pts',(-2.84758150664664,3.68932309589099,4.50786172998432));
#48656=CARTESIAN_POINT('Ctrl Pts',(-2.60894384152741,-1.79768164104147,
5.54077483750139));
#48657=CARTESIAN_POINT('Ctrl Pts',(-2.37030617640819,-5.63311323370599,
1.48324285461269));
#48658=CARTESIAN_POINT('Ctrl Pts',(-2.13166851128895,-4.29323613370083,
-3.93701844882378));
#48659=CARTESIAN_POINT('Ctrl Pts',(-1.89303084616973,0.990931345983249,
-5.7401686421007));
#48660=CARTESIAN_POINT('Ctrl Pts',(-1.65439318105051,5.36474874573582,-2.26979037177858));
#48661=CARTESIAN_POINT('Ctrl Pts',(-1.41575551593128,4.80973576926203,3.28614200352924));
#48662=CARTESIAN_POINT('Ctrl Pts',(-1.17711785081205,-0.163945061774615,
5.82255383487542));
#48663=CARTESIAN_POINT('Ctrl Pts',(-0.938480185692826,-4.98732912999593,
3.0104915028476));
#48664=CARTESIAN_POINT('Ctrl Pts',(-0.699842520573593,-5.22809441916263,
-2.56905538786673));
#48665=CARTESIAN_POINT('Ctrl Pts',(-0.461204855454365,-0.666861035834833,
-5.78514584226827));
#48666=CARTESIAN_POINT('Ctrl Pts',(-0.222567190335147,4.50934465203849,
-3.6924177249843));
#48667=CARTESIAN_POINT('Ctrl Pts',(0.016070474784088,5.53813222627847,1.80465927151925));
#48668=CARTESIAN_POINT('Ctrl Pts',(0.214935195716776,2.16371145271264,4.98307551377353));
#48669=CARTESIAN_POINT('Ctrl Pts',(0.374026972462927,-1.23643196713973,
4.97495722373696));
#48670=CARTESIAN_POINT('Ctrl Pts',(0.453572860835998,-2.72416315711316,
4.18423143996577));
#48671=CARTESIAN_POINT('Ctrl Pts',(0.493345805022534,-3.32886324744157,
3.62964109518183));
#48672=CARTESIAN_POINT('',(0.,4.77615934004779,1.20163511869213));
#48673=CARTESIAN_POINT('Ctrl Pts',(1.27675647831893E-15,4.78202092340378,
1.20708649626074));
#48674=CARTESIAN_POINT('Ctrl Pts',(1.54554986213376E-15,4.74680432306751,
1.31141193121661));
#48675=CARTESIAN_POINT('Ctrl Pts',(-1.2200289887242E-15,4.70790283853999,
1.41429721113204));
#48676=CARTESIAN_POINT('Ctrl Pts',(-1.0547118733939E-15,4.66526667899838,
1.51554882908261));
#48677=CARTESIAN_POINT('Ctrl Pts',(-8.36120983837436E-16,4.60951044466766,
1.64795777485803));
#48678=CARTESIAN_POINT('Ctrl Pts',(1.7406482083505E-15,4.5473685300075,
1.77757428418243));
#48679=CARTESIAN_POINT('Ctrl Pts',(9.99200722162641E-16,4.47921304648044,
1.90412989878513));
#48680=CARTESIAN_POINT('Ctrl Pts',(5.41776053129587E-16,4.43716556493129,
1.98220644662206));
#48681=CARTESIAN_POINT('Ctrl Pts',(-6.14882986343895E-16,4.39282838373583,
2.05911740148693));
#48682=CARTESIAN_POINT('Ctrl Pts',(-5.55111512312578E-16,4.34628172346416,
2.13479307691151));
#48683=CARTESIAN_POINT('Ctrl Pts',(-5.12735502418862E-16,4.31328167171442,
2.18844464268728));
#48684=CARTESIAN_POINT('Ctrl Pts',(7.5446052363616E-15,4.27917094813153,
2.24147520753853));
#48685=CARTESIAN_POINT('Ctrl Pts',(7.32747196252603E-15,4.24397679643589,
2.29385817644388));
#48686=CARTESIAN_POINT('Ctrl Pts',(7.25033478916171E-15,4.23147398038747,
2.31246736554886));
#48687=CARTESIAN_POINT('Ctrl Pts',(1.1248375135418E-15,4.21883292816165,
2.33099695996549));
#48688=CARTESIAN_POINT('Ctrl Pts',(9.43689570931383E-16,4.20605981758978,
2.34943854375472));
#48689=CARTESIAN_POINT('Ctrl Pts',(-2.0749684309091E-16,4.12488731768033,
2.46663391680332));
#48690=CARTESIAN_POINT('Ctrl Pts',(1.20832359191774E-15,4.03848405238999,
2.58013740696103));
#48691=CARTESIAN_POINT('Ctrl Pts',(2.72004641033163E-15,3.94721695353052,
2.68968900864157));
#48692=CARTESIAN_POINT('Ctrl Pts',(4.18855970728122E-15,3.85855853902716,
2.79610930064906));
#48693=CARTESIAN_POINT('Ctrl Pts',(1.88596569557423E-15,3.7653095628778,
2.89880063696627));
#48694=CARTESIAN_POINT('Ctrl Pts',(-4.9960036108132E-16,3.66777702457831,
2.99748899318237));
#48695=CARTESIAN_POINT('Ctrl Pts',(-2.58697066065493E-15,3.58243605356626,
3.08384130487147));
#48696=CARTESIAN_POINT('Ctrl Pts',(-1.9993502333868E-15,3.49381479608703,
3.16712847527816));
#48697=CARTESIAN_POINT('Ctrl Pts',(-3.60822483003176E-15,3.40210641955682,
3.24714114973565));
#48698=CARTESIAN_POINT('Ctrl Pts',(-3.93090312754506E-15,3.38371325027676,
3.26318861150008));
#48699=CARTESIAN_POINT('Ctrl Pts',(-8.00198331154243E-15,3.36519389765555,
3.27910584403603));
#48700=CARTESIAN_POINT('Ctrl Pts',(-7.93809462606987E-15,3.34656787360052,
3.29487610387643));
#48701=CARTESIAN_POINT('Ctrl Pts',(-7.56940933970987E-15,3.23908184596226,
3.38588224560911));
#48702=CARTESIAN_POINT('Ctrl Pts',(9.69472795872832E-15,3.12792305846971,
3.4721065544235));
#48703=CARTESIAN_POINT('Ctrl Pts',(8.60422844084496E-15,3.01343370374636,
3.55329630674216));
#48704=CARTESIAN_POINT('Ctrl Pts',(7.5193745599244E-15,2.89953707311163,
3.63406573070746));
#48705=CARTESIAN_POINT('Ctrl Pts',(1.54891535256133E-14,2.78234353560187,
3.70985298607676));
#48706=CARTESIAN_POINT('Ctrl Pts',(1.29340982368831E-14,2.66216592270983,
3.78036399292217));
#48707=CARTESIAN_POINT('Ctrl Pts',(1.04428067996356E-14,2.54498745723108,
3.84911533006954));
#48708=CARTESIAN_POINT('Ctrl Pts',(9.06092894879522E-15,2.42497131537325,
3.91285066923259));
#48709=CARTESIAN_POINT('Ctrl Pts',(1.10467190950203E-14,2.30239503897639,
3.9712502394403));
#48710=CARTESIAN_POINT('Ctrl Pts',(1.25360617046891E-14,2.21046283167875,
4.01504991709609));
#48711=CARTESIAN_POINT('Ctrl Pts',(1.14694130650435E-14,2.11709024431302,
4.05584730347416));
#48712=CARTESIAN_POINT('Ctrl Pts',(1.04916075827077E-14,2.02239293435179,
4.09348836738669));
#48713=CARTESIAN_POINT('Ctrl Pts',(1.01019433215215E-14,1.98465520635888,
4.10848866921022));
#48714=CARTESIAN_POINT('Ctrl Pts',(1.58900622876451E-14,1.94670710034945,
4.12298752598548));
#48715=CARTESIAN_POINT('Ctrl Pts',(1.63757896132211E-14,1.90855596787325,
4.1369744095719));
#48716=CARTESIAN_POINT('Ctrl Pts',(1.66667902990066E-14,1.8856995109076,
4.14535399313934));
#48717=CARTESIAN_POINT('Ctrl Pts',(-3.74501732116749E-15,1.8627701834264,
4.15354980834729));
#48718=CARTESIAN_POINT('Ctrl Pts',(-4.38538094726937E-15,1.83976957424201,
4.16155951178909));
#48719=CARTESIAN_POINT('Ctrl Pts',(-4.90190327326717E-15,1.8212171023791,
4.16802020144052));
#48720=CARTESIAN_POINT('Ctrl Pts',(9.50430379515547E-15,1.80262497700585,
4.17435742449665));
#48721=CARTESIAN_POINT('Ctrl Pts',(9.38138455808257E-15,1.784001553863,
4.18056782352897));
#48722=CARTESIAN_POINT('Ctrl Pts',(8.54497039802425E-15,1.65727692396478,
4.22282699966724));
#48723=CARTESIAN_POINT('Ctrl Pts',(7.75693411885647E-15,1.52899676754921,
4.25925543233605));
#48724=CARTESIAN_POINT('Ctrl Pts',(7.66053886991358E-15,1.39943774817802,
4.28958765120325));
#48725=CARTESIAN_POINT('Ctrl Pts',(7.59729281300995E-15,1.31443255133079,
4.30948897685494));
#48726=CARTESIAN_POINT('Ctrl Pts',(1.2113674912629E-15,1.2288765362281,
4.32676501145738));
#48727=CARTESIAN_POINT('Ctrl Pts',(1.0547118733939E-15,1.14284625117365,
4.34132862407617));
#48728=CARTESIAN_POINT('Ctrl Pts',(8.68428161696615E-16,1.01006019941622,
4.36380727351629));
#48729=CARTESIAN_POINT('Ctrl Pts',(4.15203095003235E-15,0.876143569520156,
4.37982636972409));
#48730=CARTESIAN_POINT('Ctrl Pts',(4.94049245958195E-15,0.741565045486008,
4.38948206088079));
#48731=CARTESIAN_POINT('Ctrl Pts',(5.72761812915067E-15,0.607214529250332,
4.39912139301662));
#48732=CARTESIAN_POINT('Ctrl Pts',(1.10432148395374E-14,0.472203479324102,
4.40241856966672));
#48733=CARTESIAN_POINT('Ctrl Pts',(1.14075415780235E-14,0.337013667456073,
4.39942001130783));
#48734=CARTESIAN_POINT('Ctrl Pts',(1.15826238267446E-14,0.272046335208114,
4.39797901265212));
#48735=CARTESIAN_POINT('Ctrl Pts',(9.92588300807085E-15,0.207038030887552,
4.39508336506645));
#48736=CARTESIAN_POINT('Ctrl Pts',(1.02695629777827E-14,0.142044407157708,
4.39073446593813));
#48737=CARTESIAN_POINT('Ctrl Pts',(1.03617903745677E-14,0.124603202396043,
4.38956742776066));
#48738=CARTESIAN_POINT('Ctrl Pts',(4.4841957176862E-15,0.107164810159224,
4.38829579344102));
#48739=CARTESIAN_POINT('Ctrl Pts',(4.69069227904129E-15,0.0897419980454403,
4.38692068583962));
#48740=CARTESIAN_POINT('Ctrl Pts',(6.25118297356027E-15,-0.0419218708223804,
4.37652902313169));
#48741=CARTESIAN_POINT('Ctrl Pts',(-5.49571088697169E-16,-0.17288184694056,
4.36022055581769));
#48742=CARTESIAN_POINT('Ctrl Pts',(8.60422844084496E-16,-0.302702434116573,
4.33812072407467));
#48743=CARTESIAN_POINT('Ctrl Pts',(2.26456079903569E-15,-0.431983851255918,
4.31611267721224));
#48744=CARTESIAN_POINT('Ctrl Pts',(1.75511797657805E-14,-0.560136154997887,
4.28836093293126));
#48745=CARTESIAN_POINT('Ctrl Pts',(1.48214773787458E-14,-0.686713620784949,
4.25494071804226));
#48746=CARTESIAN_POINT('Ctrl Pts',(1.23397585715295E-14,-0.80179198203985,
4.22455660868837));
#48747=CARTESIAN_POINT('Ctrl Pts',(-2.35332166972068E-15,-0.915568901399882,
4.18948643033132));
#48748=CARTESIAN_POINT('Ctrl Pts',(-5.99520433297585E-15,-1.02768958167645,
4.14975498030284));
#48749=CARTESIAN_POINT('Ctrl Pts',(-8.67136215211543E-15,-1.11007901125274,
4.12055919326328));
#48750=CARTESIAN_POINT('Ctrl Pts',(6.0234625807556E-15,-1.19157368030025,
4.08884575090022));
#48751=CARTESIAN_POINT('Ctrl Pts',(4.84334794492725E-15,-1.27206424811892,
4.05464924064616));
#48752=CARTESIAN_POINT('Ctrl Pts',(4.19130181297638E-15,-1.31653752369003,
4.03575471840195));
#48753=CARTESIAN_POINT('Ctrl Pts',(7.59797375755575E-15,-1.36070412856013,
4.01610202232593));
#48754=CARTESIAN_POINT('Ctrl Pts',(7.70217223333702E-15,-1.40454455699869,
3.99569611765175));
#48755=CARTESIAN_POINT('Ctrl Pts',(7.75609059491098E-15,-1.42723014864851,
3.98513691380336));
#48756=CARTESIAN_POINT('Ctrl Pts',(-7.46205461605755E-15,-1.44982838930905,
3.97437601887541));
#48757=CARTESIAN_POINT('Ctrl Pts',(-8.10462807976364E-15,-1.47233648956831,
3.96341406098191));
#48758=CARTESIAN_POINT('Ctrl Pts',(-8.59111957832261E-15,-1.48937734177172,
3.95511477751635));
#48759=CARTESIAN_POINT('Ctrl Pts',(5.51713801836789E-15,-1.50635977342605,
3.94670349607368));
#48760=CARTESIAN_POINT('Ctrl Pts',(5.68989300120393E-15,-1.52327621904144,
3.93818410740871));
#48761=CARTESIAN_POINT('Ctrl Pts',(6.8760654734775E-15,-1.63942813424693,
3.87968817201454));
#48762=CARTESIAN_POINT('Ctrl Pts',(4.1445617132442E-15,-1.75256979369442,
3.81605162100472));
#48763=CARTESIAN_POINT('Ctrl Pts',(4.69069227904129E-15,-1.8623899266764,
3.74745962400277));
#48764=CARTESIAN_POINT('Ctrl Pts',(5.22545435247209E-15,-1.96992399580907,
3.68029546796622));
#48765=CARTESIAN_POINT('Ctrl Pts',(5.0249819177936E-15,-2.07427385910768,
3.60837941731036));
#48766=CARTESIAN_POINT('Ctrl Pts',(6.27276008913213E-15,-2.17511326369545,
3.53184659443599));
#48767=CARTESIAN_POINT('Ctrl Pts',(7.56032798375268E-15,-2.27916828152011,
3.45287325776349));
#48768=CARTESIAN_POINT('Ctrl Pts',(-5.02292661063484E-15,-2.37948625932775,
3.36898369722969));
#48769=CARTESIAN_POINT('Ctrl Pts',(-4.60395610524245E-15,-2.47566144275777,
3.28029126749575));
#48770=CARTESIAN_POINT('Ctrl Pts',(-4.21077948966132E-15,-2.56591560775799,
3.19705918098456));
#48771=CARTESIAN_POINT('Ctrl Pts',(5.23948052523968E-15,-2.65252139743486,
3.10959674386589));
#48772=CARTESIAN_POINT('Ctrl Pts',(5.31345800691696E-15,-2.73509733308257,
3.0179750570285));
#48773=CARTESIAN_POINT('Ctrl Pts',(5.31831121266542E-15,-2.74051463029901,
3.01196432393565));
#48774=CARTESIAN_POINT('Ctrl Pts',(2.3894388675905E-18,-2.74591456605251,
3.00593568341939));
#48775=CARTESIAN_POINT('Ctrl Pts',(-1.38777878078145E-17,-2.75129702511903,
2.99988915288068));
#48776=CARTESIAN_POINT('Ctrl Pts',(-0.808841525903593,-4.91703434725887,
-0.0013692803956027));
#48777=CARTESIAN_POINT('Ctrl Pts',(-0.772508524126926,-4.91859034973346,
-0.753815327274128));
#48778=CARTESIAN_POINT('Ctrl Pts',(-0.73617552235026,-4.75666071795644,
-1.50557039925234));
#48779=CARTESIAN_POINT('Ctrl Pts',(-0.699842520573593,-4.42776130708021,
-2.1751459818146));
#48780=CARTESIAN_POINT('Ctrl Pts',(-0.620296632200516,-3.70768329138669,
-3.64108553933391));
#48781=CARTESIAN_POINT('Ctrl Pts',(-0.540750743827439,-2.18727216361073,
-4.71311569080111));
#48782=CARTESIAN_POINT('Ctrl Pts',(-0.461204855454364,-0.564365651743867,
-4.90034274698736));
#48783=CARTESIAN_POINT('Ctrl Pts',(-0.381658967081291,1.05854086012297,
-5.08756980317361));
#48784=CARTESIAN_POINT('Ctrl Pts',(-0.302113078708221,2.78394275608069,
-4.38999376407897));
#48785=CARTESIAN_POINT('Ctrl Pts',(-0.222567190335146,3.81810829976624,
-3.12502624511441));
#48786=CARTESIAN_POINT('Ctrl Pts',(-0.148378126890099,4.78263047309757,
-1.94524489575994));
#48787=CARTESIAN_POINT('Ctrl Pts',(-0.0741890634450472,5.14588079318518,
-0.271918139693744));
#48788=CARTESIAN_POINT('Ctrl Pts',(1.31838984174237E-15,4.78202092340378,
1.20708649626074));
#48789=CARTESIAN_POINT('',(-29.575,-2.36230756092323,-3.31488661006752));
#48790=CARTESIAN_POINT('Ctrl Pts',(-29.575,-2.36826780557339,-3.31775809990771));
#48791=CARTESIAN_POINT('Ctrl Pts',(-29.575,-2.44830306796112,-3.27276844726465));
#48792=CARTESIAN_POINT('Ctrl Pts',(-29.575,-2.52655779909889,-3.22498344987375));
#48793=CARTESIAN_POINT('Ctrl Pts',(-29.575,-2.60286326628888,-3.1744359090982));
#48794=CARTESIAN_POINT('Ctrl Pts',(-29.575,-2.70499541343267,-3.106779828055));
#48795=CARTESIAN_POINT('Ctrl Pts',(-29.575,-2.80363682654566,-3.03417684171155));
#48796=CARTESIAN_POINT('Ctrl Pts',(-29.575,-2.89869614562238,-2.9570330604008));
#48797=CARTESIAN_POINT('Ctrl Pts',(-29.575,-2.96224887403662,-2.90545791942454));
#48798=CARTESIAN_POINT('Ctrl Pts',(-29.575,-3.02420016779924,-2.85185208063885));
#48799=CARTESIAN_POINT('Ctrl Pts',(-29.575,-3.08451737823507,-2.79632528183713));
#48800=CARTESIAN_POINT('Ctrl Pts',(-29.575,-3.11868159705198,-2.76487439591655));
#48801=CARTESIAN_POINT('Ctrl Pts',(-29.575,-3.15232148638354,-2.73280706845916));
#48802=CARTESIAN_POINT('Ctrl Pts',(-29.575,-3.18543039276807,-2.70014206823866));
#48803=CARTESIAN_POINT('Ctrl Pts',(-29.575,-3.20694675023592,-2.67891419035985));
#48804=CARTESIAN_POINT('Ctrl Pts',(-29.575,-3.22824271002023,-2.65742973362904));
#48805=CARTESIAN_POINT('Ctrl Pts',(-29.575,-3.24929376278556,-2.63571743596404));
#48806=CARTESIAN_POINT('Ctrl Pts',(-29.575,-3.33714135858251,-2.54511041643103));
#48807=CARTESIAN_POINT('Ctrl Pts',(-29.575,-3.42079165100367,-2.45047748262222));
#48808=CARTESIAN_POINT('Ctrl Pts',(-29.575,-3.50014704916176,-2.35224076529156));
#48809=CARTESIAN_POINT('Ctrl Pts',(-29.575,-3.58105807397336,-2.25207828538672));
#48810=CARTESIAN_POINT('Ctrl Pts',(-29.575,-3.65750467553342,-2.14816887047587));
#48811=CARTESIAN_POINT('Ctrl Pts',(-29.575,-3.72935582339607,-2.04091404902635));
#48812=CARTESIAN_POINT('Ctrl Pts',(-29.575,-3.76079070058598,-1.99399006464218));
#48813=CARTESIAN_POINT('Ctrl Pts',(-29.575,-3.79134558154171,-1.94642520728123));
#48814=CARTESIAN_POINT('Ctrl Pts',(-29.575,-3.82100749080666,-1.89825079032625));
#48815=CARTESIAN_POINT('Ctrl Pts',(-29.575,-3.83626358617193,-1.87347310347317));
#48816=CARTESIAN_POINT('Ctrl Pts',(-29.575,-3.85128343521349,-1.84853414389017));
#48817=CARTESIAN_POINT('Ctrl Pts',(-29.575,-3.86606513313638,-1.82343804723132));
#48818=CARTESIAN_POINT('Ctrl Pts',(-29.575,-3.87962032072916,-1.80042429740151));
#48819=CARTESIAN_POINT('Ctrl Pts',(-29.575,-3.8929775187076,-1.77727417891757));
#48820=CARTESIAN_POINT('Ctrl Pts',(-29.575,-3.90612065588015,-1.75401710046083));
#48821=CARTESIAN_POINT('Ctrl Pts',(-29.575,-3.97117453777595,-1.63890278526318));
#48822=CARTESIAN_POINT('Ctrl Pts',(-29.575,-4.03105238509688,-1.52106386401277));
#48823=CARTESIAN_POINT('Ctrl Pts',(-29.575,-4.08564840782879,-1.40094223444012));
#48824=CARTESIAN_POINT('Ctrl Pts',(-29.575,-4.14101887615531,-1.27911667732505));
#48825=CARTESIAN_POINT('Ctrl Pts',(-29.575,-4.19095714201348,-1.1549425736421));
#48826=CARTESIAN_POINT('Ctrl Pts',(-29.575,-4.23531866325731,-1.0288395166209));
#48827=CARTESIAN_POINT('Ctrl Pts',(-29.575,-4.27963521656908,-0.902864286453708));
#48828=CARTESIAN_POINT('Ctrl Pts',(-29.575,-4.31838678906507,-0.774963270506112));
#48829=CARTESIAN_POINT('Ctrl Pts',(-29.575,-4.35138804153719,-0.645524185385383));
#48830=CARTESIAN_POINT('Ctrl Pts',(-29.575,-4.37561871456528,-0.550485484921972));
#48831=CARTESIAN_POINT('Ctrl Pts',(-29.575,-4.39674856572066,-0.45461692513887));
#48832=CARTESIAN_POINT('Ctrl Pts',(-29.575,-4.41468782191536,-0.358064990641669));
#48833=CARTESIAN_POINT('Ctrl Pts',(-29.575,-4.42224607172046,-0.317385286189321));
#48834=CARTESIAN_POINT('Ctrl Pts',(-29.575,-4.42923776471172,-0.27658421805809));
#48835=CARTESIAN_POINT('Ctrl Pts',(-29.575,-4.43565536938885,-0.235672547990024));
#48836=CARTESIAN_POINT('Ctrl Pts',(-29.575,-4.43961660695444,-0.210420004011757));
#48837=CARTESIAN_POINT('Ctrl Pts',(-29.575,-4.44335980044231,-0.185119699039305));
#48838=CARTESIAN_POINT('Ctrl Pts',(-29.575,-4.44687885001345,-0.159806585076518));
#48839=CARTESIAN_POINT('Ctrl Pts',(-29.575,-4.46586121538066,-0.0232632462829367));
#48840=CARTESIAN_POINT('Ctrl Pts',(-29.575,-4.47835132040759,0.113799339019299));
#48841=CARTESIAN_POINT('Ctrl Pts',(-29.575,-4.48420367058679,0.25094774090325));
#48842=CARTESIAN_POINT('Ctrl Pts',(-29.575,-4.48802427633214,0.340482706542299));
#48843=CARTESIAN_POINT('Ctrl Pts',(-29.575,-4.4890151135886,0.430054946692756));
#48844=CARTESIAN_POINT('Ctrl Pts',(-29.575,-4.48712517877637,0.519549617577561));
#48845=CARTESIAN_POINT('Ctrl Pts',(-29.575,-4.48432359350001,0.652213956389896));
#48846=CARTESIAN_POINT('Ctrl Pts',(-29.575,-4.47519448741699,0.784707646574493));
#48847=CARTESIAN_POINT('Ctrl Pts',(-29.575,-4.45999947400341,0.916663774321655));
#48848=CARTESIAN_POINT('Ctrl Pts',(-29.575,-4.44456005012953,1.05074240482977));
#48849=CARTESIAN_POINT('Ctrl Pts',(-29.575,-4.42285792068252,1.1842667673282));
#48850=CARTESIAN_POINT('Ctrl Pts',(-29.575,-4.39511381888785,1.31685585528468));
#48851=CARTESIAN_POINT('Ctrl Pts',(-29.575,-4.38178896280792,1.38053535472801));
#48852=CARTESIAN_POINT('Ctrl Pts',(-29.575,-4.36706965006509,1.44399910643623));
#48853=CARTESIAN_POINT('Ctrl Pts',(-29.575,-4.35097613979996,1.50720443522242));
#48854=CARTESIAN_POINT('Ctrl Pts',(-29.575,-4.34482928679442,1.53134546218391));
#48855=CARTESIAN_POINT('Ctrl Pts',(-29.575,-4.33848058918165,1.55545340805442));
#48856=CARTESIAN_POINT('Ctrl Pts',(-29.575,-4.3319391871451,1.57949701586949));
#48857=CARTESIAN_POINT('Ctrl Pts',(-29.575,-4.29596876934752,1.71171005118469));
#48858=CARTESIAN_POINT('Ctrl Pts',(-29.575,-4.25413965605729,1.84212793058693));
#48859=CARTESIAN_POINT('Ctrl Pts',(-29.575,-4.20675605414909,1.97036806915586));
#48860=CARTESIAN_POINT('Ctrl Pts',(-29.575,-4.15824257123346,2.10166614530495));
#48861=CARTESIAN_POINT('Ctrl Pts',(-29.575,-4.10390647699439,2.23068214498256));
#48862=CARTESIAN_POINT('Ctrl Pts',(-29.575,-4.04401911667263,2.35700945357488));
#48863=CARTESIAN_POINT('Ctrl Pts',(-29.575,-3.98492825956341,2.48165660617797));
#48864=CARTESIAN_POINT('Ctrl Pts',(-29.575,-3.92043243319514,2.60368687307991));
#48865=CARTESIAN_POINT('Ctrl Pts',(-29.575,-3.85074314886284,2.72270204804338));
#48866=CARTESIAN_POINT('Ctrl Pts',(-29.575,-3.79985133012436,2.80961496111749));
#48867=CARTESIAN_POINT('Ctrl Pts',(-29.575,-3.74618885745191,2.89491983557514));
#48868=CARTESIAN_POINT('Ctrl Pts',(-29.575,-3.68984439893471,2.97851803505928));
#48869=CARTESIAN_POINT('Ctrl Pts',(-29.575,-3.66391228552828,3.01699347783834));
#48870=CARTESIAN_POINT('Ctrl Pts',(-29.575,-3.63741189415848,3.05510731852617));
#48871=CARTESIAN_POINT('Ctrl Pts',(-29.575,-3.61035102303907,3.09284943609328));
#48872=CARTESIAN_POINT('Ctrl Pts',(-29.575,-3.59584650743156,3.11307905586041));
#48873=CARTESIAN_POINT('Ctrl Pts',(-29.575,-3.58118096187307,3.13320187682416));
#48874=CARTESIAN_POINT('Ctrl Pts',(-29.575,-3.56635552732019,3.15321629747535));
#48875=CARTESIAN_POINT('Ctrl Pts',(-29.575,-3.5546900145129,3.16896480586503));
#48876=CARTESIAN_POINT('Ctrl Pts',(-29.575,-3.54292488679082,3.18464691960963));
#48877=CARTESIAN_POINT('Ctrl Pts',(-29.575,-3.53107100158975,3.20024854439494));
#48878=CARTESIAN_POINT('Ctrl Pts',(-29.575,-3.444915061959,3.31364365665938));
#48879=CARTESIAN_POINT('Ctrl Pts',(-29.575,-3.353952606715,3.42295435898676));
#48880=CARTESIAN_POINT('Ctrl Pts',(-29.575,-3.25851212336527,3.52794677560707));
#48881=CARTESIAN_POINT('Ctrl Pts',(-29.575,-3.1617890061929,3.63435019539871));
#48882=CARTESIAN_POINT('Ctrl Pts',(-29.575,-3.06046638882771,3.73631912635592));
#48883=CARTESIAN_POINT('Ctrl Pts',(-29.575,-2.95483635071748,3.83359158033952));
#48884=CARTESIAN_POINT('Ctrl Pts',(-29.575,-2.84930340889874,3.93077462041477));
#48885=CARTESIAN_POINT('Ctrl Pts',(-29.575,-2.73947053698142,4.02327043490703));
#48886=CARTESIAN_POINT('Ctrl Pts',(-29.575,-2.62558525501093,4.11078989098106));
#48887=CARTESIAN_POINT('Ctrl Pts',(-29.575,-2.51319651570498,4.19715927219268));
#48888=CARTESIAN_POINT('Ctrl Pts',(-29.575,-2.39686069001292,4.27868275896332));
#48889=CARTESIAN_POINT('Ctrl Pts',(-29.575,-2.27677987968084,4.3550468235479));
#48890=CARTESIAN_POINT('Ctrl Pts',(-29.575,-2.24098328939054,4.37781126963447));
#48891=CARTESIAN_POINT('Ctrl Pts',(-29.575,-2.20485367910692,4.40011694506889));
#48892=CARTESIAN_POINT('Ctrl Pts',(-29.575,-2.16839587231048,4.42195480991686));
#48893=CARTESIAN_POINT('Ctrl Pts',(-29.575,-2.36826780557337,-3.31775809990772));
#48894=CARTESIAN_POINT('Ctrl Pts',(-29.5008109365549,-1.33928601121754,
-4.04293436335451));
#48895=CARTESIAN_POINT('Ctrl Pts',(-29.3470759847368,1.55637121596689,-4.50701225231274));
#48896=CARTESIAN_POINT('Ctrl Pts',(-29.1137951445456,4.65387018191312,-1.22765401651987));
#48897=CARTESIAN_POINT('Ctrl Pts',(-28.8751574794264,3.55090078994383,3.25125842872222));
#48898=CARTESIAN_POINT('Ctrl Pts',(-28.6365198143072,-0.816478135197904,
4.74503193420896));
#48899=CARTESIAN_POINT('Ctrl Pts',(-28.4455297648071,-3.71062116286106,
2.45079400531014));
#48900=CARTESIAN_POINT('Ctrl Pts',(-28.3340856036801,-4.06733760858173,
0.547694664417248));
#48901=CARTESIAN_POINT('Ctrl Pts',(-28.3021873309261,-4.06480101368718,
0.00206955444756761));
#48902=CARTESIAN_POINT('Origin',(-29.575,-4.52129938221115E-16,0.));
#48903=CARTESIAN_POINT('',(-29.575,-4.925,-6.03138548580071E-16));
#48904=CARTESIAN_POINT('Origin',(-29.575,0.,0.));
#48905=CARTESIAN_POINT('Origin',(-29.575,0.,0.));
#48906=CARTESIAN_POINT('',(-29.575,2.36230756092324,-3.31488661006752));
#48907=CARTESIAN_POINT('Ctrl Pts',(-29.575,2.17494790042119,4.42655504786424));
#48908=CARTESIAN_POINT('Ctrl Pts',(-29.575,2.26967152441801,4.37041752782518));
#48909=CARTESIAN_POINT('Ctrl Pts',(-29.575,2.36222031470781,4.31097507135364));
#48910=CARTESIAN_POINT('Ctrl Pts',(-29.575,2.45239463893034,4.24821920794634));
#48911=CARTESIAN_POINT('Ctrl Pts',(-29.575,2.57031754301399,4.16615201503894));
#48912=CARTESIAN_POINT('Ctrl Pts',(-29.575,2.68418134028915,4.07841926504524));
#48913=CARTESIAN_POINT('Ctrl Pts',(-29.575,2.793800816624,3.98544075385194));
#48914=CARTESIAN_POINT('Ctrl Pts',(-29.575,2.86142888819741,3.928079073063));
#48915=CARTESIAN_POINT('Ctrl Pts',(-29.575,2.92744077307288,3.8687200679563));
#48916=CARTESIAN_POINT('Ctrl Pts',(-29.575,2.99178498903163,3.80745669486626));
#48917=CARTESIAN_POINT('Ctrl Pts',(-29.575,3.03740293232873,3.76402296833516));
#48918=CARTESIAN_POINT('Ctrl Pts',(-29.575,3.08218251964483,3.71963195357705));
#48919=CARTESIAN_POINT('Ctrl Pts',(-29.575,3.12610340234575,3.67431582845979));
#48920=CARTESIAN_POINT('Ctrl Pts',(-29.575,3.14170642099533,3.65821714596868));
#48921=CARTESIAN_POINT('Ctrl Pts',(-29.575,3.15720284290207,3.64199979656664));
#48922=CARTESIAN_POINT('Ctrl Pts',(-29.575,3.17258572052557,3.62567157287578));
#48923=CARTESIAN_POINT('Ctrl Pts',(-29.575,3.27034309847291,3.52190657040855));
#48924=CARTESIAN_POINT('Ctrl Pts',(-29.575,3.36340172212969,3.41379269192058));
#48925=CARTESIAN_POINT('Ctrl Pts',(-29.575,3.45158356813246,3.30174290977256));
#48926=CARTESIAN_POINT('Ctrl Pts',(-29.575,3.53724490642985,3.19289585417305));
#48927=CARTESIAN_POINT('Ctrl Pts',(-29.575,3.61830434560196,3.08033384565738));
#48928=CARTESIAN_POINT('Ctrl Pts',(-29.575,3.69455768842054,2.96441414844495));
#48929=CARTESIAN_POINT('Ctrl Pts',(-29.575,3.76127936338681,2.86298441338408));
#48930=CARTESIAN_POINT('Ctrl Pts',(-29.575,3.82432087679273,2.75898335344391));
#48931=CARTESIAN_POINT('Ctrl Pts',(-29.575,3.88351761773973,2.65264344251299));
#48932=CARTESIAN_POINT('Ctrl Pts',(-29.575,3.89539020296671,2.63131575393826));
#48933=CARTESIAN_POINT('Ctrl Pts',(-29.575,3.90710917047629,2.60989171569305));
#48934=CARTESIAN_POINT('Ctrl Pts',(-29.575,3.91866219954629,2.58839389445723));
#48935=CARTESIAN_POINT('Ctrl Pts',(-29.575,3.98533187012549,2.46433529032153));
#48936=CARTESIAN_POINT('Ctrl Pts',(-29.575,4.04656060379988,2.33767837925172));
#48937=CARTESIAN_POINT('Ctrl Pts',(-29.575,4.10217235556336,2.20881042226382));
#48938=CARTESIAN_POINT('Ctrl Pts',(-29.575,4.15749625211679,2.08060950617376));
#48939=CARTESIAN_POINT('Ctrl Pts',(-29.575,4.20726139736363,1.95021957273537));
#48940=CARTESIAN_POINT('Ctrl Pts',(-29.575,4.25124518841383,1.81800776290176));
#48941=CARTESIAN_POINT('Ctrl Pts',(-29.575,4.29413119192342,1.68909581590603));
#48942=CARTESIAN_POINT('Ctrl Pts',(-29.575,4.33152087503006,1.55845109390724));
#48943=CARTESIAN_POINT('Ctrl Pts',(-29.575,4.36315916984956,1.42641155759016));
#48944=CARTESIAN_POINT('Ctrl Pts',(-29.575,4.38688789096419,1.32738190535235));
#48945=CARTESIAN_POINT('Ctrl Pts',(-29.575,4.40738049178401,1.22756756386048));
#48946=CARTESIAN_POINT('Ctrl Pts',(-29.575,4.42451035861733,1.12711368795651));
#48947=CARTESIAN_POINT('Ctrl Pts',(-29.575,4.43133674032546,1.08708205737504));
#48948=CARTESIAN_POINT('Ctrl Pts',(-29.575,4.4376289049131,1.04694890359475));
#48949=CARTESIAN_POINT('Ctrl Pts',(-29.575,4.44337808320161,1.00672360633312));
#48950=CARTESIAN_POINT('Ctrl Pts',(-29.575,4.44682246179442,0.982624309733816));
#48951=CARTESIAN_POINT('Ctrl Pts',(-29.575,4.45007193773189,0.958491942467769));
#48952=CARTESIAN_POINT('Ctrl Pts',(-29.575,4.45312454919313,0.934328545878378));
#48953=CARTESIAN_POINT('Ctrl Pts',(-29.575,4.45558677843594,0.914838406879834));
#48954=CARTESIAN_POINT('Ctrl Pts',(-29.575,4.45791999829306,0.895335151707175));
#48955=CARTESIAN_POINT('Ctrl Pts',(-29.575,4.46012266207708,0.87582765091181));
#48956=CARTESIAN_POINT('Ctrl Pts',(-29.575,4.47511104469547,0.743085700928035));
#48957=CARTESIAN_POINT('Ctrl Pts',(-29.575,4.48407271847718,0.610034498076699));
#48958=CARTESIAN_POINT('Ctrl Pts',(-29.575,4.48680554393477,0.476999857930275));
#48959=CARTESIAN_POINT('Ctrl Pts',(-29.575,4.48859856927288,0.389714927249725));
#48960=CARTESIAN_POINT('Ctrl Pts',(-29.575,4.48770920842808,0.302437045899035));
#48961=CARTESIAN_POINT('Ctrl Pts',(-29.575,4.48406815367479,0.215259203818982));
#48962=CARTESIAN_POINT('Ctrl Pts',(-29.575,4.47844824112982,0.0807015326092455));
#48963=CARTESIAN_POINT('Ctrl Pts',(-29.575,4.46627498023888,-0.0536189903864601));
#48964=CARTESIAN_POINT('Ctrl Pts',(-29.575,4.44773981895834,-0.187263918132325));
#48965=CARTESIAN_POINT('Ctrl Pts',(-29.575,4.42923611011045,-0.320682062953368));
#48966=CARTESIAN_POINT('Ctrl Pts',(-29.575,4.40439160268717,-0.453427703408474));
#48967=CARTESIAN_POINT('Ctrl Pts',(-29.575,4.37335182340664,-0.58503925570624));
#48968=CARTESIAN_POINT('Ctrl Pts',(-29.575,4.35843537009352,-0.648286405680295));
#48969=CARTESIAN_POINT('Ctrl Pts',(-29.575,4.34208757622849,-0.711271201901602));
#48970=CARTESIAN_POINT('Ctrl Pts',(-29.575,4.32432137404194,-0.773939500968908));
#48971=CARTESIAN_POINT('Ctrl Pts',(-29.575,4.31955371135246,-0.790756899990894));
#48972=CARTESIAN_POINT('Ctrl Pts',(-29.575,4.31468432223976,-0.807549803851364));
#48973=CARTESIAN_POINT('Ctrl Pts',(-29.575,4.30971696019155,-0.824305954558689));
#48974=CARTESIAN_POINT('Ctrl Pts',(-29.575,4.27217870230904,-0.950931857858156));
#48975=CARTESIAN_POINT('Ctrl Pts',(-29.575,4.22899927473913,-1.07563909243635));
#48976=CARTESIAN_POINT('Ctrl Pts',(-29.575,4.18039187949891,-1.19802776435577));
#48977=CARTESIAN_POINT('Ctrl Pts',(-29.575,4.13198650007613,-1.3199077801853));
#48978=CARTESIAN_POINT('Ctrl Pts',(-29.575,4.07819767353095,-1.43948920797592));
#48979=CARTESIAN_POINT('Ctrl Pts',(-29.575,4.01919161106764,-1.55635171305596));
#48980=CARTESIAN_POINT('Ctrl Pts',(-29.575,3.96554454554038,-1.66260063403094));
#48981=CARTESIAN_POINT('Ctrl Pts',(-29.575,3.90758410693226,-1.7666021746683));
#48982=CARTESIAN_POINT('Ctrl Pts',(-29.575,3.84540829196954,-1.86801442537029));
#48983=CARTESIAN_POINT('Ctrl Pts',(-29.575,3.79972079463418,-1.9425333027907));
#48984=CARTESIAN_POINT('Ctrl Pts',(-29.575,3.7517566228007,-2.01565352617642));
#48985=CARTESIAN_POINT('Ctrl Pts',(-29.575,3.70157235710967,-2.08727533440549));
#48986=CARTESIAN_POINT('Ctrl Pts',(-29.575,3.67384420437395,-2.12684830434812));
#48987=CARTESIAN_POINT('Ctrl Pts',(-29.575,3.64543819285622,-2.16596367436737));
#48988=CARTESIAN_POINT('Ctrl Pts',(-29.575,3.61636323740365,-2.20460339725076));
#48989=CARTESIAN_POINT('Ctrl Pts',(-29.575,3.60131842230507,-2.22459749447954));
#48990=CARTESIAN_POINT('Ctrl Pts',(-29.575,3.58609448820911,-2.24446422067884));
#48991=CARTESIAN_POINT('Ctrl Pts',(-29.575,3.57069262976354,-2.26420097811176));
#48992=CARTESIAN_POINT('Ctrl Pts',(-29.575,3.55903139036739,-2.27914430810939));
#48993=CARTESIAN_POINT('Ctrl Pts',(-29.575,3.54727273939743,-2.29400720550239));
#48994=CARTESIAN_POINT('Ctrl Pts',(-29.575,3.53542205698418,-2.30878307744774));
#48995=CARTESIAN_POINT('Ctrl Pts',(-29.575,3.45405476451608,-2.41023484639433));
#48996=CARTESIAN_POINT('Ctrl Pts',(-29.575,3.36828498238971,-2.50767334973966));
#48997=CARTESIAN_POINT('Ctrl Pts',(-29.575,3.27835860536771,-2.60083261446428));
#48998=CARTESIAN_POINT('Ctrl Pts',(-29.575,3.19030403000318,-2.69205278554481));
#48999=CARTESIAN_POINT('Ctrl Pts',(-29.575,3.09826340014138,-2.77917034507256));
#49000=CARTESIAN_POINT('Ctrl Pts',(-29.575,3.00243676957963,-2.86189425854725));
#49001=CARTESIAN_POINT('Ctrl Pts',(-29.575,2.90355461728311,-2.94725590136843));
#49002=CARTESIAN_POINT('Ctrl Pts',(-29.575,2.80064068610558,-3.02794003035809));
#49003=CARTESIAN_POINT('Ctrl Pts',(-29.575,2.69389027200841,-3.10357332294541));
#49004=CARTESIAN_POINT('Ctrl Pts',(-29.575,2.59371175266095,-3.17455038967486));
#49005=CARTESIAN_POINT('Ctrl Pts',(-29.575,2.49015393838355,-3.24107925145737));
#49006=CARTESIAN_POINT('Ctrl Pts',(-29.575,2.38336574054609,-3.30280154424992));
#49007=CARTESIAN_POINT('Ctrl Pts',(-29.575,2.37636023875519,-3.30685063995014));
#49008=CARTESIAN_POINT('Ctrl Pts',(-29.575,2.36934083188486,-3.31087903158254));
#49009=CARTESIAN_POINT('Ctrl Pts',(-29.575,2.36230756092332,-3.31488661006746));
#49010=CARTESIAN_POINT('Origin',(-29.575,0.,0.));
#49011=CARTESIAN_POINT('Origin',(-32.3478126690739,0.,0.));
#49012=CARTESIAN_POINT('Ctrl Pts',(-29.575,2.36230756092324,-3.31488661006752));
#49013=CARTESIAN_POINT('Ctrl Pts',(-29.5352270558135,2.91456939066647,-2.92132494432319));
#49014=CARTESIAN_POINT('Ctrl Pts',(-29.4556811674404,3.80947864266608,-1.85446537575054));
#49015=CARTESIAN_POINT('Ctrl Pts',(-29.2965893906943,4.40029930288375,0.892938679230673));
#49016=CARTESIAN_POINT('Ctrl Pts',(-29.0977246697615,2.41062119233501,4.16711865021482));
#49017=CARTESIAN_POINT('Ctrl Pts',(-28.8590870046423,-2.21020820766824,
4.28001845847083));
#49018=CARTESIAN_POINT('Ctrl Pts',(-28.6924496710798,-4.01269863755865,
1.60905902128973));
#49019=CARTESIAN_POINT('Ctrl Pts',(-28.6053582258903,-4.07619291884947,
0.130177206130288));
#49020=CARTESIAN_POINT('Ctrl Pts',(-28.5978126690739,-4.07533558288693,
0.00197868943318465));
#49021=CARTESIAN_POINT('Ctrl Pts',(-30.0683458050225,2.85821514250009,-4.01076441581692));
#49022=CARTESIAN_POINT('Ctrl Pts',(-30.028572860836,3.52641057585851,-3.5345842895939));
#49023=CARTESIAN_POINT('Ctrl Pts',(-29.9490269724629,4.60918371579173,-2.24376415073622));
#49024=CARTESIAN_POINT('Ctrl Pts',(-29.7899351957168,5.32403244483542,1.08038889453645));
#49025=CARTESIAN_POINT('Ctrl Pts',(-29.5910704747841,2.91667101639856,5.0419013271853));
#49026=CARTESIAN_POINT('Ctrl Pts',(-29.3524328096649,-2.6741863217702,5.17850163566369));
#49027=CARTESIAN_POINT('Ctrl Pts',(-29.1137951445457,-5.7973743179944,0.550511209599409));
#49028=CARTESIAN_POINT('Ctrl Pts',(-28.8751574794264,-3.59989778886694,
-4.57971187869854));
#49029=CARTESIAN_POINT('Ctrl Pts',(-28.6365198143073,1.9077811732274,-5.50426057988267));
#49030=CARTESIAN_POINT('Ctrl Pts',(-28.3978821491879,5.66123134949523,-1.37093968550409));
#49031=CARTESIAN_POINT('Ctrl Pts',(-28.1592444840688,4.21433244584917,4.02140449350459));
#49032=CARTESIAN_POINT('Ctrl Pts',(-27.9206068189495,-1.10479606405923,
5.71943238413845));
#49033=CARTESIAN_POINT('Ctrl Pts',(-27.6819691538303,-5.40870633854705,
2.16272545229035));
#49034=CARTESIAN_POINT('Ctrl Pts',(-27.4433314887111,-4.74359941984978,
-3.380866692594));
#49035=CARTESIAN_POINT('Ctrl Pts',(-27.2046938235918,0.279640350988314,
-5.8184000833979));
#49036=CARTESIAN_POINT('Ctrl Pts',(-26.9660561584726,5.04593690996907,-2.91039003941573));
#49037=CARTESIAN_POINT('Ctrl Pts',(-26.7274184933533,5.17640786355619,2.67146555315453));
#49038=CARTESIAN_POINT('Ctrl Pts',(-26.4887808282342,0.551162248122564,
5.79897734693768));
#49039=CARTESIAN_POINT('Ctrl Pts',(-26.2501431631149,-4.58044707277724,
3.59880626920218));
#49040=CARTESIAN_POINT('Ctrl Pts',(-26.0115054979957,-5.50387573699426,
-1.90768582721621));
#49041=CARTESIAN_POINT('Ctrl Pts',(-25.7728678328765,-1.37074105079164,
-5.66153515210527));
#49042=CARTESIAN_POINT('Ctrl Pts',(-25.5342301677573,4.02173058771444,-4.21397584735458));
#49043=CARTESIAN_POINT('Ctrl Pts',(-25.295592502638,5.71932789822544,1.10507891249598));
#49044=CARTESIAN_POINT('Ctrl Pts',(-25.0569548375188,2.16242101025971,5.40886734761332));
#49045=CARTESIAN_POINT('Ctrl Pts',(-24.8183171723995,-3.38116152304108,
4.74338034983671));
#49046=CARTESIAN_POINT('Ctrl Pts',(-24.5796795072803,-5.81837790032782,
-0.27998076825629));
#49047=CARTESIAN_POINT('Ctrl Pts',(-24.3410418421611,-2.91009025392015,
-5.04611585917912));
#49048=CARTESIAN_POINT('Ctrl Pts',(-24.1024041770419,2.67177743350171,-5.17624534512243));
#49049=CARTESIAN_POINT('Ctrl Pts',(-23.8637665119226,5.79900962484977,-0.550815695476877));
#49050=CARTESIAN_POINT('Ctrl Pts',(-23.6251288468035,3.59853198023136,4.58066350376895));
#49051=CARTESIAN_POINT('Ctrl Pts',(-23.3864911816842,-1.90801608760284,
5.50376100088902));
#49052=CARTESIAN_POINT('Ctrl Pts',(-23.147853516565,-5.66161723459444,1.37040170709392));
#49053=CARTESIAN_POINT('Ctrl Pts',(-22.9092158514458,-4.21373472077718,
-4.02198337277209));
#49054=CARTESIAN_POINT('Ctrl Pts',(-22.6705781863265,1.10542191660648,-5.71926157245085));
#49055=CARTESIAN_POINT('Ctrl Pts',(-22.4319405212073,5.40899699874395,-2.16209667128711));
#49056=CARTESIAN_POINT('Ctrl Pts',(-22.1933028560881,4.74317758767807,3.38144598062146));
#49057=CARTESIAN_POINT('Ctrl Pts',(-21.9546651909688,-0.280329688527433,
5.81836109345686));
#49058=CARTESIAN_POINT('Ctrl Pts',(-21.7160275258496,-5.04629036031444,
2.90978764647796));
#49059=CARTESIAN_POINT('Ctrl Pts',(-21.4773898607304,-5.17608511572218,
-2.67208783967747));
#49060=CARTESIAN_POINT('Ctrl Pts',(-21.2387521956112,-0.55046793874511,
-5.79904264483125));
#49061=CARTESIAN_POINT('Ctrl Pts',(-21.0001145304919,4.58087929208444,-3.59825728089574));
#49062=CARTESIAN_POINT('Ctrl Pts',(-20.7614768653727,5.50364657119464,1.90834613410097));
#49063=CARTESIAN_POINT('Ctrl Pts',(-20.5228392002535,1.37006218854147,5.66169940456846));
#49064=CARTESIAN_POINT('Ctrl Pts',(-20.2842015351343,-4.02223605484748,
4.21349352286768));
#49065=CARTESIAN_POINT('Ctrl Pts',(-20.045563870015,-5.71919527222015,-1.10576488747686));
#49066=CARTESIAN_POINT('Ctrl Pts',(-19.8069262048958,-2.16177230051888,
-5.40912664566764));
#49067=CARTESIAN_POINT('Ctrl Pts',(-19.5682885397766,3.38173041352887,-4.74297480052089));
#49068=CARTESIAN_POINT('Ctrl Pts',(-19.3296508746573,5.81834427218029,0.28067860365368));
#49069=CARTESIAN_POINT('Ctrl Pts',(-19.0910132095381,2.90948502517622,5.04646484545742));
#49070=CARTESIAN_POINT('Ctrl Pts',(-18.8523755444189,-2.67239823447518,
5.17592486658531));
#49071=CARTESIAN_POINT('Ctrl Pts',(-18.6137378792997,-5.79907564487983,
0.550120180618539));
#49072=CARTESIAN_POINT('Ctrl Pts',(-18.3751002141804,-3.59798256814023,
-4.58109506423096));
#49073=CARTESIAN_POINT('Ctrl Pts',(-18.1364625490612,1.90867617348636,-5.50353212154956));
#49074=CARTESIAN_POINT('Ctrl Pts',(-17.897824883942,5.66178155431231,-1.3697226651447));
#49075=CARTESIAN_POINT('Ctrl Pts',(-17.6591872188228,4.2132523097379,4.02248872250135));
#49076=CARTESIAN_POINT('Ctrl Pts',(-17.4205495537035,-1.10610785433544,
5.71912895139983));
#49077=CARTESIAN_POINT('Ctrl Pts',(-17.1819118885843,-5.40925627315763,
2.16144792198822));
#49078=CARTESIAN_POINT('Ctrl Pts',(-16.9432742234651,-4.74277199629759,
-3.38201483428115));
#49079=CARTESIAN_POINT('Ctrl Pts',(-16.7046365583458,0.281027517765593,
-5.81832742997681));
#49080=CARTESIAN_POINT('Ctrl Pts',(-16.4659988932266,5.04663931245511,-2.90918239341314));
#49081=CARTESIAN_POINT('Ctrl Pts',(-16.2273612281074,5.17576459883361,2.67270861966342));
#49082=CARTESIAN_POINT('Ctrl Pts',(-15.9887235629882,0.549772420514306,
5.79910862407352));
#49083=CARTESIAN_POINT('Ctrl Pts',(-15.750085897869,-4.5813108199035,3.597707842446));
#49084=CARTESIAN_POINT('Ctrl Pts',(-15.5114482327497,-5.50341765211267,
-1.90900620600798));
#49085=CARTESIAN_POINT('Ctrl Pts',(-15.2728105676305,-1.36938313682227,
-5.66186368369541));
#49086=CARTESIAN_POINT('Ctrl Pts',(-15.0341729025113,4.02274137568974,-4.21301108145661));
#49087=CARTESIAN_POINT('Ctrl Pts',(-14.7955352373921,5.71906261001256,1.10645081721627));
#49088=CARTESIAN_POINT('Ctrl Pts',(-14.5568975722728,2.16112353568466,5.40938588119503));
#49089=CARTESIAN_POINT('Ctrl Pts',(-14.3182599071536,-3.38229924287111,
4.74256917501852));
#49090=CARTESIAN_POINT('Ctrl Pts',(-14.0796222420344,-5.81831056684969,
-0.281376430866862));
#49091=CARTESIAN_POINT('Ctrl Pts',(-13.8409845769151,-2.90887975118817,
-5.04681376130423));
#49092=CARTESIAN_POINT('Ctrl Pts',(-13.6023469117959,2.67301899524012,-5.17560431246901));
#49093=CARTESIAN_POINT('Ctrl Pts',(-13.3637092466767,5.79914158241269,-0.549424658433007));
#49094=CARTESIAN_POINT('Ctrl Pts',(-13.1250715815575,3.5974331038138,4.5815265591009));
#49095=CARTESIAN_POINT('Ctrl Pts',(-12.8864339164382,-1.90933623166449,
5.50330316288458));
#49096=CARTESIAN_POINT('Ctrl Pts',(-12.647796251319,-5.66194579271754,1.3690436035753));
#49097=CARTESIAN_POINT('Ctrl Pts',(-12.4091585861998,-4.21276983802462,
-4.0229940144117));
#49098=CARTESIAN_POINT('Ctrl Pts',(-12.1705209210806,1.10679377611814,-5.7189962480586));
#49099=CARTESIAN_POINT('Ctrl Pts',(-11.9318832559613,5.4095154697794,-2.16079914160935));
#49100=CARTESIAN_POINT('Ctrl Pts',(-11.6932455908421,4.74236633668439,3.38258363929778));
#49101=CARTESIAN_POINT('Ctrl Pts',(-11.4546079257229,-0.281725342956251,
5.81829368279896));
#49102=CARTESIAN_POINT('Ctrl Pts',(-11.2159702606036,-5.04698819200419,
2.9085770985024));
#49103=CARTESIAN_POINT('Ctrl Pts',(-10.9773325954844,-5.17544400749208,
-2.67332936120422));
#49104=CARTESIAN_POINT('Ctrl Pts',(-10.7386949303652,-0.549076894375944,
-5.79917451989717));
#49105=CARTESIAN_POINT('Ctrl Pts',(-10.5000572652459,4.58174228182235,-3.5971583522447));
#49106=CARTESIAN_POINT('Ctrl Pts',(-10.2614196001268,5.50318865386573,1.9096662504547));
#49107=CARTESIAN_POINT('Ctrl Pts',(-10.0227819350075,1.36870406540507,5.66202788137834));
#49108=CARTESIAN_POINT('Ctrl Pts',(-9.78414426988828,-4.02324663866633,
4.21252857944289));
#49109=CARTESIAN_POINT('Ctrl Pts',(-9.54550660476906,-5.71892986553813,
-1.10713673103989));
#49110=CARTESIAN_POINT('Ctrl Pts',(-9.30686893964983,-2.16047473976357,
-5.40964503891006));
#49111=CARTESIAN_POINT('Ctrl Pts',(-9.0682312745306,3.38286802356034,-4.74216348129631));
#49112=CARTESIAN_POINT('Ctrl Pts',(-8.82959360941138,5.81827677782428,0.282074254033242));
#49113=CARTESIAN_POINT('Ctrl Pts',(-8.59095594429215,2.90827443535771,5.04716260455295));
#49114=CARTESIAN_POINT('Ctrl Pts',(-8.35231827917293,-2.67363971755611,
5.1752836839061));
#49115=CARTESIAN_POINT('Ctrl Pts',(-8.1136806140537,-5.79920743652394,0.548729128339138));
#49116=CARTESIAN_POINT('Ctrl Pts',(-7.87504294893448,-3.59688358774524,
-4.58195798805725));
#49117=CARTESIAN_POINT('Ctrl Pts',(-7.63640528381524,1.90999626238828,-5.50307412507543));
#49118=CARTESIAN_POINT('Ctrl Pts',(-7.39776761869603,5.66210994965676,-1.36836452227643));
#49119=CARTESIAN_POINT('Ctrl Pts',(-7.15912995357678,4.21228730575213,4.0234992483829));
#49120=CARTESIAN_POINT('Ctrl Pts',(-6.92049228845757,-1.10747968205672,
5.7188634625854));
#49121=CARTESIAN_POINT('Ctrl Pts',(-6.68185462333833,-5.40977458843978,
2.16015032989127));
#49122=CARTESIAN_POINT('Ctrl Pts',(-6.44321695821912,-4.74196060913677,
-3.38315239516401));
#49123=CARTESIAN_POINT('Ctrl Pts',(-6.20457929309988,0.282423164637435,
-5.81825985287354));
#49124=CARTESIAN_POINT('Ctrl Pts',(-5.96594162798066,5.04733699791161,-2.90797175993565));
#49125=CARTESIAN_POINT('Ctrl Pts',(-5.72730396286144,5.17512334370478,2.6739500608018));
#49126=CARTESIAN_POINT('Ctrl Pts',(-5.4886662977422,0.548381356497653,5.79924033899806));
#49127=CARTESIAN_POINT('Ctrl Pts',(-5.25002863262299,-4.58217367045971,
3.59660879744466));
#49128=CARTESIAN_POINT('Ctrl Pts',(-5.01139096750376,-5.5029595906143,-1.91032624275442));
#49129=CARTESIAN_POINT('Ctrl Pts',(-4.77275330238452,-1.3680249471228,-5.66219204498688));
#49130=CARTESIAN_POINT('Ctrl Pts',(-4.53411563726531,4.02375179159935,-4.21204592589478));
#49131=CARTESIAN_POINT('Ctrl Pts',(-4.29547797214607,5.71879713894916,1.10782245436525));
#49132=CARTESIAN_POINT('Ctrl Pts',(-4.05684030702685,2.1598257205091,5.40990445393106));
#49133=CARTESIAN_POINT('Ctrl Pts',(-3.81820264190762,-3.38343638652024,
4.74175707603558));
#49134=CARTESIAN_POINT('Ctrl Pts',(-3.57956497678839,-5.8182436135944,-0.282770838170588));
#49135=CARTESIAN_POINT('Ctrl Pts',(-3.34092731166917,-2.90766771762518,
-5.04751374594047));
#49136=CARTESIAN_POINT('Ctrl Pts',(-3.10228964654994,2.67425779052882,-5.17495842985376));
#49137=CARTESIAN_POINT('Ctrl Pts',(-2.86365198143071,5.79927821925697,-0.54804232686631));
#49138=CARTESIAN_POINT('Ctrl Pts',(-2.62501431631149,3.59632439845965,4.58240612234822));
#49139=CARTESIAN_POINT('Ctrl Pts',(-2.38637665119227,-1.91063779555211,
5.5028128128105));
#49140=CARTESIAN_POINT('Ctrl Pts',(-2.14773898607303,-5.66230948168428,
1.36774722574033));
#49141=CARTESIAN_POINT('Ctrl Pts',(-1.90910132095381,-4.21173664772448,
-4.02412306903384));
#49142=CARTESIAN_POINT('Ctrl Pts',(-1.67046365583459,1.10803490710056,-5.71850283364837));
#49143=CARTESIAN_POINT('Ctrl Pts',(-1.43182599071535,5.41028448303652,-2.15993873727599));
#49144=CARTESIAN_POINT('Ctrl Pts',(-1.19318832559614,4.74107307396736,3.3845606937213));
#49145=CARTESIAN_POINT('Ctrl Pts',(-0.954550660476906,-0.282194523950606,
5.81661222925236));
#49146=CARTESIAN_POINT('Ctrl Pts',(-0.715912995357673,-5.049479635978,2.91048227618002));
#49147=CARTESIAN_POINT('Ctrl Pts',(-0.477275330238451,-5.17121721536142,
-2.68071843402506));
#49148=CARTESIAN_POINT('Ctrl Pts',(-0.278410609305759,-1.32510607804596,
-5.26845855246328));
#49149=CARTESIAN_POINT('Ctrl Pts',(-0.119318832559609,2.02851289583626,
-4.70788567421457));
#49150=CARTESIAN_POINT('Ctrl Pts',(-0.0397729441865337,3.3679595299544,
-3.68587930545211));
#49151=CARTESIAN_POINT('Ctrl Pts',(4.44089209850063E-15,3.87448963569911,
-3.0403873211912));
#49152=CARTESIAN_POINT('Ctrl Pts',(-29.9038972033484,2.6929126153078,-3.77880514723378));
#49153=CARTESIAN_POINT('Ctrl Pts',(-29.8641242591618,3.32246351412783,-3.330164507837));
#49154=CARTESIAN_POINT('Ctrl Pts',(-29.7845783707887,4.34261535808318,-2.11399789240766));
#49155=CARTESIAN_POINT('Ctrl Pts',(-29.6254865940426,5.0161213975182,1.01790548943452));
#49156=CARTESIAN_POINT('Ctrl Pts',(-29.4266218731099,2.74798774171071,4.75030710152848));
#49157=CARTESIAN_POINT('Ctrl Pts',(-29.1879842079907,-2.51952695040288,
4.87900724326607));
#49158=CARTESIAN_POINT('Ctrl Pts',(-28.9493465428715,-5.46208793188772,
0.518672845565351));
#49159=CARTESIAN_POINT('Ctrl Pts',(-28.7107088777522,-3.39170065447864,
-4.31484800050243));
#49160=CARTESIAN_POINT('Ctrl Pts',(-28.472071212633,1.79744621468105,-5.18592618627794));
#49161=CARTESIAN_POINT('Ctrl Pts',(-28.2334335475138,5.33381868024693,-1.29165251384495));
#49162=CARTESIAN_POINT('Ctrl Pts',(-27.9947958823946,3.97059998730579,3.78882986476014));
#49163=CARTESIAN_POINT('Ctrl Pts',(-27.7561582172753,-1.04090109033753,
5.38865370581382));
#49164=CARTESIAN_POINT('Ctrl Pts',(-27.5175205521561,-5.09589824607407,
2.03764600058257));
#49165=CARTESIAN_POINT('Ctrl Pts',(-27.2788828870369,-4.4692572402043,-3.18533704191237));
#49166=CARTESIAN_POINT('Ctrl Pts',(-27.0402452219176,0.26346758077383,-5.48189768940374));
#49167=CARTESIAN_POINT('Ctrl Pts',(-26.8016075567985,4.75410928969372,-2.74207001987724));
#49168=CARTESIAN_POINT('Ctrl Pts',(-26.5629698916792,4.87703456275017,2.51696353520732));
#49169=CARTESIAN_POINT('Ctrl Pts',(-26.32433222656,0.519286231809787,5.46359825096759));
#49170=CARTESIAN_POINT('Ctrl Pts',(-26.0856945614407,-4.31554067523491,
3.39067226195794));
#49171=CARTESIAN_POINT('Ctrl Pts',(-25.8470568963215,-5.18556360046217,
-1.79735638292817));
#49172=CARTESIAN_POINT('Ctrl Pts',(-25.6084192312023,-1.29146536700809,
-5.33410491268233));
#49173=CARTESIAN_POINT('Ctrl Pts',(-25.3697815660831,3.78913709957896,-3.97026401239249));
#49174=CARTESIAN_POINT('Ctrl Pts',(-25.1311439009638,5.38855526275784,1.04116758046706));
#49175=CARTESIAN_POINT('Ctrl Pts',(-24.8925062358446,2.03735916570693,5.09604994331312));
#49176=CARTESIAN_POINT('Ctrl Pts',(-24.6538685707254,-3.18561482108248,
4.46905083992566));
#49177=CARTESIAN_POINT('Ctrl Pts',(-24.4152309056062,-5.48187678927333,
-0.263788310288471));
#49178=CARTESIAN_POINT('Ctrl Pts',(-24.1765932404869,-2.74178757222978,
-4.75427788952306));
#49179=CARTESIAN_POINT('Ctrl Pts',(-23.9379555753677,2.51725737821055,-4.87688144343666));
#49180=CARTESIAN_POINT('Ctrl Pts',(-23.6993179102484,5.46362866211312,-0.518959721751974));
#49181=CARTESIAN_POINT('Ctrl Pts',(-23.4606802451293,3.39041383626465,4.31574458911784));
#49182=CARTESIAN_POINT('Ctrl Pts',(-23.22204258001,-1.79766754297636,5.1854555000254));
#49183=CARTESIAN_POINT('Ctrl Pts',(-22.9834049148908,-5.33418224799811,
1.29114564897465));
#49184=CARTESIAN_POINT('Ctrl Pts',(-22.7447672497716,-3.97003683117282,
-3.78937526502026));
#49185=CARTESIAN_POINT('Ctrl Pts',(-22.5061295846523,1.04149074721631,-5.38849277288));
#49186=CARTESIAN_POINT('Ctrl Pts',(-22.2674919195332,5.09617209617701,-2.03705358461264));
#49187=CARTESIAN_POINT('Ctrl Pts',(-22.0288542544139,4.46885980435008,3.18588282729214));
#49188=CARTESIAN_POINT('Ctrl Pts',(-21.7902165892947,-0.264117051042074,
5.48186095441396));
#49189=CARTESIAN_POINT('Ctrl Pts',(-21.5515789241754,-4.75444229852842,
2.74150246584068));
#49190=CARTESIAN_POINT('Ctrl Pts',(-21.3129412590562,-4.87673048077228,
-2.51754983229987));
#49191=CARTESIAN_POINT('Ctrl Pts',(-21.074303593937,-0.518632077245404,
-5.46365977241106));
#49192=CARTESIAN_POINT('Ctrl Pts',(-20.8356659288178,4.31594789749319,-3.39015502393968));
#49193=CARTESIAN_POINT('Ctrl Pts',(-20.5970282636985,5.1853476882785,1.79797850150613));
#49194=CARTESIAN_POINT('Ctrl Pts',(-20.3583905985793,1.29082576619906,5.3342596657391));
#49195=CARTESIAN_POINT('Ctrl Pts',(-20.1197529334601,-3.78961333343518,
3.96980958274648));
#49196=CARTESIAN_POINT('Ctrl Pts',(-19.8811152683408,-5.38843030706872,
-1.04181388264786));
#49197=CARTESIAN_POINT('Ctrl Pts',(-19.6424776032216,-2.0367479735616,-5.09629424507725));
#49198=CARTESIAN_POINT('Ctrl Pts',(-19.4038399381024,3.18615081025577,-4.46866874522171));
#49199=CARTESIAN_POINT('Ctrl Pts',(-19.1652022729832,5.48184510598211,0.264445786948331));
#49200=CARTESIAN_POINT('Ctrl Pts',(-18.9265646078639,2.74121734639358,4.75460669246635));
#49201=CARTESIAN_POINT('Ctrl Pts',(-18.6879269427447,-2.51784227566918,
4.87657949951273));
#49202=CARTESIAN_POINT('Ctrl Pts',(-18.4492892776255,-5.46369086392892,
0.518304431424697));
#49203=CARTESIAN_POINT('Ctrl Pts',(-18.2106516125063,-3.38989619897094,
-4.31615119063469));
#49204=CARTESIAN_POINT('Ctrl Pts',(-17.972013947387,1.7982894533345,-5.18523985773471));
#49205=CARTESIAN_POINT('Ctrl Pts',(-17.7333762822678,5.33433706441994,-1.29050587885931));
#49206=CARTESIAN_POINT('Ctrl Pts',(-17.4947386171486,3.96958231998011,3.78985138826264));
#49207=CARTESIAN_POINT('Ctrl Pts',(-17.2561009520293,-1.04213701429963,
5.38836782185863));
#49208=CARTESIAN_POINT('Ctrl Pts',(-17.0174632869101,-5.09641637566774,
2.03644235519705));
#49209=CARTESIAN_POINT('Ctrl Pts',(-16.7788256217909,-4.46847767001423,
-3.18641878176725));
#49210=CARTESIAN_POINT('Ctrl Pts',(-16.5401879566717,0.264774521898913,
-5.48182923783365));
#49211=CARTESIAN_POINT('Ctrl Pts',(-16.3015502915525,4.7547710693084,-2.74093221709016));
#49212=CARTESIAN_POINT('Ctrl Pts',(-16.0629126264332,4.87642850071492,2.51813470998477));
#49213=CARTESIAN_POINT('Ctrl Pts',(-15.824274961314,0.517976783740707,5.46372193579801));
#49214=CARTESIAN_POINT('Ctrl Pts',(-15.5856372961948,-4.31635446825496,
3.38963736181178));
#49215=CARTESIAN_POINT('Ctrl Pts',(-15.3469996310756,-5.18513200854378,
-1.79860039869607));
#49216=CARTESIAN_POINT('Ctrl Pts',(-15.1083619659563,-1.29018598687877,
-5.33441444391757));
#49217=CARTESIAN_POINT('Ctrl Pts',(-14.8697243008371,3.7900894294612,-3.9693550429385));
#49218=CARTESIAN_POINT('Ctrl Pts',(-14.6310866357179,5.38830531727106,1.0424601422037));
#49219=CARTESIAN_POINT('Ctrl Pts',(-14.3924489705986,2.03613672950916,5.09653848793067));
#49220=CARTESIAN_POINT('Ctrl Pts',(-14.1538113054794,-3.18668674181981,
4.46828657873739));
#49221=CARTESIAN_POINT('Ctrl Pts',(-13.9151736403602,-5.48181334997165,
-0.265103255897302));
#49222=CARTESIAN_POINT('Ctrl Pts',(-13.6765359752409,-2.74064707792992,
-4.75493542905149));
#49223=CARTESIAN_POINT('Ctrl Pts',(-13.4378983101217,2.51842713524471,-4.87627748438068));
#49224=CARTESIAN_POINT('Ctrl Pts',(-13.1992606450025,5.46375298801868,-0.517649134193991));
#49225=CARTESIAN_POINT('Ctrl Pts',(-12.9606229798833,3.38937851246291,4.31655773035292));
#49226=CARTESIAN_POINT('Ctrl Pts',(-12.721985314764,-1.79891133758957,5.18502414070623));
#49227=CARTESIAN_POINT('Ctrl Pts',(-12.4833476496448,-5.33449180423179,
1.28986609025851));
#49228=CARTESIAN_POINT('Ctrl Pts',(-12.2447099845256,-3.96912775162243,
-3.79032745703001));
#49229=CARTESIAN_POINT('Ctrl Pts',(-12.0060723194064,1.04278326635893,-5.38824279330623));
#49230=CARTESIAN_POINT('Ctrl Pts',(-11.7674346542871,5.0966605818656,-2.03583109649899));
#49231=CARTESIAN_POINT('Ctrl Pts',(-11.5287969891679,4.46809547139186,3.18695469041253));
#49232=CARTESIAN_POINT('Ctrl Pts',(-11.2901593240487,-0.265431988942334,
5.48179744239614));
#49233=CARTESIAN_POINT('Ctrl Pts',(-11.0515216589295,-4.75509977169506,
2.74036192891386));
#49234=CARTESIAN_POINT('Ctrl Pts',(-10.8128839938102,-4.87612645051055,
-2.51871955144797));
#49235=CARTESIAN_POINT('Ctrl Pts',(-10.574246328691,-0.517321482785775,
-5.46378402059077));
#49236=CARTESIAN_POINT('Ctrl Pts',(-10.3356086635718,4.3167609769278,-3.38911965092534));
#49237=CARTESIAN_POINT('Ctrl Pts',(-10.0969709984526,5.18491625422252,1.79922227001388));
#49238=CARTESIAN_POINT('Ctrl Pts',(-9.85833333333333,1.28954618899972,5.33456914536226));
#49239=CARTESIAN_POINT('Ctrl Pts',(-9.61969566821411,-3.79056547096819,
3.96890044603278));
#49240=CARTESIAN_POINT('Ctrl Pts',(-9.38105800309488,-5.38818024996436,
-1.04310638676421));
#49241=CARTESIAN_POINT('Ctrl Pts',(-9.14242033797565,-2.03552545616774,
-5.09678265747193));
#49242=CARTESIAN_POINT('Ctrl Pts',(-8.90378267285643,3.18722262754464,-4.46790434797868));
#49243=CARTESIAN_POINT('Ctrl Pts',(-8.6651450077372,5.48178151510679,0.265760721033513));
#49244=CARTESIAN_POINT('Ctrl Pts',(-8.42650734261798,2.74007677004376,4.7552640972372));
#49245=CARTESIAN_POINT('Ctrl Pts',(-8.18786967749874,-2.51901195859494,
4.87597539910758));
#49246=CARTESIAN_POINT('Ctrl Pts',(-7.94923201237954,-5.46381503351144,
0.516993829512319));
#49247=CARTESIAN_POINT('Ctrl Pts',(-7.71059434726029,-3.38886077720523,
-4.31696420796962));
#49248=CARTESIAN_POINT('Ctrl Pts',(-7.47195668214107,1.7995331959781,-5.18480834911082));
#49249=CARTESIAN_POINT('Ctrl Pts',(-7.23331901702184,5.33464646728914,-1.28922628306928));
#49250=CARTESIAN_POINT('Ctrl Pts',(-6.99468135190262,3.96867312620793,3.79080347120911));
#49251=CARTESIAN_POINT('Ctrl Pts',(-6.75604368678338,-1.04342950349043,
5.38811768737191));
#49252=CARTESIAN_POINT('Ctrl Pts',(-6.51740602166417,-5.09690471461091,
2.03521980827418));
#49253=CARTESIAN_POINT('Ctrl Pts',(-6.27876835654494,-4.467713208764,-3.18749055274999));
#49254=CARTESIAN_POINT('Ctrl Pts',(-6.04013069142571,0.266089452679246,
-5.48176556899668));
#49255=CARTESIAN_POINT('Ctrl Pts',(-5.80149302630648,4.75542840469908,-2.73979159960635));
#49256=CARTESIAN_POINT('Ctrl Pts',(-5.56285536118726,4.87582433205023,2.5193043533937));
#49257=CARTESIAN_POINT('Ctrl Pts',(-5.32421769606802,0.516666170769886,
5.46384603309797));
#49258=CARTESIAN_POINT('Ctrl Pts',(-5.08558003094881,-4.31716741655734,
3.38860187917618));
#49259=CARTESIAN_POINT('Ctrl Pts',(-4.84694236582958,-5.18470043865627,
-1.79984409220056));
#49260=CARTESIAN_POINT('Ctrl Pts',(-4.60830470071034,-1.28890634696599,
-5.3347238147032));
#49261=CARTESIAN_POINT('Ctrl Pts',(-4.36966703559113,3.79104140879587,-3.96844570635655));
#49262=CARTESIAN_POINT('Ctrl Pts',(-4.13102937047189,5.38805519950874,1.04375245184379));
#49263=CARTESIAN_POINT('Ctrl Pts',(-3.89239170535267,2.03491397240924,5.09702706943807));
#49264=CARTESIAN_POINT('Ctrl Pts',(-3.65375404023344,-3.18775811969919,
4.46752144683269));
#49265=CARTESIAN_POINT('Ctrl Pts',(-3.41511637511422,-5.48175026890294,
-0.266417018798925));
#49266=CARTESIAN_POINT('Ctrl Pts',(-3.17647870999499,-2.7395051413334,-4.75559493065073));
#49267=CARTESIAN_POINT('Ctrl Pts',(-2.93784104487577,2.51959428582449,-4.87566895585645));
#49268=CARTESIAN_POINT('Ctrl Pts',(-2.69920337975653,5.4638817225832,-0.516346748639057));
#49269=CARTESIAN_POINT('Ctrl Pts',(-2.46056571463731,3.38833392817308,4.31738642478165));
#49270=CARTESIAN_POINT('Ctrl Pts',(-2.22192804951809,-1.80013762659788,
5.18456214962629));
#49271=CARTESIAN_POINT('Ctrl Pts',(-1.98329038439885,-5.33483445954559,
1.28864468737176));
#49272=CARTESIAN_POINT('Ctrl Pts',(-1.74465271927964,-3.96815431503542,
-3.79139121370463));
#49273=CARTESIAN_POINT('Ctrl Pts',(-1.50601505416041,1.0439526175495,-5.38777791511351));
#49274=CARTESIAN_POINT('Ctrl Pts',(-1.26737738904118,5.09738511987209,-2.03502045294416));
#49275=CARTESIAN_POINT('Ctrl Pts',(-1.02873972392196,4.46687700346276,3.18881740351592));
#49276=CARTESIAN_POINT('Ctrl Pts',(-0.790102058802729,-0.265874035238907,
5.48021323433553));
#49277=CARTESIAN_POINT('Ctrl Pts',(-0.551464393683494,-4.75744712505124,
2.74215692220397));
#49278=CARTESIAN_POINT('Ctrl Pts',(-0.312826728564273,-4.87214411143407,
-2.52568128330601));
#49279=CARTESIAN_POINT('Ctrl Pts',(-0.113962007631581,-1.24846965546114,
-4.96376157560509));
#49280=CARTESIAN_POINT('Ctrl Pts',(0.0451297691145686,1.91119551719046,
-4.43560896973968));
#49281=CARTESIAN_POINT('Ctrl Pts',(0.124675657487644,3.17317635443185,-3.47270950061224));
#49282=CARTESIAN_POINT('Ctrl Pts',(0.164448601674182,3.65041170719118,-2.86454901554259));
#49283=CARTESIAN_POINT('Ctrl Pts',(-29.7394486016742,2.52761008811552,-3.54684587865065));
#49284=CARTESIAN_POINT('Ctrl Pts',(-29.6996756574876,3.11851645239715,-3.12574472608009));
#49285=CARTESIAN_POINT('Ctrl Pts',(-29.6201297691146,4.07604700037463,-1.9842316340791));
#49286=CARTESIAN_POINT('Ctrl Pts',(-29.4610379923684,4.70821035020098,0.955422084332599));
#49287=CARTESIAN_POINT('Ctrl Pts',(-29.2621732714357,2.57930446702286,4.45871287587165));
#49288=CARTESIAN_POINT('Ctrl Pts',(-29.0235356063165,-2.36486757903556,
4.57951285086845));
#49289=CARTESIAN_POINT('Ctrl Pts',(-28.7848979411973,-5.12680154578104,
0.486834481531294));
#49290=CARTESIAN_POINT('Ctrl Pts',(-28.546260276078,-3.18350352009034,-4.04998412230631));
#49291=CARTESIAN_POINT('Ctrl Pts',(-28.3076226109588,1.6871112561347,-4.86759179267321));
#49292=CARTESIAN_POINT('Ctrl Pts',(-28.0689849458396,5.00640601099863,-1.21236534218581));
#49293=CARTESIAN_POINT('Ctrl Pts',(-27.8303472807204,3.72686752876241,3.55625523601567));
#49294=CARTESIAN_POINT('Ctrl Pts',(-27.5917096156011,-0.977006116615824,
5.05787502748919));
#49295=CARTESIAN_POINT('Ctrl Pts',(-27.3530719504819,-4.7830901536011,1.91256654887478));
#49296=CARTESIAN_POINT('Ctrl Pts',(-27.1144342853627,-4.19491506055882,
-2.98980739123073));
#49297=CARTESIAN_POINT('Ctrl Pts',(-26.8757966202435,0.247294810559338,
-5.1453952954096));
#49298=CARTESIAN_POINT('Ctrl Pts',(-26.6371589551242,4.46228166941837,-2.57375000033875));
#49299=CARTESIAN_POINT('Ctrl Pts',(-26.398521290005,4.57766126194414,2.3624615172601));
#49300=CARTESIAN_POINT('Ctrl Pts',(-26.1598836248858,0.487410215497018,
5.12821915499749));
#49301=CARTESIAN_POINT('Ctrl Pts',(-25.9212459597666,-4.05063427769259,
3.1825382547137));
#49302=CARTESIAN_POINT('Ctrl Pts',(-25.6826082946473,-4.86725146393007,
-1.68702693864012));
#49303=CARTESIAN_POINT('Ctrl Pts',(-25.4439706295281,-1.21218968322454,
-5.0066746732594));
#49304=CARTESIAN_POINT('Ctrl Pts',(-25.2053329644089,3.55654361144349,-3.7265521774304));
#49305=CARTESIAN_POINT('Ctrl Pts',(-24.9666952992897,5.05778262729025,0.977256248438136));
#49306=CARTESIAN_POINT('Ctrl Pts',(-24.7280576341704,1.91229732115414,4.78323253901292));
#49307=CARTESIAN_POINT('Ctrl Pts',(-24.4894199690512,-2.99006811912389,
4.19472133001462));
#49308=CARTESIAN_POINT('Ctrl Pts',(-24.250782303932,-5.14537567821884,-0.247595852320659));
#49309=CARTESIAN_POINT('Ctrl Pts',(-24.0121446388127,-2.57348489053941,
-4.46243991986699));
#49310=CARTESIAN_POINT('Ctrl Pts',(-23.7735069736935,2.3627373229194,-4.57751754175089));
#49311=CARTESIAN_POINT('Ctrl Pts',(-23.5348693085743,5.12824769937646,-0.487103748027066));
#49312=CARTESIAN_POINT('Ctrl Pts',(-23.2962316434551,3.18229569229794,4.05082567446672));
#49313=CARTESIAN_POINT('Ctrl Pts',(-23.0575939783358,-1.68731899834989,
4.8671499991618));
#49314=CARTESIAN_POINT('Ctrl Pts',(-22.8189563132166,-5.00674726140177,
1.21188959085538));
#49315=CARTESIAN_POINT('Ctrl Pts',(-22.5803186480974,-3.72633894156846,
-3.55676715726841));
#49316=CARTESIAN_POINT('Ctrl Pts',(-22.3416809829781,0.97755957782614,-5.05772397330915));
#49317=CARTESIAN_POINT('Ctrl Pts',(-22.1030433178589,4.78334719361007,-1.91201049793817));
#49318=CARTESIAN_POINT('Ctrl Pts',(-21.8644056527397,4.19454202102207,2.99031967396282));
#49319=CARTESIAN_POINT('Ctrl Pts',(-21.6257679876205,-0.247904413556711,
5.14536081537106));
#49320=CARTESIAN_POINT('Ctrl Pts',(-21.3871303225013,-4.4625942367424,2.57321728520339));
#49321=CARTESIAN_POINT('Ctrl Pts',(-21.148492657382,-4.57737584582237,-2.36301182492228));
#49322=CARTESIAN_POINT('Ctrl Pts',(-20.9098549922628,-0.486796215745698,
-5.12827689999088));
#49323=CARTESIAN_POINT('Ctrl Pts',(-20.6712173271436,4.05101650290193,-3.18205276698362));
#49324=CARTESIAN_POINT('Ctrl Pts',(-20.4325796620244,4.86704880536236,1.68761086891128));
#49325=CARTESIAN_POINT('Ctrl Pts',(-20.1939419969051,1.21158934385664,5.00681992690976));
#49326=CARTESIAN_POINT('Ctrl Pts',(-19.9553043317859,-3.55699061202287,
3.72612564262527));
#49327=CARTESIAN_POINT('Ctrl Pts',(-19.7166666666667,-5.05766534191731,
-0.977862877818859));
#49328=CARTESIAN_POINT('Ctrl Pts',(-19.4780290015474,-1.91172364660431,
-4.78346184448688));
#49329=CARTESIAN_POINT('Ctrl Pts',(-19.2393913364282,2.99057120698267,-4.19436268992253));
#49330=CARTESIAN_POINT('Ctrl Pts',(-19.000753671309,5.14534593978394,0.248212970242977));
#49331=CARTESIAN_POINT('Ctrl Pts',(-18.7621160061898,2.57294966761094,4.46274853947527));
#49332=CARTESIAN_POINT('Ctrl Pts',(-18.5234783410705,-2.36328631686318,
4.57723413244015));
#49333=CARTESIAN_POINT('Ctrl Pts',(-18.2848406759513,-5.12830608297801,
0.486488682230852));
#49334=CARTESIAN_POINT('Ctrl Pts',(-18.0462030108321,-3.18180982980166,
-4.0512073170384));
#49335=CARTESIAN_POINT('Ctrl Pts',(-17.8075653457129,1.68790273318265,-4.86694759391988));
#49336=CARTESIAN_POINT('Ctrl Pts',(-17.5689276805936,5.00689257452757,-1.21128909257392));
#49337=CARTESIAN_POINT('Ctrl Pts',(-17.3302900154744,3.72591233022232,3.55721405402392));
#49338=CARTESIAN_POINT('Ctrl Pts',(-17.0916523503552,-0.978166174263816,
5.05760669231743));
#49339=CARTESIAN_POINT('Ctrl Pts',(-16.8530146852359,-4.78357647817786,
1.91143678840589));
#49340=CARTESIAN_POINT('Ctrl Pts',(-16.6143770201167,-4.19418334373088,
-2.99082272925335));
#49341=CARTESIAN_POINT('Ctrl Pts',(-16.3757393549975,0.248521526032233,
-5.14533104569049));
#49342=CARTESIAN_POINT('Ctrl Pts',(-16.1371016898783,4.46290282616169,-2.57268204076719));
#49343=CARTESIAN_POINT('Ctrl Pts',(-15.8984640247591,4.57709240259623,2.36356080030613));
#49344=CARTESIAN_POINT('Ctrl Pts',(-15.6598263596398,0.486181146967108,
5.12833524752249));
#49345=CARTESIAN_POINT('Ctrl Pts',(-15.4211886945206,-4.05139811660642,
3.18156688117757));
#49346=CARTESIAN_POINT('Ctrl Pts',(-15.1825510294014,-4.86684636497488,
-1.68819459138417));
#49347=CARTESIAN_POINT('Ctrl Pts',(-14.9439133642821,-1.21098883693528,
-5.00696520413972));
#49348=CARTESIAN_POINT('Ctrl Pts',(-14.7052756991629,3.55743748323268,-3.7256990044204));
#49349=CARTESIAN_POINT('Ctrl Pts',(-14.4666380340437,5.05754802452954,0.978469467191119));
#49350=CARTESIAN_POINT('Ctrl Pts',(-14.2280003689245,1.91114992333367,4.7836910946663));
#49351=CARTESIAN_POINT('Ctrl Pts',(-13.9893627038052,-2.99107424076851,
4.19400398245627));
#49352=CARTESIAN_POINT('Ctrl Pts',(-13.750725038686,-5.1453161330936,-0.248830080927746));
#49353=CARTESIAN_POINT('Ctrl Pts',(-13.5120873735668,-2.57241440467166,
-4.46305709679875));
#49354=CARTESIAN_POINT('Ctrl Pts',(-13.2734497084476,2.3638352752493,-4.57695065629236));
#49355=CARTESIAN_POINT('Ctrl Pts',(-13.0348120433283,5.12836439362466,-0.485873609954974));
#49356=CARTESIAN_POINT('Ctrl Pts',(-12.7961743782091,3.18132392111204,4.05158890160494));
#49357=CARTESIAN_POINT('Ctrl Pts',(-12.5575367130899,-1.68848644351467,
4.86674511852789));
#49358=CARTESIAN_POINT('Ctrl Pts',(-12.3188990479707,-5.00703781574603,
1.21068857694173));
#49359=CARTESIAN_POINT('Ctrl Pts',(-12.0802613828514,-3.72548566522024,
-3.55766089964832));
#49360=CARTESIAN_POINT('Ctrl Pts',(-11.8416237177322,0.978772756599708,
-5.05748933855386));
#49361=CARTESIAN_POINT('Ctrl Pts',(-11.602986052613,4.78380569395181,-1.91086305138862));
#49362=CARTESIAN_POINT('Ctrl Pts',(-11.3643483874938,4.19382460609933,2.99132574152728));
#49363=CARTESIAN_POINT('Ctrl Pts',(-11.1257107223745,-0.249138634928415,
5.14530120199331));
#49364=CARTESIAN_POINT('Ctrl Pts',(-10.8870730572553,-4.46321135138594,
2.57214675932532));
#49365=CARTESIAN_POINT('Ctrl Pts',(-10.6484353921361,-4.57680889352901,
-2.36410974169172));
#49366=CARTESIAN_POINT('Ctrl Pts',(-10.4097977270168,-0.485566071195607,
-5.12839352128436));
#49367=CARTESIAN_POINT('Ctrl Pts',(-10.1711600618976,4.05177967203326,-3.18108094960599));
#49368=CARTESIAN_POINT('Ctrl Pts',(-9.93252239677838,4.86664385457931,1.68877828957306));
#49369=CARTESIAN_POINT('Ctrl Pts',(-9.69388473165916,1.21038831259436,5.00711040934616));
#49370=CARTESIAN_POINT('Ctrl Pts',(-9.45524706653992,-3.55788430327004,
3.72527231262268));
#49371=CARTESIAN_POINT('Ctrl Pts',(-9.21660940142071,-5.0574306343906,-0.979076042488542));
#49372=CARTESIAN_POINT('Ctrl Pts',(-8.97797173630147,-1.91057617257191,
-4.78392027603378));
#49373=CARTESIAN_POINT('Ctrl Pts',(-8.73933407118225,2.99157723152894,-4.19364521466106));
#49374=CARTESIAN_POINT('Ctrl Pts',(-8.50069640606303,5.14528625238931,0.249447188033793));
#49375=CARTESIAN_POINT('Ctrl Pts',(-8.26205874094379,2.57187910472981,4.46336558992145));
#49376=CARTESIAN_POINT('Ctrl Pts',(-8.02342107582458,-2.36438419963377,
4.57666711430907));
#49377=CARTESIAN_POINT('Ctrl Pts',(-7.78478341070534,-5.12842263049894,
0.485258530685497));
#49378=CARTESIAN_POINT('Ctrl Pts',(-7.54614574558613,-3.18083796666522,
-4.051970427882));
#49379=CARTESIAN_POINT('Ctrl Pts',(-7.30750808046688,1.68907012956793,-4.86654257314621));
#49380=CARTESIAN_POINT('Ctrl Pts',(-7.06887041534768,5.00718298492152,-1.21008804386212));
#49381=CARTESIAN_POINT('Ctrl Pts',(-6.83023275022843,3.72505894666373,3.55810769403531));
#49382=CARTESIAN_POINT('Ctrl Pts',(-6.59159508510922,-0.979379324924138,
5.05737191215842));
#49383=CARTESIAN_POINT('Ctrl Pts',(-6.35295741998998,-4.78403484078203,
1.91028928665709));
#49384=CARTESIAN_POINT('Ctrl Pts',(-6.11431975487076,-4.19346580839123,
-2.99182871033596));
#49385=CARTESIAN_POINT('Ctrl Pts',(-5.87568208975153,0.24975574072106,-5.14527128511983));
#49386=CARTESIAN_POINT('Ctrl Pts',(-5.63704442463231,4.46351981148654,-2.57161143927705));
#49387=CARTESIAN_POINT('Ctrl Pts',(-5.39840675951308,4.57652532039568,2.3646586459856));
#49388=CARTESIAN_POINT('Ctrl Pts',(-5.15976909439384,0.48495098504212,5.12845172719788));
#49389=CARTESIAN_POINT('Ctrl Pts',(-4.92113142927463,-4.05216116265496,
3.18059496090769));
#49390=CARTESIAN_POINT('Ctrl Pts',(-4.68249376415541,-4.86644128669823,
-1.68936194164671));
#49391=CARTESIAN_POINT('Ctrl Pts',(-4.44385609903616,-1.20978774680917,
-5.00725558441954));
#49392=CARTESIAN_POINT('Ctrl Pts',(-4.20521843391696,3.55833102599239,-3.72484548681831));
#49393=CARTESIAN_POINT('Ctrl Pts',(-3.96658076879771,5.05731326006834,0.97968244932232));
#49394=CARTESIAN_POINT('Ctrl Pts',(-3.7279431036785,1.91000222430937,4.78414968494508));
#49395=CARTESIAN_POINT('Ctrl Pts',(-3.48930543855926,-2.99207985287812,
4.1932858176298));
#49396=CARTESIAN_POINT('Ctrl Pts',(-3.25066777344004,-5.14525692421147,
-0.250063199427267));
#49397=CARTESIAN_POINT('Ctrl Pts',(-3.01203010832081,-2.57134256504161,
-4.46367611536099));
#49398=CARTESIAN_POINT('Ctrl Pts',(-2.77339244320159,2.36493078112016,-4.57637948185914));
#49399=CARTESIAN_POINT('Ctrl Pts',(-2.53475477808235,5.12848522590942,-0.484651170411792));
#49400=CARTESIAN_POINT('Ctrl Pts',(-2.29611711296313,3.1803434578865,4.05236672721506));
#49401=CARTESIAN_POINT('Ctrl Pts',(-2.0574794478439,-1.68963745764365,4.86631148644208));
#49402=CARTESIAN_POINT('Ctrl Pts',(-1.81884178272468,-5.00735943740691,
1.20954214900319));
#49403=CARTESIAN_POINT('Ctrl Pts',(-1.58020411760546,-3.72457198234636,
-3.55865935837542));
#49404=CARTESIAN_POINT('Ctrl Pts',(-1.34156645248623,0.979870327998434,
-5.05705299657864));
#49405=CARTESIAN_POINT('Ctrl Pts',(-1.102928787367,4.78448575670765,-1.91010216861234));
#49406=CARTESIAN_POINT('Ctrl Pts',(-0.86429112224778,4.19268093295817,2.99307411331055));
#49407=CARTESIAN_POINT('Ctrl Pts',(-0.62565345712855,-0.24955354652721,
5.14381423941869));
#49408=CARTESIAN_POINT('Ctrl Pts',(-0.387015792009318,-4.46541461412448,
2.57383156822791));
#49409=CARTESIAN_POINT('Ctrl Pts',(-0.148378126890095,-4.57307100750672,
-2.37064413258696));
#49410=CARTESIAN_POINT('Ctrl Pts',(0.050486594042596,-1.17183323287632,
-4.6590645987469));
#49411=CARTESIAN_POINT('Ctrl Pts',(0.209578370788747,1.79387813854466,-4.16333226526479));
#49412=CARTESIAN_POINT('Ctrl Pts',(0.289124259161822,2.9783931789093,-3.25953969577237));
#49413=CARTESIAN_POINT('Ctrl Pts',(0.32889720334836,3.42633377868325,-2.68871070989398));
#49414=CARTESIAN_POINT('Ctrl Pts',(-29.575,2.36230756092324,-3.31488661006752));
#49415=CARTESIAN_POINT('Ctrl Pts',(-29.5352270558135,2.91456939066647,-2.92132494432319));
#49416=CARTESIAN_POINT('Ctrl Pts',(-29.4556811674404,3.80947864266608,-1.85446537575054));
#49417=CARTESIAN_POINT('Ctrl Pts',(-29.2965893906943,4.40029930288375,0.892938679230673));
#49418=CARTESIAN_POINT('Ctrl Pts',(-29.0977246697615,2.41062119233501,4.16711865021482));
#49419=CARTESIAN_POINT('Ctrl Pts',(-28.8590870046423,-2.21020820766824,
4.28001845847083));
#49420=CARTESIAN_POINT('Ctrl Pts',(-28.6204493395231,-4.79151515967436,
0.454996117497237));
#49421=CARTESIAN_POINT('Ctrl Pts',(-28.3818116744039,-2.97530638570203,
-3.7851202441102));
#49422=CARTESIAN_POINT('Ctrl Pts',(-28.1431740092847,1.57677629758835,-4.54925739906848));
#49423=CARTESIAN_POINT('Ctrl Pts',(-27.9045363441654,4.67899334175034,-1.13307817052668));
#49424=CARTESIAN_POINT('Ctrl Pts',(-27.6658986790463,3.48313507021902,3.32368060727122));
#49425=CARTESIAN_POINT('Ctrl Pts',(-27.4272610139269,-0.913111142894123,
4.72709634916456));
#49426=CARTESIAN_POINT('Ctrl Pts',(-27.1886233488078,-4.47028206112812,
1.78748709716699));
#49427=CARTESIAN_POINT('Ctrl Pts',(-26.9499856836885,-3.92057288091334,
-2.79427774054909));
#49428=CARTESIAN_POINT('Ctrl Pts',(-26.7113480185693,0.231122040344854,
-4.80889290141546));
#49429=CARTESIAN_POINT('Ctrl Pts',(-26.4727103534501,4.17045404914302,-2.40542998080026));
#49430=CARTESIAN_POINT('Ctrl Pts',(-26.2340726883308,4.27828796113812,2.20795949931288));
#49431=CARTESIAN_POINT('Ctrl Pts',(-25.9954350232116,0.45553419918425,4.79284005902739));
#49432=CARTESIAN_POINT('Ctrl Pts',(-25.7567973580924,-3.78572788015027,
2.97440424746946));
#49433=CARTESIAN_POINT('Ctrl Pts',(-25.5181596929732,-4.54893932739796,
-1.57669749435209));
#49434=CARTESIAN_POINT('Ctrl Pts',(-25.2795220278539,-1.132913999441,-4.67924443383647));
#49435=CARTESIAN_POINT('Ctrl Pts',(-25.0408843627347,3.32395012330801,-3.48284034246832));
#49436=CARTESIAN_POINT('Ctrl Pts',(-24.8022466976155,4.72700999182265,0.913344916409211));
#49437=CARTESIAN_POINT('Ctrl Pts',(-24.5636090324962,1.78723547660136,4.47041513471273));
#49438=CARTESIAN_POINT('Ctrl Pts',(-24.324971367377,-2.7945214171653,3.92039182010356));
#49439=CARTESIAN_POINT('Ctrl Pts',(-24.0863337022578,-4.80887456716434,
-0.231403394352836));
#49440=CARTESIAN_POINT('Ctrl Pts',(-23.8476960371386,-2.40518220884904,
-4.17060195021093));
#49441=CARTESIAN_POINT('Ctrl Pts',(-23.6090583720194,2.20821726762825,-4.27815364006511));
#49442=CARTESIAN_POINT('Ctrl Pts',(-23.3704207069001,4.7928667366398,-0.455247774302161));
#49443=CARTESIAN_POINT('Ctrl Pts',(-23.1317830417809,2.97417754833123,3.7859067598156));
#49444=CARTESIAN_POINT('Ctrl Pts',(-22.8931453766616,-1.57697045372341,
4.54884449829819));
#49445=CARTESIAN_POINT('Ctrl Pts',(-22.6545077115425,-4.67931227480544,
1.13263353273611));
#49446=CARTESIAN_POINT('Ctrl Pts',(-22.4158700464232,-3.48264105196409,
-3.32415904951658));
#49447=CARTESIAN_POINT('Ctrl Pts',(-22.177232381304,0.913628408435968,-4.7269551737383));
#49448=CARTESIAN_POINT('Ctrl Pts',(-21.9385947161847,4.47052229104313,-1.7869674112637));
#49449=CARTESIAN_POINT('Ctrl Pts',(-21.6999570510656,3.92022423769407,2.79475652063351));
#49450=CARTESIAN_POINT('Ctrl Pts',(-21.4613193859463,-0.231691776071347,
4.80886067632815));
#49451=CARTESIAN_POINT('Ctrl Pts',(-21.2226817208271,-4.17074617495639,
2.40493210456611));
#49452=CARTESIAN_POINT('Ctrl Pts',(-20.9840440557078,-4.27802121087247,
-2.20847381754468));
#49453=CARTESIAN_POINT('Ctrl Pts',(-20.7454063905886,-0.454960354245989,
-4.79289402757069));
#49454=CARTESIAN_POINT('Ctrl Pts',(-20.5067687254694,3.78608510831067,-2.97395051002756));
#49455=CARTESIAN_POINT('Ctrl Pts',(-20.2681310603502,4.54874992244621,1.57724323631644));
#49456=CARTESIAN_POINT('Ctrl Pts',(-20.0294933952309,1.13235292151423,4.67938018808041));
#49457=CARTESIAN_POINT('Ctrl Pts',(-19.7908557301117,-3.32436789061056,
3.48244170250407));
#49458=CARTESIAN_POINT('Ctrl Pts',(-19.5522180649925,-4.7269003767659,-0.91391187298986));
#49459=CARTESIAN_POINT('Ctrl Pts',(-19.3135803998733,-1.78669931964703,
-4.4706294438965));
#49460=CARTESIAN_POINT('Ctrl Pts',(-19.074942734754,2.79499160370957,-3.92005663462335));
#49461=CARTESIAN_POINT('Ctrl Pts',(-18.8363050696348,4.80884677358576,0.231980153537627));
#49462=CARTESIAN_POINT('Ctrl Pts',(-18.5976674045156,2.4046819888283,4.1708903864842));
#49463=CARTESIAN_POINT('Ctrl Pts',(-18.3590297393964,-2.20873035805718,
4.27788876536757));
#49464=CARTESIAN_POINT('Ctrl Pts',(-18.1203920742771,-4.79292130202709,
0.454672933037013));
#49465=CARTESIAN_POINT('Ctrl Pts',(-17.8817544091579,-2.97372346063237,
-3.78626344344212));
#49466=CARTESIAN_POINT('Ctrl Pts',(-17.6431167440387,1.5775160130308,-4.54865533010503));
#49467=CARTESIAN_POINT('Ctrl Pts',(-17.4044790789195,4.6794480846352,-1.13207230628853));
#49468=CARTESIAN_POINT('Ctrl Pts',(-17.1658414138002,3.48224234046452,3.3245767197852));
#49469=CARTESIAN_POINT('Ctrl Pts',(-16.927203748681,-0.914195334228,4.72684556277623));
#49470=CARTESIAN_POINT('Ctrl Pts',(-16.6885660835618,-4.47073658068798,
1.78643122161473));
#49471=CARTESIAN_POINT('Ctrl Pts',(-16.4499284184426,-3.91988901744752,
-2.79522667673945));
#49472=CARTESIAN_POINT('Ctrl Pts',(-16.2112907533233,0.232268530165553,
-4.80883285354733));
#49473=CARTESIAN_POINT('Ctrl Pts',(-15.9726530882041,4.17103458301497,-2.40443186444421));
#49474=CARTESIAN_POINT('Ctrl Pts',(-15.7340154230849,4.27775630447756,2.20898689062749));
#49475=CARTESIAN_POINT('Ctrl Pts',(-15.4953777579657,0.454385510193501,
4.79294855924697));
#49476=CARTESIAN_POINT('Ctrl Pts',(-15.2567400928464,-3.78644176495787,
2.97349640054336));
#49477=CARTESIAN_POINT('Ctrl Pts',(-15.0181024277272,-4.54856072140599,
-1.57778878407227));
#49478=CARTESIAN_POINT('Ctrl Pts',(-14.7794647626079,-1.13179168699179,
-4.67951596436188));
#49479=CARTESIAN_POINT('Ctrl Pts',(-14.5408270974888,3.32478553700414,-3.48204296590229));
#49480=CARTESIAN_POINT('Ctrl Pts',(-14.3021894323695,4.72679073178803,0.914478792178541));
#49481=CARTESIAN_POINT('Ctrl Pts',(-14.0635517672503,1.78616311715816,4.47084370140194));
#49482=CARTESIAN_POINT('Ctrl Pts',(-13.8249141021311,-2.79546173971721,
3.91972138617514));
#49483=CARTESIAN_POINT('Ctrl Pts',(-13.5862764370118,-4.80881891621556,
-0.232556905958181));
#49484=CARTESIAN_POINT('Ctrl Pts',(-13.3476387718926,-2.40418173141341,
-4.17117876454601));
#49485=CARTESIAN_POINT('Ctrl Pts',(-13.1090011067734,2.20924341525388,-4.27762382820403));
#49486=CARTESIAN_POINT('Ctrl Pts',(-12.8703634416541,4.79297579923065,-0.454098085715957));
#49487=CARTESIAN_POINT('Ctrl Pts',(-12.6317257765349,2.97326932976115,3.78662007285696));
#49488=CARTESIAN_POINT('Ctrl Pts',(-12.3930881114157,-1.57806154943975,
4.54846609634954));
#49489=CARTESIAN_POINT('Ctrl Pts',(-12.1544504462965,-4.67958382726028,
1.13151106362493));
#49490=CARTESIAN_POINT('Ctrl Pts',(-11.9158127811773,-3.48184357881804,
-3.32499434226663));
#49491=CARTESIAN_POINT('Ctrl Pts',(-11.677175116058,0.914762246840484,-4.7267358838015));
#49492=CARTESIAN_POINT('Ctrl Pts',(-11.4385374509388,4.47095080603802,-1.78589500627826));
#49493=CARTESIAN_POINT('Ctrl Pts',(-11.1998997858196,3.91955374080681,2.79569679264203));
#49494=CARTESIAN_POINT('Ctrl Pts',(-10.9612621207003,-0.232845280914501,
4.80880496159049));
#49495=CARTESIAN_POINT('Ctrl Pts',(-10.7226244555811,-4.17132293107681,
2.40393158973677));
#49496=CARTESIAN_POINT('Ctrl Pts',(-10.4839867904619,-4.27749133654748,
-2.20949993193547));
#49497=CARTESIAN_POINT('Ctrl Pts',(-10.2453491253427,-0.453810659605433,
-4.79300302197796));
#49498=CARTESIAN_POINT('Ctrl Pts',(-10.0067114602234,3.78679836713871,-2.97304224828663));
#49499=CARTESIAN_POINT('Ctrl Pts',(-9.76807379510421,4.54837145493611,1.57833430913225));
#49500=CARTESIAN_POINT('Ctrl Pts',(-9.52943612998497,1.131230436189,4.67965167333008));
#49501=CARTESIAN_POINT('Ctrl Pts',(-9.29079846486575,-3.3252031355719,3.48164417921258));
#49502=CARTESIAN_POINT('Ctrl Pts',(-9.05216079974653,-4.72668101881683,
-0.915045698212859));
#49503=CARTESIAN_POINT('Ctrl Pts',(-8.8135231346273,-1.78562688897607,-4.47105789459565));
#49504=CARTESIAN_POINT('Ctrl Pts',(-8.57488546950807,2.79593183551325,-3.91938608134342));
#49505=CARTESIAN_POINT('Ctrl Pts',(-8.33624780438884,4.80879098967182,0.233133655034067));
#49506=CARTESIAN_POINT('Ctrl Pts',(-8.09761013926962,2.40368143941586,4.17146708260569));
#49507=CARTESIAN_POINT('Ctrl Pts',(-7.85897247415039,-2.20975644067261,
4.27735882951057));
#49508=CARTESIAN_POINT('Ctrl Pts',(-7.62033480903117,-4.79303022748644,
0.453523231858677));
#49509=CARTESIAN_POINT('Ctrl Pts',(-7.38169714391193,-2.97281515612521,
-3.78697664779438));
#49510=CARTESIAN_POINT('Ctrl Pts',(-7.14305947879272,1.57860706315775,-4.5482767971816));
#49511=CARTESIAN_POINT('Ctrl Pts',(-6.90442181367349,4.6797195025539,-1.13094980465497));
#49512=CARTESIAN_POINT('Ctrl Pts',(-6.66578414855425,3.48144476711953,3.32541191686152));
#49513=CARTESIAN_POINT('Ctrl Pts',(-6.42714648343504,-0.91532914635784,
4.72662613694493));
#49514=CARTESIAN_POINT('Ctrl Pts',(-6.1885088183158,-4.47116496695316,1.78535876503999));
#49515=CARTESIAN_POINT('Ctrl Pts',(-5.94987115319659,-3.91921840801846,
-2.79616686792193));
#49516=CARTESIAN_POINT('Ctrl Pts',(-5.71123348807733,0.233422028762872,
-4.80877700124299));
#49517=CARTESIAN_POINT('Ctrl Pts',(-5.47259582295814,4.171611218274,-2.40343127894775));
#49518=CARTESIAN_POINT('Ctrl Pts',(-5.23395815783889,4.27722630874114,2.21001293857749));
#49519=CARTESIAN_POINT('Ctrl Pts',(-4.99532049271968,0.453235799314355,
4.7930574212978));
#49520=CARTESIAN_POINT('Ctrl Pts',(-4.75668282760044,-3.7871549087526,2.97258804263921));
#49521=CARTESIAN_POINT('Ctrl Pts',(-4.51804516248123,-4.54818213474018,
-1.57887979109285));
#49522=CARTESIAN_POINT('Ctrl Pts',(-4.27940749736198,-1.13066914665236,
-4.67978735413588));
#49523=CARTESIAN_POINT('Ctrl Pts',(-4.04076983224278,3.32562064318893,-3.48124526728007));
#49524=CARTESIAN_POINT('Ctrl Pts',(-3.80213216712354,4.72657132062792,0.915612446800854));
#49525=CARTESIAN_POINT('Ctrl Pts',(-3.56349450200431,1.78509047620951,4.4712723004521));
#49526=CARTESIAN_POINT('Ctrl Pts',(-3.32485683688509,-2.79640158605707,
3.91905018842691));
#49527=CARTESIAN_POINT('Ctrl Pts',(-3.08621917176585,-4.80876357952,-0.233709380055606));
#49528=CARTESIAN_POINT('Ctrl Pts',(-2.84758150664664,-2.40317998874982,
-4.17175730007125));
#49529=CARTESIAN_POINT('Ctrl Pts',(-2.60894384152741,2.21026727641583,-4.27709000786183));
#49530=CARTESIAN_POINT('Ctrl Pts',(-2.37030617640818,4.79308872923565,-0.452955592184536));
#49531=CARTESIAN_POINT('Ctrl Pts',(-2.13166851128895,2.97235298759993,3.78734702964848));
#49532=CARTESIAN_POINT('Ctrl Pts',(-1.89303084616973,-1.57913728868941,
4.54806082325786));
#49533=CARTESIAN_POINT('Ctrl Pts',(-1.6543931810505,-4.67988441526822,1.13043961063463));
#49534=CARTESIAN_POINT('Ctrl Pts',(-1.41575551593128,-3.4809896496573,-3.32592750304621));
#49535=CARTESIAN_POINT('Ctrl Pts',(-1.17711785081205,0.915788038447374,
-4.72632807804377));
#49536=CARTESIAN_POINT('Ctrl Pts',(-0.938480185692821,4.47158639354322,
-1.78518388428051));
#49537=CARTESIAN_POINT('Ctrl Pts',(-0.699842520573601,3.91848486245357,
2.79733082310517));
#49538=CARTESIAN_POINT('Ctrl Pts',(-0.461204855454373,-0.233233057815519,
4.80741524450186));
#49539=CARTESIAN_POINT('Ctrl Pts',(-0.222567190335139,-4.17338210319771,
2.40550621425186));
#49540=CARTESIAN_POINT('Ctrl Pts',(0.0160704747840829,-4.27399790357938,
-2.21560698186791));
#49541=CARTESIAN_POINT('Ctrl Pts',(0.214935195716774,-1.0951968102915,-4.35436762188871));
#49542=CARTESIAN_POINT('Ctrl Pts',(0.374026972462925,1.67656075989886,-3.8910555607899));
#49543=CARTESIAN_POINT('Ctrl Pts',(0.453572860836,2.78361000338674,-3.0463698909325));
#49544=CARTESIAN_POINT('Ctrl Pts',(0.493345805022538,3.20225585017532,-2.51287240424537));
#49545=CARTESIAN_POINT('',(4.44089209850063E-15,3.87448963569911,-3.0403873211912));
#49546=CARTESIAN_POINT('Ctrl Pts',(1.88737914186277E-15,-3.73764785372982,
-1.62671566533137));
#49547=CARTESIAN_POINT('Ctrl Pts',(2.39994637830129E-15,-3.71028158849173,
-1.71435575517499));
#49548=CARTESIAN_POINT('Ctrl Pts',(-1.76827187884598E-15,-3.67981086869404,
-1.80083539107987));
#49549=CARTESIAN_POINT('Ctrl Pts',(-3.27515792264421E-15,-3.64623269726973,
-1.88598270617316));
#49550=CARTESIAN_POINT('Ctrl Pts',(-5.28932042256129E-15,-3.60128953503947,
-1.99994929319637));
#49551=CARTESIAN_POINT('Ctrl Pts',(4.56536624768121E-15,-3.55078180752455,
-2.11152991672815));
#49552=CARTESIAN_POINT('Ctrl Pts',(6.43929354282591E-15,-3.49508775615109,
-2.22055078808827));
#49553=CARTESIAN_POINT('Ctrl Pts',(7.69212451415013E-15,-3.45785299647819,
-2.29343767356915));
#49554=CARTESIAN_POINT('Ctrl Pts',(-5.3505723180461E-15,-3.41829895641058,
-2.36518031524366));
#49555=CARTESIAN_POINT('Ctrl Pts',(-5.38458166943201E-15,-3.3765261879658,
-2.43572396492932));
#49556=CARTESIAN_POINT('Ctrl Pts',(-5.40384490325929E-15,-3.35286567774219,
-2.47568058755071));
#49557=CARTESIAN_POINT('Ctrl Pts',(-3.07309964203322E-15,-3.3284931802157,
-2.51525250052437));
#49558=CARTESIAN_POINT('Ctrl Pts',(-2.55351295663786E-15,-3.30342567080822,
-2.55442929399667));
#49559=CARTESIAN_POINT('Ctrl Pts',(-2.21585161566373E-15,-3.28713516706875,
-2.57988893141763));
#49560=CARTESIAN_POINT('Ctrl Pts',(-1.73369067459434E-14,-3.27054786797816,
-2.60518633230089));
#49561=CARTESIAN_POINT('Ctrl Pts',(-1.69309011255336E-14,-3.25368678771015,
-2.63029154815235));
#49562=CARTESIAN_POINT('Ctrl Pts',(-1.52366107287811E-14,-3.18332429778173,
-2.73505740356734));
#49563=CARTESIAN_POINT('Ctrl Pts',(-7.85431309872848E-15,-3.10815120519487,
-2.83655470454748));
#49564=CARTESIAN_POINT('Ctrl Pts',(-5.77315972805081E-15,-3.02856012624411,
-2.93460023723518));
#49565=CARTESIAN_POINT('Ctrl Pts',(-3.65120770442108E-15,-2.94740875440291,
-3.03456784146166));
#49566=CARTESIAN_POINT('Ctrl Pts',(-1.10974998716751E-14,-2.86166412082263,
-3.13094761193651));
#49567=CARTESIAN_POINT('Ctrl Pts',(-1.03805852802452E-14,-2.77169173795742,
-3.2235279094873));
#49568=CARTESIAN_POINT('Ctrl Pts',(-1.00669351464947E-14,-2.73232882045389,
-3.26403178966576));
#49569=CARTESIAN_POINT('Ctrl Pts',(1.1368289068979E-15,-2.69215607320333,
-3.30380815052698));
#49570=CARTESIAN_POINT('Ctrl Pts',(1.60982338570648E-15,-2.65120142765904,
-3.34283779060884));
#49571=CARTESIAN_POINT('Ctrl Pts',(1.85310027956541E-15,-2.63013708250599,
-3.36291204101334));
#49572=CARTESIAN_POINT('Ctrl Pts',(-2.39183766274509E-15,-2.60886587002882,
-3.38278873840918));
#49573=CARTESIAN_POINT('Ctrl Pts',(-1.77635683940025E-15,-2.58739143950339,
-3.40246515988401));
#49574=CARTESIAN_POINT('Ctrl Pts',(-1.21194577917492E-15,-2.56769885828742,
-3.42050892255673));
#49575=CARTESIAN_POINT('Ctrl Pts',(3.20395462986166E-15,-2.54783172387995,
-3.43838737529476));
#49576=CARTESIAN_POINT('Ctrl Pts',(2.72004641033163E-15,-2.52781546097606,
-3.45607868380752));
#49577=CARTESIAN_POINT('Ctrl Pts',(3.24874263539825E-16,-2.42874213786364,
-3.54364431646243));
#49578=CARTESIAN_POINT('Ctrl Pts',(-1.42112367967504E-14,-2.32592759453929,
-3.6267135247425));
#49579=CARTESIAN_POINT('Ctrl Pts',(-1.0991207943789E-14,-2.21978207787836,
-3.70509096548934));
#49580=CARTESIAN_POINT('Ctrl Pts',(-7.72550104896222E-15,-2.11213082335754,
-3.78458023727349));
#49581=CARTESIAN_POINT('Ctrl Pts',(3.10559049872635E-15,-2.00105292688667,
-3.85924433374753));
#49582=CARTESIAN_POINT('Ctrl Pts',(2.60902410786912E-15,-1.88692876195011,
-3.9288546438315));
#49583=CARTESIAN_POINT('Ctrl Pts',(2.11296027189519E-15,-1.77292009749333,
-3.99839450411882));
#49584=CARTESIAN_POINT('Ctrl Pts',(-1.19023239270618E-14,-1.65587069894074,
-4.06289140983169));
#49585=CARTESIAN_POINT('Ctrl Pts',(-1.44884104713583E-14,-1.53612127914559,
-4.12208347067618));
#49586=CARTESIAN_POINT('Ctrl Pts',(-1.63872008747819E-14,-1.44819728850264,
-4.16554424245053));
#49587=CARTESIAN_POINT('Ctrl Pts',(1.48322560200536E-15,-1.358816881025,
-4.20614452293028));
#49588=CARTESIAN_POINT('Ctrl Pts',(1.77635683940025E-15,-1.26810467560363,
-4.24376604966189));
#49589=CARTESIAN_POINT('Ctrl Pts',(1.89986052924058E-15,-1.22988530266112,
-4.25961696139028));
#49590=CARTESIAN_POINT('Ctrl Pts',(-6.83825980710587E-15,-1.19142942418558,
-4.27493893402116));
#49591=CARTESIAN_POINT('Ctrl Pts',(-6.77236045021345E-15,-1.15274600094195,
-4.28972236344086));
#49592=CARTESIAN_POINT('Ctrl Pts',(-6.73168489219131E-15,-1.1288691393026,
-4.29884725129232));
#49593=CARTESIAN_POINT('Ctrl Pts',(-6.80830697204428E-15,-1.10490022885304,
-4.30776879683175));
#49594=CARTESIAN_POINT('Ctrl Pts',(-6.55031584528842E-15,-1.08087218884353,
-4.31647376695309));
#49595=CARTESIAN_POINT('Ctrl Pts',(-5.15864969987438E-15,-0.951259165936978,
-4.36343046801116));
#49596=CARTESIAN_POINT('Ctrl Pts',(-9.14651306628698E-15,-0.819788429412977,
-4.4041447952911));
#49597=CARTESIAN_POINT('Ctrl Pts',(-7.49400541621981E-15,-0.686853690194028,
-4.43838432887677));
#49598=CARTESIAN_POINT('Ctrl Pts',(-6.41519723636329E-15,-0.600069774821131,
-4.46073695696003));
#49599=CARTESIAN_POINT('Ctrl Pts',(3.08265417366316E-15,-0.512661063187981,
-4.48032944741841));
#49600=CARTESIAN_POINT('Ctrl Pts',(2.72004641033163E-15,-0.424729285070971,
-4.49708803736938));
#49601=CARTESIAN_POINT('Ctrl Pts',(2.21027954554588E-15,-0.294380989358742,
-4.52193063336172));
#49602=CARTESIAN_POINT('Ctrl Pts',(-6.11319286711368E-15,-0.162884046650897,
-4.54054853308582));
#49603=CARTESIAN_POINT('Ctrl Pts',(-6.85562717706034E-15,-0.0306517464005833,
-4.55312130983207));
#49604=CARTESIAN_POINT('Ctrl Pts',(-7.61000109133581E-15,0.103707073763108,
-4.5658962781765));
#49605=CARTESIAN_POINT('Ctrl Pts',(-1.63497112532693E-15,0.238825822812114,
-4.57243019189283));
#49606=CARTESIAN_POINT('Ctrl Pts',(-2.63677968348475E-15,0.374285930049112,
-4.57285970409636));
#49607=CARTESIAN_POINT('Ctrl Pts',(-3.1179292879162E-15,0.439344844232451,
-4.57306599064198));
#49608=CARTESIAN_POINT('Ctrl Pts',(-1.01815445406519E-14,0.504482649963796,
-4.57186341188294));
#49609=CARTESIAN_POINT('Ctrl Pts',(-1.13242748511766E-14,0.56965339169973,
-4.56926290729125));
#49610=CARTESIAN_POINT('Ctrl Pts',(-1.17607086462203E-14,0.594543528838534,
-4.56826971749176));
#49611=CARTESIAN_POINT('Ctrl Pts',(-1.64394877692331E-14,0.619443271976647,
-4.56707223758195));
#49612=CARTESIAN_POINT('Ctrl Pts',(-1.64868119156836E-14,0.644320150574942,
-4.56567290865878));
#49613=CARTESIAN_POINT('Ctrl Pts',(-1.6747057075368E-14,0.78112319360564,
-4.55797771273081));
#49614=CARTESIAN_POINT('Ctrl Pts',(-4.80959600169574E-15,0.917388398723616,
-4.5441785389719));
#49615=CARTESIAN_POINT('Ctrl Pts',(-3.30291349825984E-15,1.05267829205595,
-4.52449336420144));
#49616=CARTESIAN_POINT('Ctrl Pts',(-1.76031124497757E-15,1.19119353586137,
-4.50433888912928));
#49617=CARTESIAN_POINT('Ctrl Pts',(-9.24810924555582E-15,1.32868716814533,
-4.47801451299053));
#49618=CARTESIAN_POINT('Ctrl Pts',(-6.0507154842071E-15,1.46470504959221,
-4.44570106748648));
#49619=CARTESIAN_POINT('Ctrl Pts',(-2.89585376704057E-15,1.59891360789184,
-4.41381745859138));
#49620=CARTESIAN_POINT('Ctrl Pts',(-2.10645447082242E-15,1.73168624049081,
-4.37610283665406));
#49621=CARTESIAN_POINT('Ctrl Pts',(-1.09634523681734E-15,1.862589475375,
-4.33268125614708));
#49622=CARTESIAN_POINT('Ctrl Pts',(-3.74816430711647E-16,1.9581841340492,
-4.30097179402927));
#49623=CARTESIAN_POINT('Ctrl Pts',(3.02205267408009E-15,2.05278195326171,
-4.26621781290806));
#49624=CARTESIAN_POINT('Ctrl Pts',(4.16333634234434E-15,2.14626801492587,
-4.22848555519344));
#49625=CARTESIAN_POINT('Ctrl Pts',(4.68860356446466E-15,2.18929427148484,
-4.21111956745068));
#49626=CARTESIAN_POINT('Ctrl Pts',(1.11734467368341E-15,2.23208498079157,
-4.19312252578931));
#49627=CARTESIAN_POINT('Ctrl Pts',(1.17961196366423E-15,2.27462862144891,
-4.17449995562647));
#49628=CARTESIAN_POINT('Ctrl Pts',(1.21298692846241E-15,2.29743180607061,
-4.16451834852861));
#49629=CARTESIAN_POINT('Ctrl Pts',(2.69478357067603E-15,2.32016400623282,
-4.15435702299221));
#49630=CARTESIAN_POINT('Ctrl Pts',(2.692290834716E-15,2.34282341818224,
-4.14401676235655));
#49631=CARTESIAN_POINT('Ctrl Pts',(2.69032939972027E-15,2.36065321014296,
-4.13588042164457));
#49632=CARTESIAN_POINT('Ctrl Pts',(-1.13007804132127E-14,2.37843876952637,
-4.12763283650539));
#49633=CARTESIAN_POINT('Ctrl Pts',(-1.09495745803656E-14,2.39616405253862,
-4.11928169694977));
#49634=CARTESIAN_POINT('Ctrl Pts',(-8.39698482786046E-15,2.52499270954159,
-4.05858500214088));
#49635=CARTESIAN_POINT('Ctrl Pts',(1.60026416366889E-15,2.6508256133944,
-3.99233766103874));
#49636=CARTESIAN_POINT('Ctrl Pts',(1.87350135405495E-15,2.77336570632561,
-3.92081240446126));
#49637=CARTESIAN_POINT('Ctrl Pts',(2.15041244287694E-15,2.89755345144912,
-3.84832543206502));
#49638=CARTESIAN_POINT('Ctrl Pts',(-2.86602714926484E-15,3.01835993446049,
-3.77041749676129));
#49639=CARTESIAN_POINT('Ctrl Pts',(-2.33146835171283E-15,3.13546816361818,
-3.68731987875136));
#49640=CARTESIAN_POINT('Ctrl Pts',(-1.79739883395837E-15,3.25246920402336,
-3.60429831970052));
#49641=CARTESIAN_POINT('Ctrl Pts',(-1.49727946848197E-15,3.3657794534396,
-3.51609628762174));
#49642=CARTESIAN_POINT('Ctrl Pts',(-1.44675937896466E-15,3.47506462955744,
-3.42289583527326));
#49643=CARTESIAN_POINT('Ctrl Pts',(-1.39690296057887E-15,3.5829141507272,
-3.33091973644948));
#49644=CARTESIAN_POINT('Ctrl Pts',(7.97356274507999E-15,3.68684428184482,
-3.23407532274603));
#49645=CARTESIAN_POINT('Ctrl Pts',(8.63198401646059E-15,3.786506317757,
-3.13249514891036));
#49646=CARTESIAN_POINT('Ctrl Pts',(8.82826822414374E-15,3.81621690671488,
-3.10221273732326));
#49647=CARTESIAN_POINT('Ctrl Pts',(4.28211893531462E-15,3.84554796150488,
-3.07150918131398));
#49648=CARTESIAN_POINT('Ctrl Pts',(4.44089209850063E-15,3.87448963569911,
-3.0403873211912));
#49649=CARTESIAN_POINT('Ctrl Pts',(4.44089209850063E-15,3.87448963569911,
-3.0403873211912));
#49650=CARTESIAN_POINT('Ctrl Pts',(-0.039772944186534,3.3679595299544,-3.68587930545212));
#49651=CARTESIAN_POINT('Ctrl Pts',(-0.0795458883730713,2.69823621289534,
-4.19688248983334));
#49652=CARTESIAN_POINT('Ctrl Pts',(-0.11931883255961,1.94417218263051,-4.52245569180505));
#49653=CARTESIAN_POINT('Ctrl Pts',(-0.159091776746148,1.19010815236569,
-4.84802889377675));
#49654=CARTESIAN_POINT('Ctrl Pts',(-0.198864720932685,0.351703408895132,
-4.98817211333893));
#49655=CARTESIAN_POINT('Ctrl Pts',(-0.238637665119224,-0.463640495906287,
-4.90908491848449));
#49656=CARTESIAN_POINT('Ctrl Pts',(-0.318183553492298,-2.09432830550906,
-4.75091052877563));
#49657=CARTESIAN_POINT('Ctrl Pts',(-0.397729441865374,-3.63277276043523,
-3.71581448140035));
#49658=CARTESIAN_POINT('Ctrl Pts',(-0.477275330238448,-4.38170539133441,
-2.26639967267857));
#49659=CARTESIAN_POINT('Ctrl Pts',(-0.515236378191096,-4.7391125194254,
-1.57470703862169));
#49660=CARTESIAN_POINT('Ctrl Pts',(-0.553197426143743,-4.91671556355819,
-0.788657102896253));
#49661=CARTESIAN_POINT('Ctrl Pts',(-0.591158474096391,-4.91617236260859,
-0.00191614214703012));
#49662=CARTESIAN_POINT('Origin',(5.68856688596016,0.,0.));
#49663=CARTESIAN_POINT('',(5.45515903851997,8.,-4.61880215351701));
#49664=CARTESIAN_POINT('',(5.45515903851997,-1.69692038195985E-15,-9.23760430703401));
#49665=CARTESIAN_POINT('Ctrl Pts',(5.45515903851997,8.,-4.61880215351701));
#49666=CARTESIAN_POINT('Ctrl Pts',(6.79005121159811,3.99999999999974,-6.92820323027566));
#49667=CARTESIAN_POINT('Ctrl Pts',(5.45515903851997,-1.69692038195985E-15,
-9.23760430703401));
#49668=CARTESIAN_POINT('',(5.45515903851997,8.,4.61880215351701));
#49669=CARTESIAN_POINT('Ctrl Pts',(5.45515903851997,8.,4.61880215351701));
#49670=CARTESIAN_POINT('Ctrl Pts',(6.79005121159811,8.,-3.04201108747293E-13));
#49671=CARTESIAN_POINT('Ctrl Pts',(5.45515903851997,8.,-4.61880215351701));
#49672=CARTESIAN_POINT('',(5.45515903851997,5.6564012731995E-16,9.23760430703401));
#49673=CARTESIAN_POINT('Ctrl Pts',(5.45515903851998,5.6564012731995E-16,
9.23760430703401));
#49674=CARTESIAN_POINT('Ctrl Pts',(6.79005121159811,4.00000000000026,6.92820323027536));
#49675=CARTESIAN_POINT('Ctrl Pts',(5.45515903851998,8.,4.61880215351701));
#49676=CARTESIAN_POINT('',(5.45515903851997,-8.,4.61880215351701));
#49677=CARTESIAN_POINT('Ctrl Pts',(5.45515903851997,-8.,4.61880215351701));
#49678=CARTESIAN_POINT('Ctrl Pts',(6.79005121159811,-3.99999999999974,6.92820323027566));
#49679=CARTESIAN_POINT('Ctrl Pts',(5.45515903851997,5.6564012731995E-16,
9.23760430703401));
#49680=CARTESIAN_POINT('',(6.17052559803778,-8.,-9.768626072022E-16));
#49681=CARTESIAN_POINT('Ctrl Pts',(6.17052559803778,-8.,-9.74007775086518E-16));
#49682=CARTESIAN_POINT('Ctrl Pts',(6.17052559803781,-8.,2.14359353944912));
#49683=CARTESIAN_POINT('Ctrl Pts',(5.45515903851997,-8.,4.61880215351701));
#49684=CARTESIAN_POINT('',(6.4,-7.60300281800529,-9.31099306497848E-16));
#49685=CARTESIAN_POINT('',(5.68856688596016,-8.83380215351701,-1.08182875316056E-15));
#49686=CARTESIAN_POINT('Origin',(6.4,0.,0.));
#49687=CARTESIAN_POINT('',(5.45515903851997,-8.,-4.61880215351701));
#49688=CARTESIAN_POINT('Ctrl Pts',(5.45515903851997,-8.,-4.61880215351701));
#49689=CARTESIAN_POINT('Ctrl Pts',(6.17052559803775,-8.,-2.14359353944897));
#49690=CARTESIAN_POINT('Ctrl Pts',(6.17052559803778,-8.,-9.74007775086518E-16));
#49691=CARTESIAN_POINT('Ctrl Pts',(5.45515903851997,-1.69692038195985E-15,
-9.23760430703401));
#49692=CARTESIAN_POINT('Ctrl Pts',(6.79005121159811,-4.00000000000026,-6.92820323027536));
#49693=CARTESIAN_POINT('Ctrl Pts',(5.45515903851997,-8.,-4.61880215351701));
#49694=CARTESIAN_POINT('Origin',(0.,5.6564012731995E-16,9.23760430703401));
#49695=CARTESIAN_POINT('',(0.,5.6564012731995E-16,9.23760430703401));
#49696=CARTESIAN_POINT('',(0.,5.6564012731995E-16,9.23760430703401));
#49697=CARTESIAN_POINT('',(0.,-8.,4.61880215351701));
#49698=CARTESIAN_POINT('',(0.,5.6564012731995E-16,9.23760430703401));
#49699=CARTESIAN_POINT('',(0.,-8.,4.61880215351701));
#49700=CARTESIAN_POINT('Origin',(0.,8.,4.61880215351701));
#49701=CARTESIAN_POINT('',(0.,8.,4.61880215351701));
#49702=CARTESIAN_POINT('',(0.,8.,4.61880215351701));
#49703=CARTESIAN_POINT('',(0.,8.,4.61880215351701));
#49704=CARTESIAN_POINT('Origin',(0.,8.,-4.61880215351701));
#49705=CARTESIAN_POINT('',(0.,8.,-4.61880215351701));
#49706=CARTESIAN_POINT('',(0.,8.,-4.61880215351701));
#49707=CARTESIAN_POINT('',(0.,8.,-4.61880215351701));
#49708=CARTESIAN_POINT('Origin',(0.,0.,0.));
#49709=CARTESIAN_POINT('',(0.,-1.69692038195985E-15,-9.23760430703401));
#49710=CARTESIAN_POINT('',(0.,-1.69692038195985E-15,-9.23760430703401));
#49711=CARTESIAN_POINT('',(0.,-8.,-4.61880215351701));
#49712=CARTESIAN_POINT('',(0.,-8.,-4.61880215351701));
#49713=CARTESIAN_POINT('',(0.,-8.,4.61880215351701));
#49714=CARTESIAN_POINT('Origin',(0.,0.,0.));
#49715=CARTESIAN_POINT('Origin',(0.,-1.69692038195985E-15,-9.23760430703401));
#49716=CARTESIAN_POINT('',(0.,-1.69692038195985E-15,-9.23760430703401));
#49717=CARTESIAN_POINT('Origin',(0.,-8.,-4.61880215351701));
#49718=CARTESIAN_POINT('',(0.,-8.,-4.61880215351701));
#49719=CARTESIAN_POINT('Origin',(0.,-8.,4.61880215351701));
#49720=CARTESIAN_POINT('Origin',(6.4,0.,0.));
#49721=CARTESIAN_POINT('Origin',(-30.,4.5,0.));
#49722=CARTESIAN_POINT('',(-30.,-4.5,-5.51091059616309E-16));
#49723=CARTESIAN_POINT('Origin',(-30.,0.,0.));
#49724=CARTESIAN_POINT('Origin',(-29.75,0.,0.));
#49725=CARTESIAN_POINT('',(-29.75,-4.75,-5.81707229594993E-16));
#49726=CARTESIAN_POINT('Origin',(-14.75,0.,0.));
#49727=CARTESIAN_POINT('',(0.,0.,0.));
#49728=CARTESIAN_POINT('Origin',(-14.75,0.,0.));
#49729=CARTESIAN_POINT('',(-29.0911584740964,-4.93085069296601,0.00239406595250471));
#49730=CARTESIAN_POINT('',(-29.3088415259036,-4.92746336814012,0.00144215323830204));
#49731=CARTESIAN_POINT('',(-14.75,-4.925,-6.03138548580071E-16));
#49732=CARTESIAN_POINT('',(-29.575,2.17167188636589,4.42425492889053));
#49733=CARTESIAN_POINT('Ctrl Pts',(-29.0911584740964,-4.93085069296601,
0.00239406595250471));
#49734=CARTESIAN_POINT('Ctrl Pts',(-29.0987040309128,-4.93188800524103,
0.15750466532186));
#49735=CARTESIAN_POINT('Ctrl Pts',(-29.1062495877292,-4.92523207312776,
0.312531807375031));
#49736=CARTESIAN_POINT('Ctrl Pts',(-29.1137951445456,-4.91059689710246,
0.466805765893802));
#49737=CARTESIAN_POINT('Ctrl Pts',(-29.1933410329187,-4.75631165258633,
2.09317468495417));
#49738=CARTESIAN_POINT('Ctrl Pts',(-29.2728869212918,-3.71524898717827,
3.63583816030893));
#49739=CARTESIAN_POINT('Ctrl Pts',(-29.3524328096649,-2.26290809811278,
4.38440317990658));
#49740=CARTESIAN_POINT('Ctrl Pts',(-29.4266218731099,-0.908371583825934,
5.08255790377123));
#49741=CARTESIAN_POINT('Ctrl Pts',(-29.5008109365549,0.803915241080997,
5.08996618673832));
#49742=CARTESIAN_POINT('Ctrl Pts',(-29.575,2.17494790042119,4.42655504786424));
#49743=CARTESIAN_POINT('',(-29.575,-2.1683958723106,4.4219548099168));
#49744=CARTESIAN_POINT('Origin',(-29.575,0.,0.));
#49745=CARTESIAN_POINT('Ctrl Pts',(-29.575,-2.16839587231058,4.42195480991681));
#49746=CARTESIAN_POINT('Ctrl Pts',(-29.5352270558135,-2.90509583874374,
4.0606989321402));
#49747=CARTESIAN_POINT('Ctrl Pts',(-29.4954541116269,-3.54417075123437,
3.51185369356184));
#49748=CARTESIAN_POINT('Ctrl Pts',(-29.4556811674404,-4.01940836209596,
2.8419582808667));
#49749=CARTESIAN_POINT('Ctrl Pts',(-29.4159082232539,-4.49464597295758,
2.17206286817154));
#49750=CARTESIAN_POINT('Ctrl Pts',(-29.3761352790673,-4.80604628219013,
1.38111728135961));
#49751=CARTESIAN_POINT('Ctrl Pts',(-29.3363623348808,-4.89820932110733,
0.567147712221922));
#49752=CARTESIAN_POINT('Ctrl Pts',(-29.3271887318884,-4.91946666443181,
0.379406175157601));
#49753=CARTESIAN_POINT('Ctrl Pts',(-29.318015128896,-4.929060779183,0.190439782628943));
#49754=CARTESIAN_POINT('Ctrl Pts',(-29.3088415259036,-4.92746336814012,
0.00144215323830204));
#49755=CARTESIAN_POINT('Origin',(-14.75,0.,0.));
#49756=CARTESIAN_POINT('',(-27.5911584740964,-4.91871916148224,0.00298870709768639));
#49757=CARTESIAN_POINT('',(-27.8088415259036,-4.91810465358294,0.00250400581179228));
#49758=CARTESIAN_POINT('',(-14.75,-4.925,-6.03138548580071E-16));
#49759=CARTESIAN_POINT('Ctrl Pts',(-27.5911584740964,-4.91871916148224,
0.00298870709768639));
#49760=CARTESIAN_POINT('Ctrl Pts',(-27.6214287006744,-4.92217786568793,
0.629288456904983));
#49761=CARTESIAN_POINT('Ctrl Pts',(-27.6516989272523,-4.81132058056506,
1.2544097760338));
#49762=CARTESIAN_POINT('Ctrl Pts',(-27.6819691538303,-4.58053680634953,
1.83157791678433));
#49763=CARTESIAN_POINT('Ctrl Pts',(-27.7615150422034,-3.97406958038444,
3.34829442957306));
#49764=CARTESIAN_POINT('Ctrl Pts',(-27.8410609305764,-2.53943282222183,
4.53386340685575));
#49765=CARTESIAN_POINT('Ctrl Pts',(-27.9206068189495,-0.935593024822473,
4.84364324705812));
#49766=CARTESIAN_POINT('Ctrl Pts',(-28.0001527073226,0.668246772576907,
5.1534230872605));
#49767=CARTESIAN_POINT('Ctrl Pts',(-28.0796985956957,2.44128960921305,4.58741379038254));
#49768=CARTESIAN_POINT('Ctrl Pts',(-28.1592444840688,3.56896084480546,3.40568511210877));
#49769=CARTESIAN_POINT('Ctrl Pts',(-28.2387903724418,4.69663208039786,2.22395643383501));
#49770=CARTESIAN_POINT('Ctrl Pts',(-28.3183362608148,5.17893171494654,0.426508374165463));
#49771=CARTESIAN_POINT('Ctrl Pts',(-28.3978821491879,4.79450650284291,-1.16110247139908));
#49772=CARTESIAN_POINT('Ctrl Pts',(-28.477428037561,4.41008129073928,-2.74871331696362));
#49773=CARTESIAN_POINT('Ctrl Pts',(-28.5569739259341,3.15893123198334,-4.12648694842314));
#49774=CARTESIAN_POINT('Ctrl Pts',(-28.6365198143072,1.61540970892298,-4.66128231395555));
#49775=CARTESIAN_POINT('Ctrl Pts',(-28.7160657026803,0.0718881858626222,
-5.19607767948796));
#49776=CARTESIAN_POINT('Ctrl Pts',(-28.7956115910533,-1.76400480150215,
-4.88789477909325));
#49777=CARTESIAN_POINT('Ctrl Pts',(-28.8751574794264,-3.04819738337245,
-3.87876614751291));
#49778=CARTESIAN_POINT('Ctrl Pts',(-28.9471578109831,-4.21057413933529,
-2.96536135006638));
#49779=CARTESIAN_POINT('Ctrl Pts',(-29.0191581425397,-4.92095257284757,
-1.4776841912631));
#49780=CARTESIAN_POINT('Ctrl Pts',(-29.0911584740964,-4.93085069296601,
0.00239406595250471));
#49781=CARTESIAN_POINT('Ctrl Pts',(-29.3088415259036,-4.92746336814012,
0.00144215323830204));
#49782=CARTESIAN_POINT('Ctrl Pts',(-29.2384692405229,-4.91520935345547,
-1.44839114811431));
#49783=CARTESIAN_POINT('Ctrl Pts',(-29.1680969551423,-4.24436898433528,
-2.90006264127696));
#49784=CARTESIAN_POINT('Ctrl Pts',(-29.0977246697616,-3.12788046011008,
-3.81474362504512));
#49785=CARTESIAN_POINT('Ctrl Pts',(-29.0181787813885,-1.86584852470544,
-4.8486607564584));
#49786=CARTESIAN_POINT('Ctrl Pts',(-28.9386328930154,-0.0344076573231608,
-5.19645995170656));
#49787=CARTESIAN_POINT('Ctrl Pts',(-28.8590870046423,1.52027960945058,-4.69387792027941));
#49788=CARTESIAN_POINT('Ctrl Pts',(-28.7795411162692,3.07496687622432,-4.19129588885225));
#49789=CARTESIAN_POINT('Ctrl Pts',(-28.6999952278962,4.35290054238952,-2.83833263074978));
#49790=CARTESIAN_POINT('Ctrl Pts',(-28.6204493395231,4.76944898889192,-1.25865959225591));
#49791=CARTESIAN_POINT('Ctrl Pts',(-28.54090345115,5.18599743539432,0.321013446237961));
#49792=CARTESIAN_POINT('Ctrl Pts',(-28.4613575627769,4.74116066223391,2.12739626512323));
#49793=CARTESIAN_POINT('Ctrl Pts',(-28.3818116744039,3.63804206657526,3.33181334358779));
#49794=CARTESIAN_POINT('Ctrl Pts',(-28.3022657860308,2.53492347091661,4.53623042205235));
#49795=CARTESIAN_POINT('Ctrl Pts',(-28.2227198976577,0.773523052759708,
5.13868176009622));
#49796=CARTESIAN_POINT('Ctrl Pts',(-28.1431740092847,-0.836391940911384,
4.8618460820682));
#49797=CARTESIAN_POINT('Ctrl Pts',(-28.0636281209116,-2.44630693458247,
4.58501040404019));
#49798=CARTESIAN_POINT('Ctrl Pts',(-27.9840822325385,-3.90473650376776,
3.42888770994031));
#49799=CARTESIAN_POINT('Ctrl Pts',(-27.9045363441654,-4.54206616433802,
1.92485926408358));
#49800=CARTESIAN_POINT('Ctrl Pts',(-27.8726380714115,-4.79763833485293,
1.32173683278195));
#49801=CARTESIAN_POINT('Ctrl Pts',(-27.8407397986575,-4.92117374333981,
0.662669505529257));
#49802=CARTESIAN_POINT('Ctrl Pts',(-27.8088415259036,-4.91810465358294,
0.00250400581179228));
#49803=CARTESIAN_POINT('Origin',(-14.75,0.,0.));
#49804=CARTESIAN_POINT('',(-26.0911584740964,-4.92036739665688,-0.00383377046079936));
#49805=CARTESIAN_POINT('',(-26.3088415259036,-4.92121007081632,-0.00410983607026229));
#49806=CARTESIAN_POINT('',(-14.75,-4.925,-6.03138548580071E-16));
#49807=CARTESIAN_POINT('Ctrl Pts',(-26.0911584740964,-4.92036739665688,
-0.00383377046079936));
#49808=CARTESIAN_POINT('Ctrl Pts',(-26.1441533704359,-4.91244432033151,
1.09173065983813));
#49809=CARTESIAN_POINT('Ctrl Pts',(-26.1971482667754,-4.55141276587038,
2.19203324705585));
#49810=CARTESIAN_POINT('Ctrl Pts',(-26.2501431631149,-3.87908362999679,
3.04775276608836));
#49811=CARTESIAN_POINT('Ctrl Pts',(-26.329689051488,-2.86991063247732,4.33219662844735));
#49812=CARTESIAN_POINT('Ctrl Pts',(-26.4092349398611,-1.15937419217738,
5.06558698769252));
#49813=CARTESIAN_POINT('Ctrl Pts',(-26.4887808282342,0.466768297211532,
4.91103020168458));
#49814=CARTESIAN_POINT('Ctrl Pts',(-26.5683267166072,2.09291078660044,4.75647341567663));
#49815=CARTESIAN_POINT('Ctrl Pts',(-26.6478726049803,3.63465932507832,3.71396948441558));
#49816=CARTESIAN_POINT('Ctrl Pts',(-26.7274184933534,4.38378843538607,2.26240825335668));
#49817=CARTESIAN_POINT('Ctrl Pts',(-26.8069643817264,5.13291754569381,0.810847022297775));
#49818=CARTESIAN_POINT('Ctrl Pts',(-26.8865102700995,5.08942722783144,-1.04977150855898));
#49819=CARTESIAN_POINT('Ctrl Pts',(-26.9660561584726,4.27329930907013,-2.46474911465105));
#49820=CARTESIAN_POINT('Ctrl Pts',(-27.0456020468457,3.45717139030882,-3.87972672074312));
#49821=CARTESIAN_POINT('Ctrl Pts',(-27.1251479352187,1.86840587064857,-4.84906340207051));
#49822=CARTESIAN_POINT('Ctrl Pts',(-27.2046938235918,0.236816482345431,
-4.92747617760022));
#49823=CARTESIAN_POINT('Ctrl Pts',(-27.2842397119649,-1.39477290595772,
-5.00588895312993));
#49824=CARTESIAN_POINT('Ctrl Pts',(-27.363785600338,-3.06918616290375,-4.19337782286196));
#49825=CARTESIAN_POINT('Ctrl Pts',(-27.4433314887111,-4.01724394449298,
-2.86319023358059));
#49826=CARTESIAN_POINT('Ctrl Pts',(-27.4926071505062,-4.60452979374673,
-2.03918945724775));
#49827=CARTESIAN_POINT('Ctrl Pts',(-27.5418828123013,-4.91308887859519,
-1.01653899859688));
#49828=CARTESIAN_POINT('Ctrl Pts',(-27.5911584740964,-4.91871916148224,
0.00298870709768639));
#49829=CARTESIAN_POINT('Ctrl Pts',(-27.8088415259036,-4.91810465358294,
0.00250400581179228));
#49830=CARTESIAN_POINT('Ctrl Pts',(-27.7611939102845,-4.91352024206437,
-0.983609324467926));
#49831=CARTESIAN_POINT('Ctrl Pts',(-27.7135462946653,-4.62644968879859,
-1.97217295080227));
#49832=CARTESIAN_POINT('Ctrl Pts',(-27.6658986790462,-4.07499817460332,
-2.78038834104901));
#49833=CARTESIAN_POINT('Ctrl Pts',(-27.5863527906731,-3.15437077234312,
-4.12967330271128));
#49834=CARTESIAN_POINT('Ctrl Pts',(-27.5068069023,-1.49688621586748,-4.97630902842222));
#49835=CARTESIAN_POINT('Ctrl Pts',(-27.427261013927,0.135976152639213,-4.93130021039854));
#49836=CARTESIAN_POINT('Ctrl Pts',(-27.3477151255539,1.7688385211459,-4.88629139237487));
#49837=CARTESIAN_POINT('Ctrl Pts',(-27.2681692371808,3.37707870168364,-3.9496380306166));
#49838=CARTESIAN_POINT('Ctrl Pts',(-27.1886233488077,4.22197683163389,-2.55164722242325));
#49839=CARTESIAN_POINT('Ctrl Pts',(-27.1090774604347,5.06687496158415,-1.1536564142299));
#49840=CARTESIAN_POINT('Ctrl Pts',(-27.0295315720616,5.14843104094691,0.705671840398515));
#49841=CARTESIAN_POINT('Ctrl Pts',(-26.9499856836885,4.42915646105591,2.17225163970649));
#49842=CARTESIAN_POINT('Ctrl Pts',(-26.8704397953154,3.7098818811649,3.63883143901446));
#49843=CARTESIAN_POINT('Ctrl Pts',(-26.7908939069423,2.18977664202013,4.71266278300198));
#49844=CARTESIAN_POINT('Ctrl Pts',(-26.7113480185693,0.567134884896936,
4.90045492678425));
#49845=CARTESIAN_POINT('Ctrl Pts',(-26.6318021301962,-1.05550687222627,
5.08824707056651));
#49846=CARTESIAN_POINT('Ctrl Pts',(-26.5522562418232,-2.7806851473279,4.39000001414349));
#49847=CARTESIAN_POINT('Ctrl Pts',(-26.4727103534501,-3.81592225162572,
3.12646916519825));
#49848=CARTESIAN_POINT('Ctrl Pts',(-26.4180874109346,-4.52680370627415,
2.25882189467213));
#49849=CARTESIAN_POINT('Ctrl Pts',(-26.3634644684191,-4.91235316928586,
1.12462305447093));
#49850=CARTESIAN_POINT('Ctrl Pts',(-26.3088415259036,-4.92121007081632,
-0.00410983607026228));
#49851=CARTESIAN_POINT('Origin',(-14.75,0.,0.));
#49852=CARTESIAN_POINT('',(-24.5911584740964,-4.93264761214373,-0.00145024765580815));
#49853=CARTESIAN_POINT('',(-24.8088415259036,-4.93298564037245,-0.000844910194652536));
#49854=CARTESIAN_POINT('',(-14.75,-4.925,-6.03138548580071E-16));
#49855=CARTESIAN_POINT('Ctrl Pts',(-24.5911584740964,-4.93264761214373,
-0.00145024765580815));
#49856=CARTESIAN_POINT('Ctrl Pts',(-24.6668780401975,-4.9266177416151,1.55388178409041));
#49857=CARTESIAN_POINT('Ctrl Pts',(-24.7425976062985,-4.12958481778531,
3.11453421006534));
#49858=CARTESIAN_POINT('Ctrl Pts',(-24.8183171723996,-2.86343383037207,
4.01706799645064));
#49859=CARTESIAN_POINT('Ctrl Pts',(-24.8978630607726,-1.53330067860747,
4.96520934909558));
#49860=CARTESIAN_POINT('Ctrl Pts',(-24.9774089491457,0.314560165826125,
5.18703834835445));
#49861=CARTESIAN_POINT('Ctrl Pts',(-25.0569548375188,1.83130840270388,4.58065477546433));
#49862=CARTESIAN_POINT('Ctrl Pts',(-25.1365007258919,3.34805663958163,3.9742712025742));
#49863=CARTESIAN_POINT('Ctrl Pts',(-25.2160466142649,4.53369226890353,2.5396750575351));
#49864=CARTESIAN_POINT('Ctrl Pts',(-25.295592502638,4.84357719847932,0.935867858373788));
#49865=CARTESIAN_POINT('Ctrl Pts',(-25.3751383910111,5.15346212805511,-0.667939340787529));
#49866=CARTESIAN_POINT('Ctrl Pts',(-25.4546842793842,4.58759635788477,-2.44095759407106));
#49867=CARTESIAN_POINT('Ctrl Pts',(-25.5342301677572,3.40591819971526,-3.56872660483793));
#49868=CARTESIAN_POINT('Ctrl Pts',(-25.6137760561303,2.22424004154574,-4.69649561560481));
#49869=CARTESIAN_POINT('Ctrl Pts',(-25.6933219445034,0.426749495377071,
-5.17901538385504));
#49870=CARTESIAN_POINT('Ctrl Pts',(-25.7728678328765,-1.16085155874105,
-4.79463371383198));
#49871=CARTESIAN_POINT('Ctrl Pts',(-25.8524137212495,-2.74845261285917,
-4.41025204380892));
#49872=CARTESIAN_POINT('Ctrl Pts',(-25.9319596096226,-4.12616417492674,
-3.15896893551255));
#49873=CARTESIAN_POINT('Ctrl Pts',(-26.0115054979957,-4.661115178591,-1.61557869862796));
#49874=CARTESIAN_POINT('Ctrl Pts',(-26.0380564900293,-4.83967223700271,
-1.10042269594398));
#49875=CARTESIAN_POINT('Ctrl Pts',(-26.0646074820628,-4.92433693997005,
-0.552722898855101));
#49876=CARTESIAN_POINT('Ctrl Pts',(-26.0911584740964,-4.92036739665688,
-0.00383377046079936));
#49877=CARTESIAN_POINT('Ctrl Pts',(-26.3088415259036,-4.92121007081632,
-0.00410983607026228));
#49878=CARTESIAN_POINT('Ctrl Pts',(-26.283918580046,-4.92525123130941,-0.519119599791246));
#49879=CARTESIAN_POINT('Ctrl Pts',(-26.2589956341884,-4.85087080801869,
-1.03299143706225));
#49880=CARTESIAN_POINT('Ctrl Pts',(-26.2340726883308,-4.69319011704004,
-1.5198867036229));
#49881=CARTESIAN_POINT('Ctrl Pts',(-26.1545267999577,-4.18992494466251,
-3.07389708203135));
#49882=CARTESIAN_POINT('Ctrl Pts',(-26.0749809115847,-2.83809866641343,
-4.35310319738077));
#49883=CARTESIAN_POINT('Ctrl Pts',(-25.9954350232116,-1.25869311650182,
-4.76988247643117));
#49884=CARTESIAN_POINT('Ctrl Pts',(-25.9158891348386,0.320712433409791,
-5.18666175548156));
#49885=CARTESIAN_POINT('Ctrl Pts',(-25.8363432464654,2.12769725498392,-4.74101419823293));
#49886=CARTESIAN_POINT('Ctrl Pts',(-25.7567973580924,3.33219893892002,-3.63765499595275));
#49887=CARTESIAN_POINT('Ctrl Pts',(-25.6772514697193,4.53670062285612,-2.53429579367258));
#49888=CARTESIAN_POINT('Ctrl Pts',(-25.5977055813462,5.13871916915418,-0.773224946360884));
#49889=CARTESIAN_POINT('Ctrl Pts',(-25.5181596929732,4.86170857536212,0.836585847286859));
#49890=CARTESIAN_POINT('Ctrl Pts',(-25.4386138046001,4.58469798157006,2.44639664093459));
#49891=CARTESIAN_POINT('Ctrl Pts',(-25.359067916227,3.4286582476879,3.90494738091836));
#49892=CARTESIAN_POINT('Ctrl Pts',(-25.2795220278539,1.92463240018136,4.54223247168555));
#49893=CARTESIAN_POINT('Ctrl Pts',(-25.1999761394808,0.420606552674816,
5.17951756245273));
#49894=CARTESIAN_POINT('Ctrl Pts',(-25.1204302511078,-1.43140540845612,
4.99553700400332));
#49895=CARTESIAN_POINT('Ctrl Pts',(-25.0408843627347,-2.78065642310143,
4.07480491924754));
#49896=CARTESIAN_POINT('Ctrl Pts',(-24.9635367504577,-4.09262045392238,
3.17951756047544));
#49897=CARTESIAN_POINT('Ctrl Pts',(-24.8861891381806,-4.92922749371504,
1.58763673888852));
#49898=CARTESIAN_POINT('Ctrl Pts',(-24.8088415259036,-4.93298564037245,
-0.000844910194652536));
#49899=CARTESIAN_POINT('Origin',(-14.75,0.,0.));
#49900=CARTESIAN_POINT('',(-23.0911584740964,-4.92477578693879,0.00455121266192807));
#49901=CARTESIAN_POINT('',(-23.3088415259036,-4.92376359828451,0.00452755087589233));
#49902=CARTESIAN_POINT('',(-14.75,-4.925,-6.03138548580071E-16));
#49903=CARTESIAN_POINT('Ctrl Pts',(-23.0911584740964,-4.92477578693879,
0.00455121266192807));
#49904=CARTESIAN_POINT('Ctrl Pts',(-23.1100568215859,-4.92836778419939,
0.39435127717714));
#49905=CARTESIAN_POINT('Ctrl Pts',(-23.1289551690754,-4.88600126774917,
0.783379637951124));
#49906=CARTESIAN_POINT('Ctrl Pts',(-23.147853516565,-4.7947032911263,1.1605640760821));
#49907=CARTESIAN_POINT('Ctrl Pts',(-23.227399404938,-4.41041685226391,2.74818813835895));
#49908=CARTESIAN_POINT('Ctrl Pts',(-23.3069452933111,-3.15921646993337,
4.12597456962399));
#49909=CARTESIAN_POINT('Ctrl Pts',(-23.3864911816842,-1.6158582674624,4.66101820240316));
#49910=CARTESIAN_POINT('Ctrl Pts',(-23.4660370700573,-0.0725000649914348,
5.19606183518233));
#49911=CARTESIAN_POINT('Ctrl Pts',(-23.5455829584304,1.76301595761996,4.88836266947564));
#49912=CARTESIAN_POINT('Ctrl Pts',(-23.6251288468034,3.04752024302872,3.87926655341467));
#49913=CARTESIAN_POINT('Ctrl Pts',(-23.7046747351765,4.33202452843749,2.87017043735369));
#49914=CARTESIAN_POINT('Ctrl Pts',(-23.7842206235496,5.06551707664363,1.1596773709384));
#49915=CARTESIAN_POINT('Ctrl Pts',(-23.8637665119226,4.91105798552202,-0.46647410387683));
#49916=CARTESIAN_POINT('Ctrl Pts',(-23.9433124002957,4.75659889440041,-2.09262557869207));
#49917=CARTESIAN_POINT('Ctrl Pts',(-24.0228582886688,3.71418816395107,-3.63443546190725));
#49918=CARTESIAN_POINT('Ctrl Pts',(-24.1024041770419,2.26267151748941,-4.38365215585762));
#49919=CARTESIAN_POINT('Ctrl Pts',(-24.181950065415,0.811154871027751,-5.132868849808));
#49920=CARTESIAN_POINT('Ctrl Pts',(-24.261495953788,-1.04946769144621,-5.08949235449356));
#49921=CARTESIAN_POINT('Ctrl Pts',(-24.3410418421611,-2.4644935804178,-4.2734482583492));
#49922=CARTESIAN_POINT('Ctrl Pts',(-24.4205877305342,-3.87951946938938,
-3.45740416220484));
#49923=CARTESIAN_POINT('Ctrl Pts',(-24.5001336189073,-4.84894868485859,
-1.86869246523057));
#49924=CARTESIAN_POINT('Ctrl Pts',(-24.5796795072803,-4.92746056304542,
-0.237109763727941));
#49925=CARTESIAN_POINT('Ctrl Pts',(-24.5835058295524,-4.93123714728213,
-0.158627250588653));
#49926=CARTESIAN_POINT('Ctrl Pts',(-24.5873321518244,-4.93295231843154,
-0.0800455421075516));
#49927=CARTESIAN_POINT('Ctrl Pts',(-24.5911584740964,-4.93264761214373,
-0.00145024765580815));
#49928=CARTESIAN_POINT('Ctrl Pts',(-24.8088415259036,-4.93298564037245,
-0.000844910194652536));
#49929=CARTESIAN_POINT('Ctrl Pts',(-24.8066432498076,-4.93309244966778,
-0.0459907283445572));
#49930=CARTESIAN_POINT('Ctrl Pts',(-24.8044449737115,-4.93252653505162,
-0.0911338008527958));
#49931=CARTESIAN_POINT('Ctrl Pts',(-24.8022466976155,-4.93127968975541,
-0.136258058327248));
#49932=CARTESIAN_POINT('Ctrl Pts',(-24.7227008092424,-4.88616187360439,
-1.76910534008413));
#49933=CARTESIAN_POINT('Ctrl Pts',(-24.6431549208693,-3.94943617314267,
-3.37731629253574));
#49934=CARTESIAN_POINT('Ctrl Pts',(-24.5636090324963,-2.55140047284839,
-4.22213703896742));
#49935=CARTESIAN_POINT('Ctrl Pts',(-24.4840631441232,-1.15336477255412,
-5.06695778539909));
#49936=CARTESIAN_POINT('Ctrl Pts',(-24.4045172557501,0.705980927572705,
-5.14838832581082));
#49937=CARTESIAN_POINT('Ctrl Pts',(-24.324971367377,2.17252059826335,-4.42902243726831));
#49938=CARTESIAN_POINT('Ctrl Pts',(-24.2454254790039,3.63906026895399,-3.70965654872581));
#49939=CARTESIAN_POINT('Ctrl Pts',(-24.1658795906309,4.71279391020846,-2.18949423122905));
#49940=CARTESIAN_POINT('Ctrl Pts',(-24.0863337022578,4.90048718004666,-0.566842967216153));
#49941=CARTESIAN_POINT('Ctrl Pts',(-24.0067878138847,5.08818044988486,1.05580829679675));
#49942=CARTESIAN_POINT('Ctrl Pts',(-23.9272419255116,4.3898333483068,2.78094850732579));
#49943=CARTESIAN_POINT('Ctrl Pts',(-23.8476960371386,3.12624123694881,3.81611075100284));
#49944=CARTESIAN_POINT('Ctrl Pts',(-23.7681501487655,1.86264912559084,4.85127299467987));
#49945=CARTESIAN_POINT('Ctrl Pts',(-23.6886042603924,0.0338120044529563,
5.19645727150491));
#49946=CARTESIAN_POINT('Ctrl Pts',(-23.6090583720193,-1.52016861672953,
4.69309843356272));
#49947=CARTESIAN_POINT('Ctrl Pts',(-23.5295124836463,-3.07414923791204,
4.18973959562053));
#49948=CARTESIAN_POINT('Ctrl Pts',(-23.4499665952732,-4.35327335913915,
2.83783764291109));
#49949=CARTESIAN_POINT('Ctrl Pts',(-23.3704207069001,-4.76995770197036,
1.25840735017577));
#49950=CARTESIAN_POINT('Ctrl Pts',(-23.3498943132346,-4.8774808817366,0.850843758656771));
#49951=CARTESIAN_POINT('Ctrl Pts',(-23.3293679195691,-4.92757673294028,
0.428129724095519));
#49952=CARTESIAN_POINT('Ctrl Pts',(-23.3088415259036,-4.92376359828451,
0.00452755087589233));
#49953=CARTESIAN_POINT('Origin',(-14.75,0.,0.));
#49954=CARTESIAN_POINT('',(-21.5911584740964,-4.91693164693359,-0.000632398697534842));
#49955=CARTESIAN_POINT('',(-21.8088415259036,-4.91711569616659,-0.00117946379282014));
#49956=CARTESIAN_POINT('',(-14.75,-4.925,-6.03138548580071E-16));
#49957=CARTESIAN_POINT('Ctrl Pts',(-21.5911584740964,-4.91693164693359,
-0.000632398697534842));
#49958=CARTESIAN_POINT('Ctrl Pts',(-21.6327814913475,-4.91594750340395,
0.861347871439622));
#49959=CARTESIAN_POINT('Ctrl Pts',(-21.6744045085985,-4.70055318639053,
1.72378817794021));
#49960=CARTESIAN_POINT('Ctrl Pts',(-21.7160275258496,-4.27359604091789,
2.46423730661521));
#49961=CARTESIAN_POINT('Ctrl Pts',(-21.7955734142227,-3.4576368030521,3.87931212880427));
#49962=CARTESIAN_POINT('Ctrl Pts',(-21.8751193025958,-1.86898324578976,
4.84883661113057));
#49963=CARTESIAN_POINT('Ctrl Pts',(-21.9546651909688,-0.237405254457672,
4.92744633348781));
#49964=CARTESIAN_POINT('Ctrl Pts',(-22.0342110793419,1.39417273687441,5.00605605584506));
#49965=CARTESIAN_POINT('Ctrl Pts',(-22.113756967715,3.06867516227623,4.19375101823326));
#49966=CARTESIAN_POINT('Ctrl Pts',(-22.1933028560881,4.01689627682146,2.86367472410927));
#49967=CARTESIAN_POINT('Ctrl Pts',(-22.2728487444611,4.9651173913667,1.53359842998527));
#49968=CARTESIAN_POINT('Ctrl Pts',(-22.3523946328342,5.18705719505533,-0.314249120650923));
#49969=CARTESIAN_POINT('Ctrl Pts',(-22.4319405212073,4.58076458321006,-1.83103371282965));
#49970=CARTESIAN_POINT('Ctrl Pts',(-22.5114864095804,3.97447197136479,-3.34781830500836));
#49971=CARTESIAN_POINT('Ctrl Pts',(-22.5910322979534,2.53994694398564,-4.5335399387296));
#49972=CARTESIAN_POINT('Ctrl Pts',(-22.6705781863265,0.936158324065459,
-4.84352105564377));
#49973=CARTESIAN_POINT('Ctrl Pts',(-22.7501240746996,-0.667630295854733,
-5.15350217255794));
#49974=CARTESIAN_POINT('Ctrl Pts',(-22.8296699630727,-2.44068250831595,
-4.58774277266501));
#49975=CARTESIAN_POINT('Ctrl Pts',(-22.9092158514458,-3.56852236684944,
-3.40613222607422));
#49976=CARTESIAN_POINT('Ctrl Pts',(-22.9698633923293,-4.42841236656523,
-2.50524626705758));
#49977=CARTESIAN_POINT('Ctrl Pts',(-23.0305109332129,-4.9132485462191,-1.24637378817277));
#49978=CARTESIAN_POINT('Ctrl Pts',(-23.0911584740964,-4.92477578693879,
0.00455121266192807));
#49979=CARTESIAN_POINT('Ctrl Pts',(-23.3088415259036,-4.92376359828451,
0.00452755087589233));
#49980=CARTESIAN_POINT('Ctrl Pts',(-23.249822031196,-4.9127997005681,-1.2134548491438));
#49981=CARTESIAN_POINT('Ctrl Pts',(-23.1908025364885,-4.4561520233695,-2.43877979118426));
#49982=CARTESIAN_POINT('Ctrl Pts',(-23.1317830417809,-3.63745529283231,
-3.33241721991151));
#49983=CARTESIAN_POINT('Ctrl Pts',(-23.0522371534078,-2.53402397642775,
-4.53685286450225));
#49984=CARTESIAN_POINT('Ctrl Pts',(-22.9726912650347,-0.77291677918332,
-5.13876552092253));
#49985=CARTESIAN_POINT('Ctrl Pts',(-22.8931453766617,0.83687745995922,-4.86165832319329));
#49986=CARTESIAN_POINT('Ctrl Pts',(-22.8135994882886,2.44667169910178,-4.58455112546405));
#49987=CARTESIAN_POINT('Ctrl Pts',(-22.7340535999155,3.90515298014245,-3.42842407358526));
#49988=CARTESIAN_POINT('Ctrl Pts',(-22.6545077115424,4.5423478449547,-1.92436004709929));
#49989=CARTESIAN_POINT('Ctrl Pts',(-22.5749618231694,5.17954270976695,-0.42029602061334));
#49990=CARTESIAN_POINT('Ctrl Pts',(-22.4954159347963,4.9954511583508,1.43170498047977));
#49991=CARTESIAN_POINT('Ctrl Pts',(-22.4158700464232,4.07463817966522,2.78090079647325));
#49992=CARTESIAN_POINT('Ctrl Pts',(-22.3363241580501,3.15382520097963,4.13009661246674));
#49993=CARTESIAN_POINT('Ctrl Pts',(-22.2567782696771,1.4962907950246,4.97648724336059));
#49994=CARTESIAN_POINT('Ctrl Pts',(-22.177232381304,-0.136553786680188,
4.93127149915006));
#49995=CARTESIAN_POINT('Ctrl Pts',(-22.0976864929309,-1.76939836838497,
4.88605575493953));
#49996=CARTESIAN_POINT('Ctrl Pts',(-22.0181406045578,-3.37755312583951,
3.94923363562461));
#49997=CARTESIAN_POINT('Ctrl Pts',(-21.9385947161848,-4.22229002887781,
2.55114728056903));
#49998=CARTESIAN_POINT('Ctrl Pts',(-21.8953436527577,-4.68159433887712,
1.79097321179257));
#49999=CARTESIAN_POINT('Ctrl Pts',(-21.8520925893307,-4.91520443767987,
0.894432581458181));
#50000=CARTESIAN_POINT('Ctrl Pts',(-21.8088415259036,-4.91711569616659,
-0.00117946379282014));
#50001=CARTESIAN_POINT('Origin',(-14.75,0.,0.));
#50002=CARTESIAN_POINT('',(-20.0911584740964,-4.92710437571252,-0.00432825790191715));
#50003=CARTESIAN_POINT('',(-20.3088415259036,-4.92810468982102,-0.00410855472338207));
#50004=CARTESIAN_POINT('',(-14.75,-4.925,-6.03138548580071E-16));
#50005=CARTESIAN_POINT('Ctrl Pts',(-20.0911584740964,-4.92710437571252,
-0.00432825790191715));
#50006=CARTESIAN_POINT('Ctrl Pts',(-20.155506161109,-4.91490963574447,1.32130828947872));
#50007=CARTESIAN_POINT('Ctrl Pts',(-20.2198538481216,-4.36214110397647,
2.65590833175386));
#50008=CARTESIAN_POINT('Ctrl Pts',(-20.2842015351343,-3.40634621717809,
3.56831810142706));
#50009=CARTESIAN_POINT('Ctrl Pts',(-20.3637474235073,-2.22480330705116,
4.69622881676794));
#50010=CARTESIAN_POINT('Ctrl Pts',(-20.4432933118804,-0.427370559254853,
5.1789641106682));
#50011=CARTESIAN_POINT('Ctrl Pts',(-20.5228392002535,1.16027654508549,4.79477287920708));
#50012=CARTESIAN_POINT('Ctrl Pts',(-20.6023850886266,2.74792364942585,4.41058164774596));
#50013=CARTESIAN_POINT('Ctrl Pts',(-20.6819309769996,4.12578511031025,3.15946389092347));
#50014=CARTESIAN_POINT('Ctrl Pts',(-20.7614768653727,4.66092129423408,1.61613777667943));
#50015=CARTESIAN_POINT('Ctrl Pts',(-20.8410227537458,5.19605747815791,0.0728116624353919));
#50016=CARTESIAN_POINT('Ctrl Pts',(-20.9205686421189,4.88846838512118,-1.76272280923018));
#50017=CARTESIAN_POINT('Ctrl Pts',(-21.0001145304919,3.87944930013121,-3.04728760571889));
#50018=CARTESIAN_POINT('Ctrl Pts',(-21.079660418865,2.87043021514126,-4.33185240220757));
#50019=CARTESIAN_POINT('Ctrl Pts',(-21.1592063072381,1.1599811381981,-5.06544752351941));
#50020=CARTESIAN_POINT('Ctrl Pts',(-21.2387521956112,-0.466179596436317,
-4.91108594998304));
#50021=CARTESIAN_POINT('Ctrl Pts',(-21.3182980839842,-2.09234033107078,
-4.75672437644668));
#50022=CARTESIAN_POINT('Ctrl Pts',(-21.3978439723573,-3.6342127233965,-3.71440610806206));
#50023=CARTESIAN_POINT('Ctrl Pts',(-21.4773898607304,-4.38351646032473,
-2.26293439284383));
#50024=CARTESIAN_POINT('Ctrl Pts',(-21.5153127318524,-4.74074107152647,
-1.57095676937065));
#50025=CARTESIAN_POINT('Ctrl Pts',(-21.5532356029744,-4.9178283034161,-0.785985524275935));
#50026=CARTESIAN_POINT('Ctrl Pts',(-21.5911584740964,-4.91693164693359,
-0.000632398697534842));
#50027=CARTESIAN_POINT('Ctrl Pts',(-21.8088415259036,-4.91711569616659,
-0.00117946379282014));
#50028=CARTESIAN_POINT('Ctrl Pts',(-21.7725467009576,-4.91871955944082,
-0.752746704602252));
#50029=CARTESIAN_POINT('Ctrl Pts',(-21.7362518760116,-4.75716117024752,
-1.50366003608004));
#50030=CARTESIAN_POINT('Ctrl Pts',(-21.6999570510655,-4.42889215011132,
-2.17278619696736));
#50031=CARTESIAN_POINT('Ctrl Pts',(-21.6204111626925,-3.70943831968447,
-3.63928272865185));
#50032=CARTESIAN_POINT('Ctrl Pts',(-21.5408652743194,-2.18921161020874,
-4.71292520122458));
#50033=CARTESIAN_POINT('Ctrl Pts',(-21.4613193859463,-0.566549092315044,
-4.90052116218762));
#50034=CARTESIAN_POINT('Ctrl Pts',(-21.3817734975732,1.05611342557867,-5.08811712315067));
#50035=CARTESIAN_POINT('Ctrl Pts',(-21.3022276092002,2.78121175189034,-4.38966657250399));
#50036=CARTESIAN_POINT('Ctrl Pts',(-21.2226817208271,3.81629821795521,-3.12601238748351));
#50037=CARTESIAN_POINT('Ctrl Pts',(-21.143135832454,4.85138468402006,-1.86235820246306));
#50038=CARTESIAN_POINT('Ctrl Pts',(-21.0635899440809,5.19645928983812,-0.0335003830688158));
#50039=CARTESIAN_POINT('Ctrl Pts',(-20.9840440557079,4.69300726397856,1.52045005024925));
#50040=CARTESIAN_POINT('Ctrl Pts',(-20.9044981673348,4.189555238119,3.07440048356732));
#50041=CARTESIAN_POINT('Ctrl Pts',(-20.8249522789617,2.83757658058181,4.35344353080922));
#50042=CARTESIAN_POINT('Ctrl Pts',(-20.7454063905886,1.25812130277897,4.77003315738511));
#50043=CARTESIAN_POINT('Ctrl Pts',(-20.6658605022155,-0.321333975023885,
5.186622783961));
#50044=CARTESIAN_POINT('Ctrl Pts',(-20.5863146138425,-2.1282658730924,4.74075898987086));
#50045=CARTESIAN_POINT('Ctrl Pts',(-20.5067687254694,-3.33263534483166,
3.63725544792229));
#50046=CARTESIAN_POINT('Ctrl Pts',(-20.4407929922808,-4.33154503775366,
2.72200443061253));
#50047=CARTESIAN_POINT('Ctrl Pts',(-20.3748172590922,-4.91594471882842,
1.3543550430017));
#50048=CARTESIAN_POINT('Ctrl Pts',(-20.3088415259036,-4.92810468982102,
-0.00410855472338207));
#50049=CARTESIAN_POINT('Origin',(-14.75,0.,0.));
#50050=CARTESIAN_POINT('',(-18.5911584740964,-4.93133925263252,0.00269369058761092));
#50051=CARTESIAN_POINT('',(-18.8088415259036,-4.93057297854711,0.00316028518611533));
#50052=CARTESIAN_POINT('',(-14.75,-4.925,-6.03138548580071E-16));
#50053=CARTESIAN_POINT('Ctrl Pts',(-18.5911584740964,-4.93133925263252,
0.00269369058761092));
#50054=CARTESIAN_POINT('Ctrl Pts',(-18.5986849424975,-4.93235666587827,
0.157401246761113));
#50055=CARTESIAN_POINT('Ctrl Pts',(-18.6062114108986,-4.92571004477723,
0.312020226781154));
#50056=CARTESIAN_POINT('Ctrl Pts',(-18.6137378792997,-4.91111389702246,
0.465885087471429));
#50057=CARTESIAN_POINT('Ctrl Pts',(-18.6932837676727,-4.75684984141161,
2.0920550759408));
#50058=CARTESIAN_POINT('Ctrl Pts',(-18.7728296560458,-3.7146240379434,3.63398997126305));
#50059=CARTESIAN_POINT('Ctrl Pts',(-18.8523755444189,-2.26319725960073,
4.3833807487362));
#50060=CARTESIAN_POINT('Ctrl Pts',(-18.931921432792,-0.811770481258054,
5.13277152620935));
#50061=CARTESIAN_POINT('Ctrl Pts',(-19.0114673211651,1.04885727195908,5.08961818583339));
#50062=CARTESIAN_POINT('Ctrl Pts',(-19.0910132095381,2.46398102306833,4.27374380867811));
#50063=CARTESIAN_POINT('Ctrl Pts',(-19.1705590979112,3.87910477417757,3.45786943152285));
#50064=CARTESIAN_POINT('Ctrl Pts',(-19.2501049862843,4.84872452317893,1.86927401758828));
#50065=CARTESIAN_POINT('Ctrl Pts',(-19.3296508746573,4.92743208790438,0.237700743258566));
#50066=CARTESIAN_POINT('Ctrl Pts',(-19.4091967630304,5.00613965262983,-1.39387253107114));
#50067=CARTESIAN_POINT('Ctrl Pts',(-19.4887426514035,4.19393503307937,-3.068423665796));
#50068=CARTESIAN_POINT('Ctrl Pts',(-19.5682885397766,2.86391560429619,-4.01672454068289));
#50069=CARTESIAN_POINT('Ctrl Pts',(-19.6478344281497,1.53389617551299,-4.9650254155698));
#50070=CARTESIAN_POINT('Ctrl Pts',(-19.7273803165227,-0.313938062502946,
-5.18707603061872));
#50071=CARTESIAN_POINT('Ctrl Pts',(-19.8069262048958,-1.8307590101278,-4.58087437844472));
#50072=CARTESIAN_POINT('Ctrl Pts',(-19.8864720932689,-3.34757995775264,
-3.97467272627071));
#50073=CARTESIAN_POINT('Ctrl Pts',(-19.9660179816419,-4.5333876149864,-2.54021880687379));
#50074=CARTESIAN_POINT('Ctrl Pts',(-20.045563870015,-4.84346490737449,-0.936448778784566));
#50075=CARTESIAN_POINT('Ctrl Pts',(-20.0607620713755,-4.90270891386442,
-0.630029172173884));
#50076=CARTESIAN_POINT('Ctrl Pts',(-20.0759602727359,-4.92998463640529,
-0.317428729934899));
#50077=CARTESIAN_POINT('Ctrl Pts',(-20.0911584740964,-4.92710437571252,
-0.00432825790191715));
#50078=CARTESIAN_POINT('Ctrl Pts',(-20.3088415259036,-4.92810468982102,
-0.00410855472338207));
#50079=CARTESIAN_POINT('Ctrl Pts',(-20.2952713707191,-4.93060580175162,
-0.283522832407918));
#50080=CARTESIAN_POINT('Ctrl Pts',(-20.2817012155346,-4.90889778438975,
-0.562548496769959));
#50081=CARTESIAN_POINT('Ctrl Pts',(-20.2681310603502,-4.86160812861449,
-0.837169002561447));
#50082=CARTESIAN_POINT('Ctrl Pts',(-20.1885851719771,-4.58440439524805,
-2.44694662128967));
#50083=CARTESIAN_POINT('Ctrl Pts',(-20.109039283604,-3.42818988310517,-3.90535856893913));
#50084=CARTESIAN_POINT('Ctrl Pts',(-20.0294933952309,-1.9240876479818,-4.54246323682914));
#50085=CARTESIAN_POINT('Ctrl Pts',(-19.9499475068579,-0.419985412858412,
-5.17956790471916));
#50086=CARTESIAN_POINT('Ctrl Pts',(-19.8704016184848,1.43200454524547,-4.9953652928497));
#50087=CARTESIAN_POINT('Ctrl Pts',(-19.7908557301117,2.78114513946445,-4.07447140722498));
#50088=CARTESIAN_POINT('Ctrl Pts',(-19.7113098417387,4.13028573368341,-3.15357752160028));
#50089=CARTESIAN_POINT('Ctrl Pts',(-19.6317639533656,4.97657696401748,-1.49599236222033));
#50090=CARTESIAN_POINT('Ctrl Pts',(-19.5522180649925,4.93126330142958,0.136849505056872));
#50091=CARTESIAN_POINT('Ctrl Pts',(-19.4726721766194,4.88594963884169,1.76969137233409));
#50092=CARTESIAN_POINT('Ctrl Pts',(-19.3931262882463,3.94903108333184,3.37778994750857));
#50093=CARTESIAN_POINT('Ctrl Pts',(-19.3135803998733,2.55089407358275,4.22244300854623));
#50094=CARTESIAN_POINT('Ctrl Pts',(-19.2340345115002,1.15275706383363,5.06709606958391));
#50095=CARTESIAN_POINT('Ctrl Pts',(-19.1544886231271,-0.706598400154735,
5.14830361648474));
#50096=CARTESIAN_POINT('Ctrl Pts',(-19.074942734754,-2.17305178497508,4.42876184445237));
#50097=CARTESIAN_POINT('Ctrl Pts',(-18.995396846381,-3.63950516979541,3.70922007242002));
#50098=CARTESIAN_POINT('Ctrl Pts',(-18.9158509580079,-4.71305647544771,
2.18892898145449));
#50099=CARTESIAN_POINT('Ctrl Pts',(-18.8363050696348,-4.90055512820742,
0.566255216718109));
#50100=CARTESIAN_POINT('Ctrl Pts',(-18.8271505550577,-4.92213335412174,
0.379510295806119));
#50101=CARTESIAN_POINT('Ctrl Pts',(-18.8179960404807,-4.93197626646748,
0.191409368818455));
#50102=CARTESIAN_POINT('Ctrl Pts',(-18.8088415259036,-4.93057297854711,
0.00316028518611533));
#50103=CARTESIAN_POINT('Origin',(-14.75,0.,0.));
#50104=CARTESIAN_POINT('',(-17.0911584740964,-4.91873477802609,0.00299898967114021));
#50105=CARTESIAN_POINT('',(-17.3088415259036,-4.91816086074912,0.00255430743475421));
#50106=CARTESIAN_POINT('',(-14.75,-4.925,-6.03138548580071E-16));
#50107=CARTESIAN_POINT('Ctrl Pts',(-17.0911584740964,-4.91873477802609,
0.00299898967114021));
#50108=CARTESIAN_POINT('Ctrl Pts',(-17.121409612259,-4.92219933969977,0.628902743871938));
#50109=CARTESIAN_POINT('Ctrl Pts',(-17.1516607504217,-4.81148680932676,
1.25362658234333));
#50110=CARTESIAN_POINT('Ctrl Pts',(-17.1819118885843,-4.58098415721058,
1.83048430084528));
#50111=CARTESIAN_POINT('Ctrl Pts',(-17.2614577769574,-3.97487346688356,
3.34734159845876));
#50112=CARTESIAN_POINT('Ctrl Pts',(-17.3410036653305,-2.54049066060951,
4.53323527492929));
#50113=CARTESIAN_POINT('Ctrl Pts',(-17.4205495537035,-0.936739230126934,
4.84340874168148));
#50114=CARTESIAN_POINT('Ctrl Pts',(-17.5000954420766,0.667012200355664,
5.15358220843367));
#50115=CARTESIAN_POINT('Ctrl Pts',(-17.5796413304497,2.44013225504679,4.58803546546751));
#50116=CARTESIAN_POINT('Ctrl Pts',(-17.6591872188228,3.56811382315476,3.40656019604341));
#50117=CARTESIAN_POINT('Ctrl Pts',(-17.7387331071958,4.69609539126271,2.22508492661932));
#50118=CARTESIAN_POINT('Ctrl Pts',(-17.8182789955689,5.17893847278751,0.427681130737319));
#50119=CARTESIAN_POINT('Ctrl Pts',(-17.897824883942,4.79484245007892,-1.15998900993782));
#50120=CARTESIAN_POINT('Ctrl Pts',(-17.9773707723151,4.41074642737033,-2.74765915061299));
#50121=CARTESIAN_POINT('Ctrl Pts',(-18.0569166606881,3.15971130042833,-4.12559563608129));
#50122=CARTESIAN_POINT('Ctrl Pts',(-18.1364625490612,1.61641728001955,-4.66082436926233));
#50123=CARTESIAN_POINT('Ctrl Pts',(-18.2160084374343,0.0731232596108,-5.19605310244336));
#50124=CARTESIAN_POINT('Ctrl Pts',(-18.2955543258074,-1.76242965426471,
-4.88857408333716));
#50125=CARTESIAN_POINT('Ctrl Pts',(-18.3751002141804,-3.04705495732574,
-3.87963203297581));
#50126=CARTESIAN_POINT('Ctrl Pts',(-18.4471196341524,-4.21013165556918,
-2.96615400490252));
#50127=CARTESIAN_POINT('Ctrl Pts',(-18.5191390541244,-4.92160380860666,
-1.47767503842927));
#50128=CARTESIAN_POINT('Ctrl Pts',(-18.5911584740964,-4.93133925263252,
0.00269369058761092));
#50129=CARTESIAN_POINT('Ctrl Pts',(-18.8088415259036,-4.93057297854711,
0.00316028518611533));
#50130=CARTESIAN_POINT('Ctrl Pts',(-18.7384501521076,-4.91978274344346,
-1.4443344455465));
#50131=CARTESIAN_POINT('Ctrl Pts',(-18.6680587783116,-4.24406537670826,
-2.90058887915162));
#50132=CARTESIAN_POINT('Ctrl Pts',(-18.5976674045156,-3.12578352599411,
-3.8164856718825));
#50133=CARTESIAN_POINT('Ctrl Pts',(-18.5181215161425,-1.86206727115392,
-4.85149635723954));
#50134=CARTESIAN_POINT('Ctrl Pts',(-18.4385756277694,-0.0331887616064278,
-5.19646128944632));
#50135=CARTESIAN_POINT('Ctrl Pts',(-18.3590297393964,1.52073147789346,-4.69291607715336));
#50136=CARTESIAN_POINT('Ctrl Pts',(-18.2794838510233,3.07465171739332,-4.18937086486042));
#50137=CARTESIAN_POINT('Ctrl Pts',(-18.1999379626502,4.35361368684558,-2.83731550806776));
#50138=CARTESIAN_POINT('Ctrl Pts',(-18.1203920742771,4.77010859585846,-1.2578352510475));
#50139=CARTESIAN_POINT('Ctrl Pts',(-18.0408461859041,5.18660350487135,0.321645005972764));
#50140=CARTESIAN_POINT('Ctrl Pts',(-17.961300297531,4.74063135344486,2.12855016322063));
#50141=CARTESIAN_POINT('Ctrl Pts',(-17.8817544091579,3.63705558982148,3.33285345786593));
#50142=CARTESIAN_POINT('Ctrl Pts',(-17.8022085207848,2.53347982619808,4.53715675251125));
#50143=CARTESIAN_POINT('Ctrl Pts',(-17.7226626324118,0.772300450377784,
5.13885818455397));
#50144=CARTESIAN_POINT('Ctrl Pts',(-17.6431167440387,-0.837460542095409,
4.86155791650103));
#50145=CARTESIAN_POINT('Ctrl Pts',(-17.5635708556656,-2.44722153456857,
4.58425764844809));
#50146=CARTESIAN_POINT('Ctrl Pts',(-17.4840249672925,-3.90556414369463,
3.42795568029952));
#50147=CARTESIAN_POINT('Ctrl Pts',(-17.4044790789195,-4.5425786123982,1.92381524197179));
#50148=CARTESIAN_POINT('Ctrl Pts',(-17.3725998945808,-4.79787152683423,
1.32100884574773));
#50149=CARTESIAN_POINT('Ctrl Pts',(-17.3407207102422,-4.92124900075768,
0.662335296357207));
#50150=CARTESIAN_POINT('Ctrl Pts',(-17.3088415259036,-4.91816086074912,
0.00255430743475421));
#50151=CARTESIAN_POINT('Origin',(-14.75,0.,0.));
#50152=CARTESIAN_POINT('',(-15.5911584740964,-4.92035796642718,-0.00383015064837622));
#50153=CARTESIAN_POINT('',(-15.8088415259036,-4.92120003017842,-0.00410675641256026));
#50154=CARTESIAN_POINT('',(-14.75,-4.925,-6.03138548580071E-16));
#50155=CARTESIAN_POINT('Ctrl Pts',(-15.5911584740964,-4.92035796642718,
-0.00383015064837622));
#50156=CARTESIAN_POINT('Ctrl Pts',(-15.6441342820206,-4.9124462735778,1.09134504077847));
#50157=CARTESIAN_POINT('Ctrl Pts',(-15.6971100899448,-4.55169660768519,
2.19124987504687));
#50158=CARTESIAN_POINT('Ctrl Pts',(-15.750085897869,-3.87981475186871,3.04682229797494));
#50159=CARTESIAN_POINT('Ctrl Pts',(-15.829631786242,-2.87094973976422,4.33150810298851));
#50160=CARTESIAN_POINT('Ctrl Pts',(-15.9091776746151,-1.16058865962495,
5.06530836353102));
#50161=CARTESIAN_POINT('Ctrl Pts',(-15.9887235629882,0.465590576831222,
4.91114182640059));
#50162=CARTESIAN_POINT('Ctrl Pts',(-16.0682694513612,2.0917698132874,4.75697528927016));
#50163=CARTESIAN_POINT('Ctrl Pts',(-16.1478153397343,3.63376720606049,3.71484195446679));
#50164=CARTESIAN_POINT('Ctrl Pts',(-16.2273612281074,4.38324502138396,2.26346011821903));
#50165=CARTESIAN_POINT('Ctrl Pts',(-16.3069071164805,5.13272283670744,0.812078281971235));
#50166=CARTESIAN_POINT('Ctrl Pts',(-16.3864530048536,5.08968107458128,-1.04855205572096));
#50167=CARTESIAN_POINT('Ctrl Pts',(-16.4659988932266,4.27389156106992,-2.46372473066101));
#50168=CARTESIAN_POINT('Ctrl Pts',(-16.5455447815997,3.45810204755859,-3.87889740560104));
#50169=CARTESIAN_POINT('Ctrl Pts',(-16.6250906699728,1.86956478266209,-4.84861241778893));
#50170=CARTESIAN_POINT('Ctrl Pts',(-16.7046365583459,0.237996231203316,
-4.92741782460026));
#50171=CARTESIAN_POINT('Ctrl Pts',(-16.7841824467189,-1.39357232025546,
-5.00622323141159));
#50172=CARTESIAN_POINT('Ctrl Pts',(-16.863728335092,-3.06817215827651,-4.19411903284637));
#50173=CARTESIAN_POINT('Ctrl Pts',(-16.9432742234651,-4.01655279009705,
-2.86415647418555));
#50174=CARTESIAN_POINT('Ctrl Pts',(-16.9925689736755,-4.60426621320643,
-2.03997594821106));
#50175=CARTESIAN_POINT('Ctrl Pts',(-17.041863723886,-4.91308921515918,-1.01692194861672));
#50176=CARTESIAN_POINT('Ctrl Pts',(-17.0911584740964,-4.91873477802609,
0.00299898967114021));
#50177=CARTESIAN_POINT('Ctrl Pts',(-17.3088415259036,-4.91816086074912,
0.00255430743475421));
#50178=CARTESIAN_POINT('Ctrl Pts',(-17.2611748218691,-4.91354338201311,
-0.983969839246001));
#50179=CARTESIAN_POINT('Ctrl Pts',(-17.2135081178347,-4.62618522137736,
-1.9729699017009));
#50180=CARTESIAN_POINT('Ctrl Pts',(-17.1658414138002,-4.07430462011665,
-2.78138947246816));
#50181=CARTESIAN_POINT('Ctrl Pts',(-17.0862955254271,-3.15332983085048,
-4.13047484007342));
#50182=CARTESIAN_POINT('Ctrl Pts',(-17.0067496370541,-1.4956939240371,-4.97666666677702));
#50183=CARTESIAN_POINT('Ctrl Pts',(-16.927203748681,0.137145222933267,-4.93125508596819));
#50184=CARTESIAN_POINT('Ctrl Pts',(-16.8476578603079,1.76998436990362,-4.88584350515936));
#50185=CARTESIAN_POINT('Ctrl Pts',(-16.7681119719349,3.37802675703098,-3.94882851683809));
#50186=CARTESIAN_POINT('Ctrl Pts',(-16.6885660835618,4.2225959730343,-2.55064085742682));
#50187=CARTESIAN_POINT('Ctrl Pts',(-16.6090201951887,5.06716518903764,-1.15245319801552));
#50188=CARTESIAN_POINT('Ctrl Pts',(-16.5294743068156,5.14826123391693,0.706907132485781));
#50189=CARTESIAN_POINT('Ctrl Pts',(-16.4499284184425,4.42863152286466,2.17331736517013));
#50190=CARTESIAN_POINT('Ctrl Pts',(-16.3703825300695,3.7090018118124,3.63972759785445));
#50191=CARTESIAN_POINT('Ctrl Pts',(-16.2908366416964,2.18864634482861,4.71318773272181));
#50192=CARTESIAN_POINT('Ctrl Pts',(-16.2112907533233,0.565961339085978,
4.90058907660299));
#50193=CARTESIAN_POINT('Ctrl Pts',(-16.1317448649502,-1.05672366665665,
5.08799042048417));
#50194=CARTESIAN_POINT('Ctrl Pts',(-16.0521989765772,-2.78173821115814,
4.38933297337918));
#50195=CARTESIAN_POINT('Ctrl Pts',(-15.9726530882041,-3.81667311208576,
3.12555465326431));
#50196=CARTESIAN_POINT('Ctrl Pts',(-15.9180492341039,-4.52709869773482,
2.25804071360155));
#50197=CARTESIAN_POINT('Ctrl Pts',(-15.8634453800038,-4.91235438239858,
1.1242382374886));
#50198=CARTESIAN_POINT('Ctrl Pts',(-15.8088415259036,-4.92120003017842,
-0.00410675641256026));
#50199=CARTESIAN_POINT('Origin',(-14.75,0.,0.));
#50200=CARTESIAN_POINT('',(-14.0911584740964,-4.93264269199776,-0.00145718338004752));
#50201=CARTESIAN_POINT('',(-14.3088415259036,-4.93298263358733,-0.000852151517113329));
#50202=CARTESIAN_POINT('',(-14.75,-4.925,-6.03138548580071E-16));
#50203=CARTESIAN_POINT('Ctrl Pts',(-14.0911584740964,-4.93264269199776,
-0.00145718338004752));
#50204=CARTESIAN_POINT('Ctrl Pts',(-14.1668589517821,-4.92658863837471,
1.55348689693233));
#50205=CARTESIAN_POINT('Ctrl Pts',(-14.2425594294679,-4.13001266093176,
3.11377115163446));
#50206=CARTESIAN_POINT('Ctrl Pts',(-14.3182599071536,-2.86439733377493,
4.01638102506703));
#50207=CARTESIAN_POINT('Ctrl Pts',(-14.3978057955267,-1.5344916500192,4.96484141041069));
#50208=CARTESIAN_POINT('Ctrl Pts',(-14.4773516838997,0.313315942832746,
5.18711364580286));
#50209=CARTESIAN_POINT('Ctrl Pts',(-14.5568975722728,1.83020958498003,4.58109391950248));
#50210=CARTESIAN_POINT('Ctrl Pts',(-14.6364434606459,3.3471032271273,3.97507419320211));
#50211=CARTESIAN_POINT('Ctrl Pts',(-14.715989349019,4.53308291856992,2.5407625052092));
#50212=CARTESIAN_POINT('Ctrl Pts',(-14.7955352373921,4.84335255857077,0.937029678100604));
#50213=CARTESIAN_POINT('Ctrl Pts',(-14.8750811257651,5.15362219857162,-0.666703149008015));
#50214=CARTESIAN_POINT('Ctrl Pts',(-14.9546270141382,4.58818178713068,-2.43985711523233));
#50215=CARTESIAN_POINT('Ctrl Pts',(-15.0341729025113,3.40677416265819,-3.56790953205094));
#50216=CARTESIAN_POINT('Ctrl Pts',(-15.1137187908843,2.22536653818572,-4.69596194886955));
#50217=CARTESIAN_POINT('Ctrl Pts',(-15.1932646792574,0.427991700681723,
-5.17891281628248));
#50218=CARTESIAN_POINT('Ctrl Pts',(-15.2728105676305,-1.15970147061867,
-4.79491200370771));
#50219=CARTESIAN_POINT('Ctrl Pts',(-15.3523564560036,-2.74739464191907,
-4.41091119113294));
#50220=CARTESIAN_POINT('Ctrl Pts',(-15.4319023443767,-4.12540614701586,
-3.15995869857046));
#50221=CARTESIAN_POINT('Ctrl Pts',(-15.5114482327497,-4.6607274275294,-1.61669677754691));
#50222=CARTESIAN_POINT('Ctrl Pts',(-15.5380183131986,-4.83953653734212,
-1.10121327193814));
#50223=CARTESIAN_POINT('Ctrl Pts',(-15.5645883936475,-4.92432608553159,
-0.553116590668242));
#50224=CARTESIAN_POINT('Ctrl Pts',(-15.5911584740964,-4.92035796642718,
-0.00383015064837622));
#50225=CARTESIAN_POINT('Ctrl Pts',(-15.8088415259036,-4.92120003017842,
-0.00410675641256026));
#50226=CARTESIAN_POINT('Ctrl Pts',(-15.7838994916307,-4.92524055907015,
-0.519513955654037));
#50227=CARTESIAN_POINT('Ctrl Pts',(-15.7589574573578,-4.85074335816441,
-1.03378245448552));
#50228=CARTESIAN_POINT('Ctrl Pts',(-15.7340154230849,-4.69282487345136,
-1.52101290006915));
#50229=CARTESIAN_POINT('Ctrl Pts',(-15.6544695347118,-4.18918647653558,
-3.07490294016289));
#50230=CARTESIAN_POINT('Ctrl Pts',(-15.5749236463387,-2.83705442535027,
-4.35378382722562));
#50231=CARTESIAN_POINT('Ctrl Pts',(-15.4953777579656,-1.25754919479281,
-4.77018401717759));
#50232=CARTESIAN_POINT('Ctrl Pts',(-15.4158318695926,0.321956035764672,
-5.18658420712955));
#50233=CARTESIAN_POINT('Ctrl Pts',(-15.3362859812195,2.12883444569431,-4.74050369997076));
#50234=CARTESIAN_POINT('Ctrl Pts',(-15.2567400928464,3.33307155891485,-3.63685571864124));
#50235=CARTESIAN_POINT('Ctrl Pts',(-15.1771942044733,4.5373086721354,-2.53320773731172));
#50236=CARTESIAN_POINT('Ctrl Pts',(-15.0976483161003,5.13890448864684,-0.771992281811449));
#50237=CARTESIAN_POINT('Ctrl Pts',(-15.0181024277272,4.86150768690456,0.837752078617765));
#50238=CARTESIAN_POINT('Ctrl Pts',(-14.9385565393541,4.58411088516229,2.44749643904697));
#50239=CARTESIAN_POINT('Ctrl Pts',(-14.859010650981,3.42772146516635,3.90576970440512));
#50240=CARTESIAN_POINT('Ctrl Pts',(-14.779464762608,1.92354282904339,4.5426939716314));
#50241=CARTESIAN_POINT('Ctrl Pts',(-14.6999188742349,0.419364192920443,
5.17961823885768));
#50242=CARTESIAN_POINT('Ctrl Pts',(-14.6203729858618,-1.43260365932953,
4.99519350795208));
#50243=CARTESIAN_POINT('Ctrl Pts',(-14.5408270974887,-2.78163379546954,
4.07413781835645));
#50244=CARTESIAN_POINT('Ctrl Pts',(-14.463498573627,-4.09305932865878,3.17875682095258));
#50245=CARTESIAN_POINT('Ctrl Pts',(-14.3861700497653,-4.92919541411866,
1.58724007886021));
#50246=CARTESIAN_POINT('Ctrl Pts',(-14.3088415259036,-4.93298263358733,
-0.000852151517113329));
#50247=CARTESIAN_POINT('Origin',(-14.75,0.,0.));
#50248=CARTESIAN_POINT('',(-12.5911584740964,-4.92478776395509,0.00455105250847659));
#50249=CARTESIAN_POINT('',(-12.8088415259036,-4.92377532403654,0.00452825219503028));
#50250=CARTESIAN_POINT('',(-14.75,-4.925,-6.03138548580071E-16));
#50251=CARTESIAN_POINT('Ctrl Pts',(-12.5911584740964,-4.92478776395509,
0.00455105250847659));
#50252=CARTESIAN_POINT('Ctrl Pts',(-12.6100377331706,-4.92837678960448,
0.393954978247036));
#50253=CARTESIAN_POINT('Ctrl Pts',(-12.6289169922448,-4.88609691325311,
0.78258860004133));
#50254=CARTESIAN_POINT('Ctrl Pts',(-12.647796251319,-4.79498154009321,1.15941392712904));
#50255=CARTESIAN_POINT('Ctrl Pts',(-12.7273421396921,-4.41107593903318,
2.74713012334508));
#50256=CARTESIAN_POINT('Ctrl Pts',(-12.8068880280651,-3.16020608534884,
4.12521664311483));
#50257=CARTESIAN_POINT('Ctrl Pts',(-12.8864339164382,-1.61697626926029,
4.66063046903576));
#50258=CARTESIAN_POINT('Ctrl Pts',(-12.9659798048113,-0.0737464531717311,
5.19604429495669));
#50259=CARTESIAN_POINT('Ctrl Pts',(-13.0455256931844,1.76184332532101,4.8887854270288));
#50260=CARTESIAN_POINT('Ctrl Pts',(-13.1250715815575,3.04658962766721,3.87999745680921));
#50261=CARTESIAN_POINT('Ctrl Pts',(-13.2046174699305,4.33133593001341,2.87120948658962));
#50262=CARTESIAN_POINT('Ctrl Pts',(-13.2841633583036,5.06523875621307,1.16089241407827));
#50263=CARTESIAN_POINT('Ctrl Pts',(-13.3637092466767,4.91116973811745,-0.465296064516709));
#50264=CARTESIAN_POINT('Ctrl Pts',(-13.4432551350498,4.75710072002183,-2.09148454311171));
#50265=CARTESIAN_POINT('Ctrl Pts',(-13.5228010234228,3.71505985763101,-3.63354442779033));
#50266=CARTESIAN_POINT('Ctrl Pts',(-13.6023469117959,2.26372296869752,-4.38310927826887));
#50267=CARTESIAN_POINT('Ctrl Pts',(-13.681892800169,0.812386079764056,-5.13267412874741));
#50268=CARTESIAN_POINT('Ctrl Pts',(-13.7614386885421,-1.0482468357121,-5.08974394502581));
#50269=CARTESIAN_POINT('Ctrl Pts',(-13.8409845769151,-2.46346842939373,
-4.27403929809212));
#50270=CARTESIAN_POINT('Ctrl Pts',(-13.9205304652882,-3.87869002307536,
-3.45833465115842));
#50271=CARTESIAN_POINT('Ctrl Pts',(-14.0000763536613,-4.84850029496252,
-1.86985554101265));
#50272=CARTESIAN_POINT('Ctrl Pts',(-14.0796222420344,-4.92740354357634,
-0.238291718292194));
#50273=CARTESIAN_POINT('Ctrl Pts',(-14.0834676527217,-4.93121788774538,
-0.159418591229293));
#50274=CARTESIAN_POINT('Ctrl Pts',(-14.0873130634091,-4.93295022404004,
-0.0804447772164642));
#50275=CARTESIAN_POINT('Ctrl Pts',(-14.0911584740964,-4.93264269199776,
-0.00145718338004752));
#50276=CARTESIAN_POINT('Ctrl Pts',(-14.3088415259036,-4.93298263358733,
-0.000852151517113329));
#50277=CARTESIAN_POINT('Ctrl Pts',(-14.3066241613922,-4.93309123059174,
-0.0463900614183807));
#50278=CARTESIAN_POINT('Ctrl Pts',(-14.3044067968809,-4.93251544314009,
-0.0919251555741316));
#50279=CARTESIAN_POINT('Ctrl Pts',(-14.3021894323695,-4.93124685277319,
-0.137440940316469));
#50280=CARTESIAN_POINT('Ctrl Pts',(-14.2226435439964,-4.88573735390672,
-1.77027736110802));
#50281=CARTESIAN_POINT('Ctrl Pts',(-14.1430976556234,-3.94862593614372,
-3.37826355440545));
#50282=CARTESIAN_POINT('Ctrl Pts',(-14.0635517672503,-2.55038763209838,
-4.22274892233722));
#50283=CARTESIAN_POINT('Ctrl Pts',(-13.9840058788772,-1.15214932805305,
-5.06723429026899));
#50284=CARTESIAN_POINT('Ctrl Pts',(-13.9044599905041,0.707215862274635,
-5.14821883283511));
#50285=CARTESIAN_POINT('Ctrl Pts',(-13.8249141021311,2.17358293754952,-4.42850118535088));
#50286=CARTESIAN_POINT('Ctrl Pts',(-13.745368213758,3.6399500128244,-3.70878353786665));
#50287=CARTESIAN_POINT('Ctrl Pts',(-13.6658223253849,4.71331897304647,-2.18836370033207));
#50288=CARTESIAN_POINT('Ctrl Pts',(-13.5862764370118,4.90062300737523,-0.565667459418628));
#50289=CARTESIAN_POINT('Ctrl Pts',(-13.5067305486388,5.08792704170398,1.05702878149484));
#50290=CARTESIAN_POINT('Ctrl Pts',(-13.4271846602657,4.38916615013937,2.78200142578717));
#50291=CARTESIAN_POINT('Ctrl Pts',(-13.3476387718926,3.12532576929452,3.81686053856362));
#50292=CARTESIAN_POINT('Ctrl Pts',(-13.2680928835195,1.86148538844969,4.85171965134006));
#50293=CARTESIAN_POINT('Ctrl Pts',(-13.1885469951465,0.0325655183246379,
5.19646523260064));
#50294=CARTESIAN_POINT('Ctrl Pts',(-13.1090011067734,-1.52129431677496,
4.69273365287321));
#50295=CARTESIAN_POINT('Ctrl Pts',(-13.0294552184003,-3.07515415187458,
4.18900207314577));
#50296=CARTESIAN_POINT('Ctrl Pts',(-12.9499093300272,-4.35395395194874,
2.8367933324303));
#50297=CARTESIAN_POINT('Ctrl Pts',(-12.8703634416541,-4.77025942134235,
1.25726313401576));
#50298=CARTESIAN_POINT('Ctrl Pts',(-12.849856136404,-4.87758493511541,0.850052798028952));
#50299=CARTESIAN_POINT('Ctrl Pts',(-12.8293488311538,-4.92758625344338,
0.427733934129015));
#50300=CARTESIAN_POINT('Ctrl Pts',(-12.8088415259036,-4.92377532403654,
0.00452825219503028));
#50301=CARTESIAN_POINT('Origin',(-14.75,0.,0.));
#50302=CARTESIAN_POINT('',(-11.0911584740964,-4.91693014897725,-0.000625914149278983));
#50303=CARTESIAN_POINT('',(-11.3088415259036,-4.91711289028958,-0.00117313378838655));
#50304=CARTESIAN_POINT('',(-14.75,-4.925,-6.03138548580071E-16));
#50305=CARTESIAN_POINT('Ctrl Pts',(-11.0911584740964,-4.91693014897725,
-0.000625914149278983));
#50306=CARTESIAN_POINT('Ctrl Pts',(-11.1327624029322,-4.91595655984975,
0.8609597041095));
#50307=CARTESIAN_POINT('Ctrl Pts',(-11.1743663317679,-4.70077081773724,
1.72300021548812));
#50308=CARTESIAN_POINT('Ctrl Pts',(-11.2159702606036,-4.27418701974417,
2.46321211926741));
#50309=CARTESIAN_POINT('Ctrl Pts',(-11.2955161489767,-3.45856724232153,
3.87848262660126));
#50310=CARTESIAN_POINT('Ctrl Pts',(-11.3750620373498,-1.87014629263889,
4.84838815470011));
#50311=CARTESIAN_POINT('Ctrl Pts',(-11.4546079257229,-0.238587204524135,
4.92738924483267));
#50312=CARTESIAN_POINT('Ctrl Pts',(-11.5341538140959,1.39297188359064,5.00639033496524));
#50313=CARTESIAN_POINT('Ctrl Pts',(-11.613699702469,3.06766911013748,4.19448698713153));
#50314=CARTESIAN_POINT('Ctrl Pts',(-11.6932455908421,4.01620924559344,2.86463818306347));
#50315=CARTESIAN_POINT('Ctrl Pts',(-11.7727914792152,4.96474938104939,1.53478937899541));
#50316=CARTESIAN_POINT('Ctrl Pts',(-11.8523373675882,5.18713242541439,-0.313004881306989));
#50317=CARTESIAN_POINT('Ctrl Pts',(-11.9318832559613,4.58120366532001,-1.82993486253306));
#50318=CARTESIAN_POINT('Ctrl Pts',(-12.0114291443344,3.97527490522564,-3.34686484375911));
#50319=CARTESIAN_POINT('Ctrl Pts',(-12.0909750327075,2.54103434067188,-4.53293054590886));
#50320=CARTESIAN_POINT('Ctrl Pts',(-12.1705209210806,0.937320122704561,
-4.84329635804258));
#50321=CARTESIAN_POINT('Ctrl Pts',(-12.2500668094536,-0.666394095262762,
-5.1536621701763));
#50322=CARTESIAN_POINT('Ctrl Pts',(-12.3296126978267,-2.43958196664368,
-4.588328092294));
#50323=CARTESIAN_POINT('Ctrl Pts',(-12.4091585861998,-3.56770522811629,
-3.4069881170217));
#50324=CARTESIAN_POINT('Ctrl Pts',(-12.4698252154987,-4.42808201322696,
-2.50602496453717));
#50325=CARTESIAN_POINT('Ctrl Pts',(-12.5304918447975,-4.91325478547539,
-1.24675989764379));
#50326=CARTESIAN_POINT('Ctrl Pts',(-12.5911584740964,-4.92478776395509,
0.00455105250847659));
#50327=CARTESIAN_POINT('Ctrl Pts',(-12.8088415259036,-4.92377532403654,
0.00452825219503028));
#50328=CARTESIAN_POINT('Ctrl Pts',(-12.7498029427807,-4.91280402040514,
-1.21384069126802));
#50329=CARTESIAN_POINT('Ctrl Pts',(-12.6907643596578,-4.45583175677877,
-2.43955966583319));
#50330=CARTESIAN_POINT('Ctrl Pts',(-12.6317257765349,-3.63665583438227,
-3.33328964797749));
#50331=CARTESIAN_POINT('Ctrl Pts',(-12.5521798881619,-2.53293563931553,
-4.53746057544264));
#50332=CARTESIAN_POINT('Ctrl Pts',(-12.4726339997888,-0.771684110468958,
-5.13895077425935));
#50333=CARTESIAN_POINT('Ctrl Pts',(-12.3930881114157,0.838043612127357,
-4.86145743982533));
#50334=CARTESIAN_POINT('Ctrl Pts',(-12.3135422230426,2.44777133472372,-4.58396410539131));
#50335=CARTESIAN_POINT('Ctrl Pts',(-12.2339963346695,3.90597525106984,-3.42748723770652));
#50336=CARTESIAN_POINT('Ctrl Pts',(-12.1544504462965,4.54280931452835,-1.92327040919758));
#50337=CARTESIAN_POINT('Ctrl Pts',(-12.0749045579234,5.17964337798684,-0.419053580688679));
#50338=CARTESIAN_POINT('Ctrl Pts',(-11.9953586695503,4.99510758855781,1.43290320864429));
#50339=CARTESIAN_POINT('Ctrl Pts',(-11.9158127811772,4.07397100194497,2.78187810846774));
#50340=CARTESIAN_POINT('Ctrl Pts',(-11.8362668928042,3.15283441533213,4.13085300829118));
#50341=CARTESIAN_POINT('Ctrl Pts',(-11.7567210044311,1.49509703153545,4.97684601860504));
#50342=CARTESIAN_POINT('Ctrl Pts',(-11.677175116058,-0.137736657205341,
4.93123860184462));
#50343=CARTESIAN_POINT('Ctrl Pts',(-11.5976292276849,-1.77057034594614,
4.88563118508419));
#50344=CARTESIAN_POINT('Ctrl Pts',(-11.5180833393119,-3.37850033963107,
3.94842334124948));
#50345=CARTESIAN_POINT('Ctrl Pts',(-11.4385374509388,-4.22290185645441,
2.55013439759839));
#50346=CARTESIAN_POINT('Ctrl Pts',(-11.3953054759271,-4.68182117990154,
1.79018572008053));
#50347=CARTESIAN_POINT('Ctrl Pts',(-11.3520735009153,-4.91521278868756,
0.894044916314203));
#50348=CARTESIAN_POINT('Ctrl Pts',(-11.3088415259036,-4.91711289028958,
-0.00117313378838655));
#50349=CARTESIAN_POINT('Origin',(-14.75,0.,0.));
#50350=CARTESIAN_POINT('',(-9.59115847409641,-4.92709248349153,-0.00433039759252629));
#50351=CARTESIAN_POINT('',(-9.80884152590359,-4.92809314710804,-0.00411155299795817));
#50352=CARTESIAN_POINT('',(-14.75,-4.925,-6.03138548580071E-16));
#50353=CARTESIAN_POINT('Ctrl Pts',(-9.59115847409641,-4.92709248349153,
-0.00433039759252629));
#50354=CARTESIAN_POINT('Ctrl Pts',(-9.6554870726937,-4.91489864183716,1.32092114795559));
#50355=CARTESIAN_POINT('Ctrl Pts',(-9.71981567129099,-4.36249459000914,
2.65513262914084));
#50356=CARTESIAN_POINT('Ctrl Pts',(-9.78414426988828,-3.40720205913308,
3.56750091135165));
#50357=CARTESIAN_POINT('Ctrl Pts',(-9.86369015826136,-2.2259297373092,4.69569501342137));
#50358=CARTESIAN_POINT('Ctrl Pts',(-9.94323604663443,-0.428612835952052,
5.17886144739986));
#50359=CARTESIAN_POINT('Ctrl Pts',(-10.0227819350075,1.15912637946997,4.79505105923515));
#50360=CARTESIAN_POINT('Ctrl Pts',(-10.1023278233806,2.74686559489197,4.41124067107045));
#50361=CARTESIAN_POINT('Ctrl Pts',(-10.1818737117537,4.12502712437884,3.16045346076258));
#50362=CARTESIAN_POINT('Ctrl Pts',(-10.2614196001267,4.66053349378172,1.61725575515876));
#50363=CARTESIAN_POINT('Ctrl Pts',(-10.3409654884998,5.19603986318461,0.0740580495549087));
#50364=CARTESIAN_POINT('Ctrl Pts',(-10.4205113768729,4.88889107250348,-1.76155015134491));
#50365=CARTESIAN_POINT('Ctrl Pts',(-10.500057265246,3.88018014779652,-3.04635694640356));
#50366=CARTESIAN_POINT('Ctrl Pts',(-10.579603153619,2.87146922308957,-4.3311637414622));
#50367=CARTESIAN_POINT('Ctrl Pts',(-10.6591490419921,1.16119616435681,-5.06516913067968));
#50368=CARTESIAN_POINT('Ctrl Pts',(-10.7386949303652,-0.465001550528919,
-4.91119763217294));
#50369=CARTESIAN_POINT('Ctrl Pts',(-10.8182408187383,-2.09119926541465,
-4.75722613366619));
#50370=CARTESIAN_POINT('Ctrl Pts',(-10.8977867071114,-3.63332163645336,
-3.71527774743521));
#50371=CARTESIAN_POINT('Ctrl Pts',(-10.9773325954844,-4.3829735193914,-2.26398581103529));
#50372=CARTESIAN_POINT('Ctrl Pts',(-11.0152745550218,-4.74054399840997,
-1.5717456330203));
#50373=CARTESIAN_POINT('Ctrl Pts',(-11.0532165145591,-4.91781804298907,
-0.786374942684098));
#50374=CARTESIAN_POINT('Ctrl Pts',(-11.0911584740964,-4.91693014897725,
-0.000625914149278983));
#50375=CARTESIAN_POINT('Ctrl Pts',(-11.3088415259036,-4.91711289028958,
-0.00117313378838655));
#50376=CARTESIAN_POINT('Ctrl Pts',(-11.2725276125423,-4.91870893407279,
-0.753136714034694));
#50377=CARTESIAN_POINT('Ctrl Pts',(-11.2362136991809,-4.7569730771308,-1.5044492332048));
#50378=CARTESIAN_POINT('Ctrl Pts',(-11.1998997858196,-4.42837083191147,
-2.1738485021124));
#50379=CARTESIAN_POINT('Ctrl Pts',(-11.1203538974465,-3.70856525058346,
-3.64017241470453));
#50380=CARTESIAN_POINT('Ctrl Pts',(-11.0408080090734,-2.18808104796575,
-4.71345019642131));
#50381=CARTESIAN_POINT('Ctrl Pts',(-10.9612621207003,-0.565373577716975,
-4.90065692052403));
#50382=CARTESIAN_POINT('Ctrl Pts',(-10.8817162323273,1.05733389253182,-5.08786364462675));
#50383=CARTESIAN_POINT('Ctrl Pts',(-10.8021703439542,2.78226463041168,-4.38899931111538));
#50384=CARTESIAN_POINT('Ctrl Pts',(-10.7226244555811,3.81704795131542,-3.12509687408555));
#50385=CARTESIAN_POINT('Ctrl Pts',(-10.643078567208,4.85183127221915,-1.86119443705574));
#50386=CARTESIAN_POINT('Ctrl Pts',(-10.563532678835,5.1964671761468,-0.0322538965074959));
#50387=CARTESIAN_POINT('Ctrl Pts',(-10.4839867904619,4.6926424154192,1.52157572801001));
#50388=CARTESIAN_POINT('Ctrl Pts',(-10.4044409020888,4.1888176546916,3.07540535252754));
#50389=CARTESIAN_POINT('Ctrl Pts',(-10.3248950137157,2.83653222930873,4.35412406101433));
#50390=CARTESIAN_POINT('Ctrl Pts',(-10.2453491253427,1.25697706871738,4.77033480835247));
#50391=CARTESIAN_POINT('Ctrl Pts',(-10.1658032369696,-0.322578091873937,
5.1865455556906));
#50392=CARTESIAN_POINT('Ctrl Pts',(-10.0862573485965,-2.12940298767373,
4.74024834188012));
#50393=CARTESIAN_POINT('Ctrl Pts',(-10.0067114602234,-3.33350772505308,
3.6364559370453));
#50394=CARTESIAN_POINT('Ctrl Pts',(-9.94075481545016,-4.33190890024233,
2.72123020963015));
#50395=CARTESIAN_POINT('Ctrl Pts',(-9.87479817067687,-4.91593144188893,
1.35396723904141));
#50396=CARTESIAN_POINT('Ctrl Pts',(-9.80884152590359,-4.92809314710804,
-0.00411155299795817));
#50397=CARTESIAN_POINT('Origin',(-14.75,0.,0.));
#50398=CARTESIAN_POINT('',(-8.09115847409641,-4.93134763236354,0.00268789096151988));
#50399=CARTESIAN_POINT('',(-8.3088415259036,-4.93058250867777,0.00315514943839852));
#50400=CARTESIAN_POINT('',(-14.75,-4.925,-6.03138548580071E-16));
#50401=CARTESIAN_POINT('Ctrl Pts',(-8.09115847409641,-4.93134763236354,
0.00268789096151988));
#50402=CARTESIAN_POINT('Ctrl Pts',(-8.09866585408217,-4.93236070319556,
0.157002391239283));
#50403=CARTESIAN_POINT('Ctrl Pts',(-8.10617323406794,-4.92574782328456,
0.311228913952019));
#50404=CARTESIAN_POINT('Ctrl Pts',(-8.11368061405371,-4.91122550856618,
0.464707034867637));
#50405=CARTESIAN_POINT('Ctrl Pts',(-8.19322650242678,-4.7573515302013,2.09091398019483));
#50406=CARTESIAN_POINT('Ctrl Pts',(-8.27277239079985,-3.71549562387871,
3.63309883205044));
#50407=CARTESIAN_POINT('Ctrl Pts',(-8.35231827917293,-2.2642486452318,4.38283774475274));
#50408=CARTESIAN_POINT('Ctrl Pts',(-8.431864167546,-0.813001666584828,5.13257665745506));
#50409=CARTESIAN_POINT('Ctrl Pts',(-8.51141005591908,1.0476363843865,5.089869631004));
#50410=CARTESIAN_POINT('Ctrl Pts',(-8.59095594429216,2.46295580028325,4.27433472602514));
#50411=CARTESIAN_POINT('Ctrl Pts',(-8.67050183266523,3.87827521617993,3.45879982104632));
#50412=CARTESIAN_POINT('Ctrl Pts',(-8.75004772103831,4.84827599700209,1.87043703753978));
#50413=CARTESIAN_POINT('Ctrl Pts',(-8.82959360941138,4.9273749283692,0.238882689898267));
#50414=CARTESIAN_POINT('Ctrl Pts',(-8.90913949778446,5.0064738597363,-1.39267165774325));
#50415=CARTESIAN_POINT('Ctrl Pts',(-8.98868538615753,4.19467094164835,-3.06741756951973));
#50416=CARTESIAN_POINT('Ctrl Pts',(-9.0682312745306,2.86487902205042,-4.01603745167696));
#50417=CARTESIAN_POINT('Ctrl Pts',(-9.14777716290368,1.53508710245243,-4.96465733383422));
#50418=CARTESIAN_POINT('Ctrl Pts',(-9.22732305127675,-0.312693818655589,
-5.18715118637216));
#50419=CARTESIAN_POINT('Ctrl Pts',(-9.30686893964983,-1.82966013350537,
-4.58131339466273));
#50420=CARTESIAN_POINT('Ctrl Pts',(-9.38641482802291,-3.3466264483551,-3.97547560295332));
#50421=CARTESIAN_POINT('Ctrl Pts',(-9.46596071639599,-4.53277815694662,
-2.54130616699661));
#50422=CARTESIAN_POINT('Ctrl Pts',(-9.54550660476906,-4.84324014009708,
-0.937610563937788));
#50423=CARTESIAN_POINT('Ctrl Pts',(-9.56072389454484,-4.9026321471334,-0.630820342557176));
#50424=CARTESIAN_POINT('Ctrl Pts',(-9.57594118432063,-4.9299770049327,-0.317826062571257));
#50425=CARTESIAN_POINT('Ctrl Pts',(-9.59115847409641,-4.92709248349153,
-0.00433039759252629));
#50426=CARTESIAN_POINT('Ctrl Pts',(-9.80884152590359,-4.92809314710804,
-0.00411155299795817));
#50427=CARTESIAN_POINT('Ctrl Pts',(-9.7952522823038,-4.93059885938888,-0.283920563844114));
#50428=CARTESIAN_POINT('Ctrl Pts',(-9.781663038704,-4.90882931597747,-0.563339710114124));
#50429=CARTESIAN_POINT('Ctrl Pts',(-9.7680737951042,-4.86140717526349,-0.838335142623281));
#50430=CARTESIAN_POINT('Ctrl Pts',(-9.68852790673113,-4.58381730913562,
-2.44804622159789));
#50431=CARTESIAN_POINT('Ctrl Pts',(-9.60898201835805,-3.42725299792094,
-3.90618078368793));
#50432=CARTESIAN_POINT('Ctrl Pts',(-9.52943612998497,-1.9229979824355,-4.54292464108855));
#50433=CARTESIAN_POINT('Ctrl Pts',(-9.4498902416119,-0.418742966950077,
-5.17966849848915));
#50434=CARTESIAN_POINT('Ctrl Pts',(-9.37034435323882,1.43320275280612,-4.99502165120035));
#50435=CARTESIAN_POINT('Ctrl Pts',(-9.29079846486575,2.78212241146185,-4.07380417088284));
#50436=CARTESIAN_POINT('Ctrl Pts',(-9.21125257649268,4.1310420701176,-3.15258669056531));
#50437=CARTESIAN_POINT('Ctrl Pts',(-9.13170668811961,4.97693566767287,-1.49479857721911));
#50438=CARTESIAN_POINT('Ctrl Pts',(-9.05216079974653,4.93123033318249,0.138032373598989));
#50439=CARTESIAN_POINT('Ctrl Pts',(-8.97261491137345,4.8855249986921,1.77086332441709));
#50440=CARTESIAN_POINT('Ctrl Pts',(-8.89306902300037,3.94822073215603,3.37873711270705));
#50441=CARTESIAN_POINT('Ctrl Pts',(-8.8135231346273,2.54988115392759,4.22305477538536));
#50442=CARTESIAN_POINT('Ctrl Pts',(-8.73397724625422,1.15154157569918,5.06737243806365));
#50443=CARTESIAN_POINT('Ctrl Pts',(-8.65443135788115,-0.707833314221602,
5.14813397513033));
#50444=CARTESIAN_POINT('Ctrl Pts',(-8.57488546950808,-2.17411405885781,
4.428240462547));
#50445=CARTESIAN_POINT('Ctrl Pts',(-8.495339581135,-3.64039480349401,3.70834694996368));
#50446=CARTESIAN_POINT('Ctrl Pts',(-8.41579369276192,-4.71358140284566,
2.18779838773033));
#50447=CARTESIAN_POINT('Ctrl Pts',(-8.33624780438885,-4.90069081604919,
0.565079693981939));
#50448=CARTESIAN_POINT('Ctrl Pts',(-8.3271123782271,-4.92217934629819,0.378719001918263));
#50449=CARTESIAN_POINT('Ctrl Pts',(-8.31797695206535,-4.93198112784769,
0.191010756085821));
#50450=CARTESIAN_POINT('Ctrl Pts',(-8.3088415259036,-4.93058250867777,0.00315514943839852));
#50451=CARTESIAN_POINT('Origin',(-14.75,0.,0.));
#50452=CARTESIAN_POINT('',(-6.5911584740964,-4.91874206214364,0.00300395193210873));
#50453=CARTESIAN_POINT('',(-6.8088415259036,-4.91816702752264,0.00255975366377111));
#50454=CARTESIAN_POINT('',(-14.75,-4.925,-6.03138548580071E-16));
#50455=CARTESIAN_POINT('Ctrl Pts',(-6.5911584740964,-4.91874206214364,0.00300395193210873));
#50456=CARTESIAN_POINT('Ctrl Pts',(-6.62139052384371,-4.92221047690888,
0.628510441243254));
#50457=CARTESIAN_POINT('Ctrl Pts',(-6.65162257359103,-4.81164202146414,
1.2528364358832));
#50458=CARTESIAN_POINT('Ctrl Pts',(-6.68185462333834,-4.5814231074921,1.8293853978311));
#50459=CARTESIAN_POINT('Ctrl Pts',(-6.76140051171141,-3.97567628631209,
3.34638804078933));
#50460=CARTESIAN_POINT('Ctrl Pts',(-6.84094640008449,-2.54157798418442,
4.53262575168735));
#50461=CARTESIAN_POINT('Ctrl Pts',(-6.92049228845757,-0.937901001819111,
4.8431839047693));
#50462=CARTESIAN_POINT('Ctrl Pts',(-7.00003817683064,0.665775980546221,
5.15374205785124));
#50463=CARTESIAN_POINT('Ctrl Pts',(-7.07958406520371,2.43903164314918,4.58862065311707));
#50464=CARTESIAN_POINT('Ctrl Pts',(-7.15912995357679,3.5672965817681,3.40741598897341));
#50465=CARTESIAN_POINT('Ctrl Pts',(-7.23867584194987,4.69556152038701,2.22621132482977));
#50466=CARTESIAN_POINT('Ctrl Pts',(-7.31822173032295,5.17883573502188,0.428923401276672));
#50467=CARTESIAN_POINT('Ctrl Pts',(-7.39776761869602,4.79512056112791,-1.15883882763304));
#50468=CARTESIAN_POINT('Ctrl Pts',(-7.4773135070691,4.41140538723394,-2.74660105654276));
#50469=CARTESIAN_POINT('Ctrl Pts',(-7.55685939544217,3.16070082481106,-4.12483759080913));
#50470=CARTESIAN_POINT('Ctrl Pts',(-7.63640528381525,1.61753523524406,-4.66043650177258));
#50471=CARTESIAN_POINT('Ctrl Pts',(-7.71595117218832,0.0743696456770546,
-5.19603541273603));
#50472=CARTESIAN_POINT('Ctrl Pts',(-7.7954970605614,-1.76125697103409,-4.88899670039663));
#50473=CARTESIAN_POINT('Ctrl Pts',(-7.87504294893448,-3.04612425418612,
-3.88036282482753));
#50474=CARTESIAN_POINT('Ctrl Pts',(-7.94708145732179,-4.20972836304737,
-2.96692177349214));
#50475=CARTESIAN_POINT('Ctrl Pts',(-8.0191199657091,-4.92162651637264,-1.47806657246253));
#50476=CARTESIAN_POINT('Ctrl Pts',(-8.09115847409641,-4.93134763236354,
0.00268789096151988));
#50477=CARTESIAN_POINT('Ctrl Pts',(-8.3088415259036,-4.93058250867777,0.00315514943839852));
#50478=CARTESIAN_POINT('Ctrl Pts',(-8.23843106369227,-4.91980277925207,
-1.44472476977317));
#50479=CARTESIAN_POINT('Ctrl Pts',(-8.16802060148095,-4.24367279446414,
-2.90135853255996));
#50480=CARTESIAN_POINT('Ctrl Pts',(-8.09761013926962,-3.12486796763837,
-3.8172353503401));
#50481=CARTESIAN_POINT('Ctrl Pts',(-8.01806425089654,-1.86090347896865,
-4.85194287565023));
#50482=CARTESIAN_POINT('Ctrl Pts',(-7.93851836252347,-0.0319422745738374,
-5.19646910100704));
#50483=CARTESIAN_POINT('Ctrl Pts',(-7.85897247415039,1.52185713377351,-4.69255116109043));
#50484=CARTESIAN_POINT('Ctrl Pts',(-7.77942658577732,3.07565654212083,-4.18863322117384));
#50485=CARTESIAN_POINT('Ctrl Pts',(-7.69988069740424,4.35429415442072,-2.83627111598379));
#50486=CARTESIAN_POINT('Ctrl Pts',(-7.62033480903117,4.77041017820713,-1.25669099889733));
#50487=CARTESIAN_POINT('Ctrl Pts',(-7.54078892065809,5.18652620199355,0.322889118189166));
#50488=CARTESIAN_POINT('Ctrl Pts',(-7.46124303228501,4.7401206372665,2.12968724717213));
#50489=CARTESIAN_POINT('Ctrl Pts',(-7.38169714391194,3.63625602663207,3.33372579013805));
#50490=CARTESIAN_POINT('Ctrl Pts',(-7.30215125553886,2.53239141599764,4.53776433310397));
#50491=CARTESIAN_POINT('Ctrl Pts',(-7.22260536716579,0.771067759455849,
5.13904329005283));
#50492=CARTESIAN_POINT('Ctrl Pts',(-7.14305947879271,-0.838626670106471,
4.86135689322456));
#50493=CARTESIAN_POINT('Ctrl Pts',(-7.06351359041964,-2.44832109966874,
4.58367049639629));
#50494=CARTESIAN_POINT('Ctrl Pts',(-6.98396770204656,-3.90638630225154,
3.42701874579095));
#50495=CARTESIAN_POINT('Ctrl Pts',(-6.90442181367349,-4.54303995130782,
1.92272554874775));
#50496=CARTESIAN_POINT('Ctrl Pts',(-6.87256171775019,-4.79803548588176,
1.32021891346095));
#50497=CARTESIAN_POINT('Ctrl Pts',(-6.8407016218269,-4.92126012648956,0.661943615096396));
#50498=CARTESIAN_POINT('Ctrl Pts',(-6.8088415259036,-4.91816702752264,0.00255975366377111));
#50499=CARTESIAN_POINT('Origin',(-14.75,0.,0.));
#50500=CARTESIAN_POINT('',(-5.0911584740964,-4.92034850444268,-0.00382654489779644));
#50501=CARTESIAN_POINT('',(-5.30884152590359,-4.92118977299025,-0.00410386901592228));
#50502=CARTESIAN_POINT('',(-14.75,-4.925,-6.03138548580071E-16));
#50503=CARTESIAN_POINT('Ctrl Pts',(-5.0911584740964,-4.92034850444268,-0.00382654489779644));
#50504=CARTESIAN_POINT('Ctrl Pts',(-5.14411519360526,-4.91244809502025,
1.09095932864311));
#50505=CARTESIAN_POINT('Ctrl Pts',(-5.19707191311412,-4.55198007497204,
2.19046632634003));
#50506=CARTESIAN_POINT('Ctrl Pts',(-5.25002863262299,-3.88054548599257,
3.0458915476704));
#50507=CARTESIAN_POINT('Ctrl Pts',(-5.32957452099606,-2.87198866147391,
4.3308193112958));
#50508=CARTESIAN_POINT('Ctrl Pts',(-5.40912040936913,-1.16180365248812,
5.06502982514693));
#50509=CARTESIAN_POINT('Ctrl Pts',(-5.4886662977422,0.464412516539281,4.91125336903979));
#50510=CARTESIAN_POINT('Ctrl Pts',(-5.56821218611528,2.09062868556668,4.75747691293265));
#50511=CARTESIAN_POINT('Ctrl Pts',(-5.64775807448836,3.63287601463573,3.71571348686722));
#50512=CARTESIAN_POINT('Ctrl Pts',(-5.72730396286143,4.38270195487139,2.26451147037829));
#50513=CARTESIAN_POINT('Ctrl Pts',(-5.80684985123451,5.13252789510707,0.813309453889311));
#50514=CARTESIAN_POINT('Ctrl Pts',(-5.88639573960759,5.08993244650934,-1.04733115302316));
#50515=CARTESIAN_POINT('Ctrl Pts',(-5.96594162798066,4.27448241666476,-2.46269947196908));
#50516=CARTESIAN_POINT('Ctrl Pts',(-6.04548751635374,3.45903238682021,-3.87806779091495));
#50517=CARTESIAN_POINT('Ctrl Pts',(-6.12503340472681,1.87072777572881,-4.84816382189425));
#50518=CARTESIAN_POINT('Ctrl Pts',(-6.20457929309989,0.239178174554097,
-4.92736059443231));
#50519=CARTESIAN_POINT('Ctrl Pts',(-6.28412518147296,-1.39237142662062,
-5.00655736697037));
#50520=CARTESIAN_POINT('Ctrl Pts',(-6.36367106984604,-3.06716601787869,
-4.19485488106719));
#50521=CARTESIAN_POINT('Ctrl Pts',(-6.44321695821912,-4.01586564339155,
-2.86511985060641));
#50522=CARTESIAN_POINT('Ctrl Pts',(-6.49253079684488,-4.604004404473,-2.04076123134479));
#50523=CARTESIAN_POINT('Ctrl Pts',(-6.54184463547064,-4.91308446209832,
-1.01730814503372));
#50524=CARTESIAN_POINT('Ctrl Pts',(-6.5911584740964,-4.91874206214364,0.00300395193210873));
#50525=CARTESIAN_POINT('Ctrl Pts',(-6.8088415259036,-4.91816702752264,0.00255975366377111));
#50526=CARTESIAN_POINT('Ctrl Pts',(-6.76115573345382,-4.91353750990542,
-0.984356357220146));
#50527=CARTESIAN_POINT('Ctrl Pts',(-6.71346994100404,-4.62593290938502,
-1.97375585426302));
#50528=CARTESIAN_POINT('Ctrl Pts',(-6.66578414855426,-4.07363732517796,
-2.78236670443132));
#50529=CARTESIAN_POINT('Ctrl Pts',(-6.58623826018119,-3.15233895446205,
-4.13123111708606));
#50530=CARTESIAN_POINT('Ctrl Pts',(-6.5066923718081,-1.49450011750048,-4.97702529891446));
#50531=CARTESIAN_POINT('Ctrl Pts',(-6.42714648343503,0.138328089510376,
-4.93122204682461));
#50532=CARTESIAN_POINT('Ctrl Pts',(-6.34760059506195,1.77115629652118,-4.88541879473476));
#50533=CARTESIAN_POINT('Ctrl Pts',(-6.26805470668888,3.37897387358129,-3.94801810872673));
#50534=CARTESIAN_POINT('Ctrl Pts',(-6.18850881831581,4.22320767910246,-2.54962790101466));
#50535=CARTESIAN_POINT('Ctrl Pts',(-6.10896292994273,5.06744148462366,-1.15123769330255));
#50536=CARTESIAN_POINT('Ctrl Pts',(-6.02941704156966,5.14809151860588,0.708142036113649));
#50537=CARTESIAN_POINT('Ctrl Pts',(-5.94987115319658,4.42811007730965,2.17437960764566));
#50538=CARTESIAN_POINT('Ctrl Pts',(-5.8703252648235,3.70812863601341,3.64061717917766));
#50539=CARTESIAN_POINT('Ctrl Pts',(-5.79077937645043,2.18751571943878,4.71371259282546));
#50540=CARTESIAN_POINT('Ctrl Pts',(-5.71123348807735,0.564785808115402,
4.9007246942176));
#50541=CARTESIAN_POINT('Ctrl Pts',(-5.63168759970428,-1.05794410320798,
5.08773679560975));
#50542=CARTESIAN_POINT('Ctrl Pts',(-5.5521417113312,-2.78279100928007,4.38866558474619));
#50543=CARTESIAN_POINT('Ctrl Pts',(-5.47259582295812,-3.81742273544663,
3.1246390494413));
#50544=CARTESIAN_POINT('Ctrl Pts',(-5.41801105727328,-4.5273919305612,2.25725804886157));
#50545=CARTESIAN_POINT('Ctrl Pts',(-5.36342629158844,-4.9123547098068,1.12385261058705));
#50546=CARTESIAN_POINT('Ctrl Pts',(-5.30884152590359,-4.92118977299025,
-0.00410386901592228));
#50547=CARTESIAN_POINT('Origin',(-14.75,0.,0.));
#50548=CARTESIAN_POINT('',(-3.5911584740964,-4.93263795678916,-0.00146375725000258));
#50549=CARTESIAN_POINT('',(-3.80884152590359,-4.93297963225018,-0.000859328946059894));
#50550=CARTESIAN_POINT('',(-14.75,-4.925,-6.03138548580071E-16));
#50551=CARTESIAN_POINT('Ctrl Pts',(-3.5911584740964,-4.93263795678916,-0.00146375725000258));
#50552=CARTESIAN_POINT('Ctrl Pts',(-3.66683986336681,-4.9265598841513,1.55309257837791));
#50553=CARTESIAN_POINT('Ctrl Pts',(-3.74252125263721,-4.13044035554753,
3.11300803879703));
#50554=CARTESIAN_POINT('Ctrl Pts',(-3.81820264190762,-2.8653605731944,4.01569365331712));
#50555=CARTESIAN_POINT('Ctrl Pts',(-3.8977485302807,-1.53568235084381,4.96447286866741));
#50556=CARTESIAN_POINT('Ctrl Pts',(-3.97729441865377,0.31207168483266,5.18718866129924));
#50557=CARTESIAN_POINT('Ctrl Pts',(-4.05684030702685,1.82911060574424,4.58153289102084));
#50558=CARTESIAN_POINT('Ctrl Pts',(-4.13638619539992,3.34614952665579,3.97587712074245));
#50559=CARTESIAN_POINT('Ctrl Pts',(-4.215932083773,4.53247333280247,2.54184978755386));
#50560=CARTESIAN_POINT('Ctrl Pts',(-4.29547797214607,4.84312767798418,0.938191390916231));
#50561=CARTESIAN_POINT('Ctrl Pts',(-4.37502386051915,5.15378202316589,-0.665467005721419));
#50562=CARTESIAN_POINT('Ctrl Pts',(-4.45456974889223,4.58876690738262,-2.43875646580811));
#50563=CARTESIAN_POINT('Ctrl Pts',(-4.53411563726531,3.40762989303727,-3.56709221570014));
#50564=CARTESIAN_POINT('Ctrl Pts',(-4.61366152563838,2.22649287869195,-4.69542796559215));
#50565=CARTESIAN_POINT('Ctrl Pts',(-4.69320741401145,0.429233965784571,
-5.17881000528951));
#50566=CARTESIAN_POINT('Ctrl Pts',(-4.77275330238453,-1.15855126458436,
-4.79519005809945));
#50567=CARTESIAN_POINT('Ctrl Pts',(-4.8522991907576,-2.74633649495327,-4.4115701109094));
#50568=CARTESIAN_POINT('Ctrl Pts',(-4.93184507913068,-4.12464804278375,
-3.16094817683195));
#50569=CARTESIAN_POINT('Ctrl Pts',(-5.01139096750375,-4.66033949667325,
-1.6178147030934));
#50570=CARTESIAN_POINT('Ctrl Pts',(-5.03798013636797,-4.83940080100846,
-1.10200380007321));
#50571=CARTESIAN_POINT('Ctrl Pts',(-5.06456930523218,-4.92431524033904,
-0.553510262690519));
#50572=CARTESIAN_POINT('Ctrl Pts',(-5.0911584740964,-4.92034850444268,-0.00382654489779644));
#50573=CARTESIAN_POINT('Ctrl Pts',(-5.30884152590359,-4.92118977299025,
-0.00410386901592228));
#50574=CARTESIAN_POINT('Ctrl Pts',(-5.28388040321536,-4.92522996796614,
-0.519908227999806));
#50575=CARTESIAN_POINT('Ctrl Pts',(-5.25891928052713,-4.85061618972318,
-1.03457312761624));
#50576=CARTESIAN_POINT('Ctrl Pts',(-5.2339581578389,-4.69245989025258,-1.52213853308082));
#50577=CARTESIAN_POINT('Ctrl Pts',(-5.15441226946583,-4.18844877263093,
-3.07590772055185));
#50578=CARTESIAN_POINT('Ctrl Pts',(-5.07486638109275,-2.83600999112659,
-4.35446423574767));
#50579=CARTESIAN_POINT('Ctrl Pts',(-4.99532049271967,-1.25640492385531,
-4.77048553279394));
#50580=CARTESIAN_POINT('Ctrl Pts',(-4.9157746043466,0.323200143415984,-5.18650682984021));
#50581=CARTESIAN_POINT('Ctrl Pts',(-4.83622871597352,2.1299714964542,-4.73999290873692));
#50582=CARTESIAN_POINT('Ctrl Pts',(-4.75668282760045,3.33394384188576,-3.63605609952002));
#50583=CARTESIAN_POINT('Ctrl Pts',(-4.67713693922737,4.53791618731733,-2.53211929030309));
#50584=CARTESIAN_POINT('Ctrl Pts',(-4.5975910508543,5.13908952514219,-0.770759592972526));
#50585=CARTESIAN_POINT('Ctrl Pts',(-4.51804516248122,4.86130659629173,0.83891818762146));
#50586=CARTESIAN_POINT('Ctrl Pts',(-4.43849927410815,4.58352366744127,2.44859596821542));
#50587=CARTESIAN_POINT('Ctrl Pts',(-4.35895338573507,3.42678447191547,3.90659183207286));
#50588=CARTESIAN_POINT('Ctrl Pts',(-4.27940749736199,1.92245310317772,4.54315525853296));
#50589=CARTESIAN_POINT('Ctrl Pts',(-4.19986160898891,0.418121734439937,
5.17971868499307));
#50590=CARTESIAN_POINT('Ctrl Pts',(-4.12031572061584,-1.43380180750975,
4.99484967405592));
#50591=CARTESIAN_POINT('Ctrl Pts',(-4.04076983224277,-2.78261097786045,
4.07347043921392));
#50592=CARTESIAN_POINT('Ctrl Pts',(-3.96346039679638,-4.09349803459511,
3.17799601640553));
#50593=CARTESIAN_POINT('Ctrl Pts',(-3.88615096134998,-4.92916340173032,
1.58684352759606));
#50594=CARTESIAN_POINT('Ctrl Pts',(-3.80884152590359,-4.93297963225018,
-0.000859328946059894));
#50595=CARTESIAN_POINT('Origin',(-14.75,0.,0.));
#50596=CARTESIAN_POINT('',(-2.09115847409639,-4.92479967433243,0.00455076259524401));
#50597=CARTESIAN_POINT('',(-2.3088415259036,-4.92378694620037,0.00452865572044409));
#50598=CARTESIAN_POINT('',(-14.75,-4.925,-6.03138548580071E-16));
#50599=CARTESIAN_POINT('Ctrl Pts',(-2.09115847409639,-4.92479967433243,
0.00455076259524401));
#50600=CARTESIAN_POINT('Ctrl Pts',(-2.11001864475527,-4.92838960899571,
0.393565332838783));
#50601=CARTESIAN_POINT('Ctrl Pts',(-2.12887881541415,-4.8861997157664,0.781810208141141));
#50602=CARTESIAN_POINT('Ctrl Pts',(-2.14773898607303,-4.79526872833564,
1.15827977445631));
#50603=CARTESIAN_POINT('Ctrl Pts',(-2.22728487444611,-4.41175225297358,
2.74610242143037));
#50604=CARTESIAN_POINT('Ctrl Pts',(-2.30683076281919,-3.16119502426286,
4.12445761712042));
#50605=CARTESIAN_POINT('Ctrl Pts',(-2.38637665119226,-1.61808937757221,
4.66023409988841));
#50606=CARTESIAN_POINT('Ctrl Pts',(-2.46592253956534,-0.0749837308815521,
5.19601058265641));
#50607=CARTESIAN_POINT('Ctrl Pts',(-2.54546842793841,1.76067033378902,4.88920835250233));
#50608=CARTESIAN_POINT('Ctrl Pts',(-2.62501431631149,3.04565633625721,3.88073249588954));
#50609=CARTESIAN_POINT('Ctrl Pts',(-2.70456020468456,4.33064233872542,2.87225663927674));
#50610=CARTESIAN_POINT('Ctrl Pts',(-2.78410609305764,5.06496027899121,1.16210715620522));
#50611=CARTESIAN_POINT('Ctrl Pts',(-2.86365198143071,4.91128251100273,-0.464120269161797));
#50612=CARTESIAN_POINT('Ctrl Pts',(-2.94319786980379,4.75760474301426,-2.09034769452876));
#50613=CARTESIAN_POINT('Ctrl Pts',(-3.02274375817687,3.71593126677153,-3.63265306219127));
#50614=CARTESIAN_POINT('Ctrl Pts',(-3.10228964654994,2.26477361062453,-4.38256496537029));
#50615=CARTESIAN_POINT('Ctrl Pts',(-3.18183553492302,0.813615954477467,
-5.13247686854935));
#50616=CARTESIAN_POINT('Ctrl Pts',(-3.26138142329609,-1.04702588157384,
-5.08999530724491));
#50617=CARTESIAN_POINT('Ctrl Pts',(-3.34092731166917,-2.46244278226107,
-4.27463070863102));
#50618=CARTESIAN_POINT('Ctrl Pts',(-3.42047320004224,-3.87785968294825,
-3.45926611001717));
#50619=CARTESIAN_POINT('Ctrl Pts',(-3.50001908841532,-4.84805164827134,
-1.87101847409385));
#50620=CARTESIAN_POINT('Ctrl Pts',(-3.57956497678839,-4.92734642642051,
-0.239473337097873));
#50621=CARTESIAN_POINT('Ctrl Pts',(-3.58342947589106,-4.93119872608391,
-0.160209595792822));
#50622=CARTESIAN_POINT('Ctrl Pts',(-3.58729397499373,-4.93294831983193,
-0.0808436632215555));
#50623=CARTESIAN_POINT('Ctrl Pts',(-3.5911584740964,-4.93263795678916,-0.00146375725000258));
#50624=CARTESIAN_POINT('Ctrl Pts',(-3.80884152590359,-4.93297963225018,
-0.000859328946059894));
#50625=CARTESIAN_POINT('Ctrl Pts',(-3.80660507297691,-4.93309003041654,
-0.0467893332167884));
#50626=CARTESIAN_POINT('Ctrl Pts',(-3.80436862005022,-4.93250428457465,
-0.0927164506168972));
#50627=CARTESIAN_POINT('Ctrl Pts',(-3.80213216712354,-4.93121376103269,
-0.138623755771863));
#50628=CARTESIAN_POINT('Ctrl Pts',(-3.72258627875046,-4.8853125751026,-1.77144925716878));
#50629=CARTESIAN_POINT('Ctrl Pts',(-3.64304039037739,-3.94781540449082,
-3.37921080121581));
#50630=CARTESIAN_POINT('Ctrl Pts',(-3.56349450200431,-2.54937460381079,
-4.2233606619699));
#50631=CARTESIAN_POINT('Ctrl Pts',(-3.48394861363124,-1.15093380313076,
-5.06751052272398));
#50632=CARTESIAN_POINT('Ctrl Pts',(-3.40440272525816,0.708450627617543,
-5.14804870018514));
#50633=CARTESIAN_POINT('Ctrl Pts',(-3.32485683688509,2.17464508120495,-4.42797949508699));
#50634=CARTESIAN_POINT('Ctrl Pts',(-3.24531094851201,3.64083953479237,-3.70791028998884));
#50635=CARTESIAN_POINT('Ctrl Pts',(-3.16576506013894,4.71384401121892,-2.18723370233138));
#50636=CARTESIAN_POINT('Ctrl Pts',(-3.08621917176586,4.90075868413978,-0.564492267726287));
#50637=CARTESIAN_POINT('Ctrl Pts',(-3.00667328339279,5.08767335706064,1.05824916687883));
#50638=CARTESIAN_POINT('Ctrl Pts',(-2.92712739501971,4.38849822647583,2.78305544843154));
#50639=CARTESIAN_POINT('Ctrl Pts',(-2.84758150664664,3.12440987169467,3.8176107737941));
#50640=CARTESIAN_POINT('Ctrl Pts',(-2.76803561827356,1.86032151691353,4.85216609915665));
#50641=CARTESIAN_POINT('Ctrl Pts',(-2.68848972990048,0.0313199379360557,
5.19647046832902));
#50642=CARTESIAN_POINT('Ctrl Pts',(-2.60894384152741,-1.5224194503301,4.69236732243377));
#50643=CARTESIAN_POINT('Ctrl Pts',(-2.52939795315433,-3.07615883859628,
4.18826417653852));
#50644=CARTESIAN_POINT('Ctrl Pts',(-2.44985206478126,-4.35463603615115,
2.8357535155756));
#50645=CARTESIAN_POINT('Ctrl Pts',(-2.37030617640818,-4.77056178492771,
1.25612130118806));
#50646=CARTESIAN_POINT('Ctrl Pts',(-2.34981795957332,-4.87768959633853,
0.849263725144446));
#50647=CARTESIAN_POINT('Ctrl Pts',(-2.32932974273846,-4.92759608937386,
0.427338996020449));
#50648=CARTESIAN_POINT('Ctrl Pts',(-2.3088415259036,-4.92378694620037,0.00452865572044409));
#50649=CARTESIAN_POINT('Origin',(-14.75,0.,0.));
#50650=CARTESIAN_POINT('',(-0.591158474096391,-4.91621514884034,-0.00190685489401573));
#50651=CARTESIAN_POINT('',(-0.808841525903593,-4.91703434725887,-0.0013692803956027));
#50652=CARTESIAN_POINT('',(-14.75,-4.925,-6.03138548580071E-16));
#50653=CARTESIAN_POINT('Ctrl Pts',(-0.591158474096391,-4.91617236260859,
-0.00191614214703012));
#50654=CARTESIAN_POINT('Ctrl Pts',(-0.632743314516819,-4.91557730725517,
0.859927749670198));
#50655=CARTESIAN_POINT('Ctrl Pts',(-0.674328154937247,-4.70120063118156,
1.72260089528099));
#50656=CARTESIAN_POINT('Ctrl Pts',(-0.715912995357675,-4.27522171387068,
2.46297048332456));
#50657=CARTESIAN_POINT('Ctrl Pts',(-0.795458883730751,-3.46038459863554,
3.87919226053746));
#50658=CARTESIAN_POINT('Ctrl Pts',(-0.875004772103829,-1.87128956129306,
4.84790224489492));
#50659=CARTESIAN_POINT('Ctrl Pts',(-0.954550660476906,-0.23953077630217,
4.92691531448512));
#50660=CARTESIAN_POINT('Ctrl Pts',(-1.03409654884998,1.39222800868875,5.00592838407533));
#50661=CARTESIAN_POINT('Ctrl Pts',(-1.11364243722306,3.06665054132806,4.19524453889832));
#50662=CARTESIAN_POINT('Ctrl Pts',(-1.19318832559614,4.01539704249259,2.86581937781023));
#50663=CARTESIAN_POINT('Ctrl Pts',(-1.27273421396921,4.96414354365708,1.53639421672219));
#50664=CARTESIAN_POINT('Ctrl Pts',(-1.35228010234228,5.1872140133468,-0.311772260276884));
#50665=CARTESIAN_POINT('Ctrl Pts',(-1.43182599071535,4.58170765220235,-1.82894951483846));
#50666=CARTESIAN_POINT('Ctrl Pts',(-1.51137187908843,3.9762012910579,-3.34612676940009));
#50667=CARTESIAN_POINT('Ctrl Pts',(-1.59091776746151,2.54211809907922,-4.53231480152423));
#50668=CARTESIAN_POINT('Ctrl Pts',(-1.67046365583459,0.938447910619046,
-4.84301219015054));
#50669=CARTESIAN_POINT('Ctrl Pts',(-1.75000954420766,-0.665222277841155,
-5.15370957877686));
#50670=CARTESIAN_POINT('Ctrl Pts',(-1.82955543258074,-2.43847946278283,
-4.58891632390535));
#50671=CARTESIAN_POINT('Ctrl Pts',(-1.90910132095381,-3.56687019424698,
-3.40787464734053));
#50672=CARTESIAN_POINT('Ctrl Pts',(-1.96978703866801,-4.42772174548972,
-2.50685558452536));
#50673=CARTESIAN_POINT('Ctrl Pts',(-2.0304727563822,-4.91324846594047,-1.24716794257944));
#50674=CARTESIAN_POINT('Ctrl Pts',(-2.09115847409639,-4.92479967433243,
0.00455076259524401));
#50675=CARTESIAN_POINT('Ctrl Pts',(-2.3088415259036,-4.92378694620037,0.00452865572044409));
#50676=CARTESIAN_POINT('Ctrl Pts',(-2.24978385436538,-4.912807019143,-1.21423012654258));
#50677=CARTESIAN_POINT('Ctrl Pts',(-2.19072618282717,-4.45550843625236,
-2.44034737679679));
#50678=CARTESIAN_POINT('Ctrl Pts',(-2.13166851128896,-3.63585440375436,
-3.33416659713051));
#50679=CARTESIAN_POINT('Ctrl Pts',(-2.05212262291588,-2.53184697380615,
-4.53806851324942));
#50680=CARTESIAN_POINT('Ctrl Pts',(-1.9725767345428,-0.770457813911437,
-5.13911857767506));
#50681=CARTESIAN_POINT('Ctrl Pts',(-1.89303084616973,0.839206332661352,
-4.86124723150085));
#50682=CARTESIAN_POINT('Ctrl Pts',(-1.81348495779665,2.4488704792341,-4.58337588532665));
#50683=CARTESIAN_POINT('Ctrl Pts',(-1.73393906942358,3.90680961248493,-3.42658312855265));
#50684=CARTESIAN_POINT('Ctrl Pts',(-1.65439318105051,4.54327701636474,-1.9221980209477));
#50685=CARTESIAN_POINT('Ctrl Pts',(-1.57484729267743,5.17974442024456,-0.417812913342702));
#50686=CARTESIAN_POINT('Ctrl Pts',(-1.49530140430435,4.99474009475331,1.43416454509326));
#50687=CARTESIAN_POINT('Ctrl Pts',(-1.41575551593128,4.0732911268349,2.78288857953561));
#50688=CARTESIAN_POINT('Ctrl Pts',(-1.3362096275582,3.15184215891648,4.13161261397798));
#50689=CARTESIAN_POINT('Ctrl Pts',(-1.25666373918512,1.49394854857088,4.97708322442672));
#50690=CARTESIAN_POINT('Ctrl Pts',(-1.17711785081204,-0.138895601305483,
4.93114147431309));
#50691=CARTESIAN_POINT('Ctrl Pts',(-1.09757196243897,-1.77173975118177,
4.88519972419945));
#50692=CARTESIAN_POINT('Ctrl Pts',(-1.0180260740659,-3.37953444058883,3.94784561352353));
#50693=CARTESIAN_POINT('Ctrl Pts',(-0.938480185692825,-4.22355933348682,
2.54924407639987));
#50694=CARTESIAN_POINT('Ctrl Pts',(-0.895267299096415,-4.6820714291754,
1.7894611277975));
#50695=CARTESIAN_POINT('Ctrl Pts',(-0.852054412500004,-4.91518370582573,
0.893557208022445));
#50696=CARTESIAN_POINT('Ctrl Pts',(-0.808841525903593,-4.91703434725887,
-0.0013692803956027));
#50697=CARTESIAN_POINT('Origin',(-32.3478126690739,0.,0.));
#50698=CARTESIAN_POINT('',(-0.0978126690738565,-4.06323934281354,-0.00157601073016207));
#50699=CARTESIAN_POINT('',(0.,-4.0705,-4.82875428449296E-13));
#50700=CARTESIAN_POINT('',(-32.3478126690739,-4.0705,-4.82875428449296E-13));
#50701=CARTESIAN_POINT('',(0.,-3.73359974356529,-1.6214817929441));
#50702=CARTESIAN_POINT('Ctrl Pts',(-0.0978126690738567,-4.06320398010117,
-0.00158368662129781));
#50703=CARTESIAN_POINT('Ctrl Pts',(-0.0652084460492417,-4.06358958070638,
-0.560065388179513));
#50704=CARTESIAN_POINT('Ctrl Pts',(-0.0326042230246268,-3.95536025262438,
-1.1181257750272));
#50705=CARTESIAN_POINT('Ctrl Pts',(-1.16714363868065E-14,-3.73764785372991,
-1.62671566533116));
#50706=CARTESIAN_POINT('Origin',(0.,0.,0.));
#50707=CARTESIAN_POINT('Origin',(-32.3478126690739,0.,0.));
#50708=CARTESIAN_POINT('',(-1.59781266907385,-4.07033443134419,0.00376119373461055));
#50709=CARTESIAN_POINT('',(-1.30218733092609,-4.06391640822685,-0.00113170677241647));
#50710=CARTESIAN_POINT('',(-32.3478126690739,-4.0705,-4.82875428449296E-13));
#50711=CARTESIAN_POINT('Ctrl Pts',(-1.59781266907385,-4.07033443134419,
0.00376119373461031));
#50712=CARTESIAN_POINT('Ctrl Pts',(-1.53712695135966,-4.06078738692598,
-1.0307811391412));
#50713=CARTESIAN_POINT('Ctrl Pts',(-1.3968953452724,-3.13350059127503,-3.43660489264461));
#50714=CARTESIAN_POINT('Ctrl Pts',(-1.17711785081205,0.915788038447374,
-4.72632807804377));
#50715=CARTESIAN_POINT('Ctrl Pts',(-0.938480185692821,4.47158639354322,
-1.78518388428051));
#50716=CARTESIAN_POINT('Ctrl Pts',(-0.699842520573601,3.91848486245357,
2.79733082310517));
#50717=CARTESIAN_POINT('Ctrl Pts',(-0.461204855454373,-0.233233057815519,
4.80741524450186));
#50718=CARTESIAN_POINT('Ctrl Pts',(-0.260528238287788,-3.54660683376317,
2.78758749144531));
#50719=CARTESIAN_POINT('Ctrl Pts',(-0.139397509494285,-4.06271216836188,
0.7107281025446));
#50720=CARTESIAN_POINT('Ctrl Pts',(-0.0978126690738567,-4.06320398010117,
-0.00158368662129781));
#50721=CARTESIAN_POINT('',(0.,-2.75129702511903,2.99988915288068));
#50722=CARTESIAN_POINT('Origin',(0.,0.,0.));
#50723=CARTESIAN_POINT('Ctrl Pts',(-1.30218733092609,-4.06391640822685,
-0.00113170677241654));
#50724=CARTESIAN_POINT('Ctrl Pts',(-1.26585432914943,-4.06520244032274,
-0.623026454755739));
#50725=CARTESIAN_POINT('Ctrl Pts',(-1.1499754389997,-3.63835675138479,-2.6046490156767));
#50726=CARTESIAN_POINT('Ctrl Pts',(-0.9545506604769,-0.551158953576692,
-4.78140835552346));
#50727=CARTESIAN_POINT('Ctrl Pts',(-0.715912995357679,3.72696190987269,
-3.05177387808086));
#50728=CARTESIAN_POINT('Ctrl Pts',(-0.477275330238447,4.57725222884596,
1.49154630755727));
#50729=CARTESIAN_POINT('Ctrl Pts',(-0.278410609305757,1.78830202401348,
4.11849926473408));
#50730=CARTESIAN_POINT('Ctrl Pts',(-0.119318832559607,-1.02190788268887,
4.1117895186236));
#50731=CARTESIAN_POINT('Ctrl Pts',(-0.0397729441865359,-2.25151393523441,
3.45825666525491));
#50732=CARTESIAN_POINT('Ctrl Pts',(0.,-2.75129702511903,2.99988915288068));
#50733=CARTESIAN_POINT('Origin',(-32.3478126690739,0.,0.));
#50734=CARTESIAN_POINT('',(-3.09781266907385,-4.07681275190056,-0.00120979165237837));
#50735=CARTESIAN_POINT('',(-2.8021873309261,-4.06949741411341,0.00374292245829216));
#50736=CARTESIAN_POINT('',(-32.3478126690739,-4.0705,-4.82875428449296E-13));
#50737=CARTESIAN_POINT('Ctrl Pts',(-3.09781266907385,-4.07681275190056,
-0.00120979165237874));
#50738=CARTESIAN_POINT('Ctrl Pts',(-3.09394816997118,-4.07706926616768,
-0.0668170824659285));
#50739=CARTESIAN_POINT('Ctrl Pts',(-3.01053778249544,-4.04585841086343,
-1.48261925960601));
#50740=CARTESIAN_POINT('Ctrl Pts',(-2.84758150664664,-2.40317998874982,
-4.17175730007125));
#50741=CARTESIAN_POINT('Ctrl Pts',(-2.60894384152741,2.21026727641583,-4.27709000786183));
#50742=CARTESIAN_POINT('Ctrl Pts',(-2.37030617640818,4.79308872923565,-0.452955592184536));
#50743=CARTESIAN_POINT('Ctrl Pts',(-2.13166851128895,2.97235298759993,3.78734702964848));
#50744=CARTESIAN_POINT('Ctrl Pts',(-1.89303084616973,-1.57913728868941,
4.54806082325786));
#50745=CARTESIAN_POINT('Ctrl Pts',(-1.71507889876469,-3.89136234884321,
1.99954296889815));
#50746=CARTESIAN_POINT('Ctrl Pts',(-1.61667283973273,-4.0733015032319,0.325280748694308));
#50747=CARTESIAN_POINT('Ctrl Pts',(-1.59781266907385,-4.07033443134419,
0.00376119373461031));
#50748=CARTESIAN_POINT('Ctrl Pts',(-2.8021873309261,-4.06949741411341,0.00374292245829196));
#50749=CARTESIAN_POINT('Ctrl Pts',(-2.7431296593879,-4.06042253226819,-1.00355811778553));
#50750=CARTESIAN_POINT('Ctrl Pts',(-2.60452609947661,-3.17339021123584,
-3.38188525686312));
#50751=CARTESIAN_POINT('Ctrl Pts',(-2.38637665119226,0.819002242401078,
-4.74423481374027));
#50752=CARTESIAN_POINT('Ctrl Pts',(-2.14773898607304,4.43395122223712,-1.87597598138563));
#50753=CARTESIAN_POINT('Ctrl Pts',(-1.90910132095381,3.97523440584382,2.71598802545506));
#50754=CARTESIAN_POINT('Ctrl Pts',(-1.67046365583458,-0.135500177452599,
4.81232596646912));
#50755=CARTESIAN_POINT('Ctrl Pts',(-1.46815899249201,-3.51506103565612,
2.84202137248833));
#50756=CARTESIAN_POINT('Ctrl Pts',(-1.34540021752251,-4.06238685777956,
0.738522764518305));
#50757=CARTESIAN_POINT('Ctrl Pts',(-1.30218733092609,-4.06391640822685,
-0.00113170677241654));
#50758=CARTESIAN_POINT('Origin',(-32.3478126690739,0.,0.));
#50759=CARTESIAN_POINT('',(-4.59781266907386,-4.0666555507277,-0.00316262964624325));
#50760=CARTESIAN_POINT('',(-4.30218733092609,-4.0770951458019,-0.000710233193596532));
#50761=CARTESIAN_POINT('',(-32.3478126690739,-4.0705,-4.82875428449296E-13));
#50762=CARTESIAN_POINT('Ctrl Pts',(-4.59781266907386,-4.0666555507277,-0.00316262964624277));
#50763=CARTESIAN_POINT('Ctrl Pts',(-4.57122350020965,-4.06993404787816,
-0.457474827265511));
#50764=CARTESIAN_POINT('Ctrl Pts',(-4.46508844297236,-3.78979273029454,
-2.26701044287803));
#50765=CARTESIAN_POINT('Ctrl Pts',(-4.27940749736198,-1.13066914665236,
-4.67978735413588));
#50766=CARTESIAN_POINT('Ctrl Pts',(-4.04076983224278,3.32562064318893,-3.48124526728007));
#50767=CARTESIAN_POINT('Ctrl Pts',(-3.80213216712354,4.72657132062792,0.915612446800854));
#50768=CARTESIAN_POINT('Ctrl Pts',(-3.56349450200431,1.78509047620951,4.4712723004521));
#50769=CARTESIAN_POINT('Ctrl Pts',(-3.32872133598775,-2.72220888913037,
3.92799287505321));
#50770=CARTESIAN_POINT('Ctrl Pts',(-3.17349405834426,-4.07178924029207,
1.28362707416973));
#50771=CARTESIAN_POINT('Ctrl Pts',(-3.09781266907385,-4.07681275190056,
-0.00120979165237874));
#50772=CARTESIAN_POINT('Ctrl Pts',(-4.30218733092609,-4.0770951458019,-0.000710233193597031));
#50773=CARTESIAN_POINT('Ctrl Pts',(-4.29995087799942,-4.07718638960619,
-0.038671265149509));
#50774=CARTESIAN_POINT('Ctrl Pts',(-4.21816853669967,-4.05948324093355,
-1.42673845965056));
#50775=CARTESIAN_POINT('Ctrl Pts',(-4.05684030702684,-2.48802037989938,
-4.12171998606955));
#50776=CARTESIAN_POINT('Ctrl Pts',(-3.81820264190762,2.12230915839156,-4.32141378384957));
#50777=CARTESIAN_POINT('Ctrl Pts',(-3.5795649767884,4.78281558760628,-0.550907763508576));
#50778=CARTESIAN_POINT('Ctrl Pts',(-3.34092731166917,3.04921617498962,3.72573627855867));
#50779=CARTESIAN_POINT('Ctrl Pts',(-3.10228964654994,-1.48577931367711,
4.57943634031457));
#50780=CARTESIAN_POINT('Ctrl Pts',(-2.92270965296892,-3.87125352580713,
2.05582519611215));
#50781=CARTESIAN_POINT('Ctrl Pts',(-2.82267554776097,-4.07264566127848,
0.35319459559373));
#50782=CARTESIAN_POINT('Ctrl Pts',(-2.8021873309261,-4.06949741411341,0.00374292245829196));
#50783=CARTESIAN_POINT('Origin',(-32.3478126690739,0.,0.));
#50784=CARTESIAN_POINT('',(-6.09781266907385,-4.06532783024481,0.00248275864732798));
#50785=CARTESIAN_POINT('',(-5.80218733092609,-4.06735085704707,-0.00339183732646908));
#50786=CARTESIAN_POINT('',(-32.3478126690739,-4.0705,-4.82875428449296E-13));
#50787=CARTESIAN_POINT('Ctrl Pts',(-6.09781266907385,-4.06532783024481,
0.00248275864732861));
#50788=CARTESIAN_POINT('Ctrl Pts',(-6.0484988304481,-4.06065183816668,-0.840802599870245));
#50789=CARTESIAN_POINT('Ctrl Pts',(-5.91963910344927,-3.39313702767653,
-3.05113638265515));
#50790=CARTESIAN_POINT('Ctrl Pts',(-5.71123348807733,0.233422028762872,
-4.80877700124299));
#50791=CARTESIAN_POINT('Ctrl Pts',(-5.47259582295814,4.171611218274,-2.40343127894775));
#50792=CARTESIAN_POINT('Ctrl Pts',(-5.23395815783889,4.27722630874114,2.21001293857749));
#50793=CARTESIAN_POINT('Ctrl Pts',(-4.99532049271968,0.453235799314355,
4.7930574212978));
#50794=CARTESIAN_POINT('Ctrl Pts',(-4.78327199646466,-3.31468772914499,
3.17542596303663));
#50795=CARTESIAN_POINT('Ctrl Pts',(-4.65076938858272,-4.06012588239192,
0.901675116191023));
#50796=CARTESIAN_POINT('Ctrl Pts',(-4.59781266907386,-4.0666555507277,-0.00316262964624277));
#50797=CARTESIAN_POINT('Ctrl Pts',(-5.80218733092609,-4.06735085704707,
-0.00339183732646849));
#50798=CARTESIAN_POINT('Ctrl Pts',(-5.77722620823787,-4.07069006794027,
-0.429702830878314));
#50799=CARTESIAN_POINT('Ctrl Pts',(-5.67271919717658,-3.81249861092392,
-2.21063503182293));
#50800=CARTESIAN_POINT('Ctrl Pts',(-5.48866629774222,-1.22616783934351,
-4.65567735364785));
#50801=CARTESIAN_POINT('Ctrl Pts',(-5.25002863262297,3.25370797337249,-3.54854948612432));
#50802=CARTESIAN_POINT('Ctrl Pts',(-5.01139096750376,4.74431268704714,0.818728472038551));
#50803=CARTESIAN_POINT('Ctrl Pts',(-4.77275330238453,1.87618665939981,4.43381811498155));
#50804=CARTESIAN_POINT('Ctrl Pts',(-4.53635209019197,-2.67261016863284,
3.97973264573628));
#50805=CARTESIAN_POINT('Ctrl Pts',(-4.3794967663725,-4.07394104096335,1.31152214803601));
#50806=CARTESIAN_POINT('Ctrl Pts',(-4.30218733092609,-4.0770951458019,-0.000710233193597031));
#50807=CARTESIAN_POINT('Origin',(-32.3478126690739,0.,0.));
#50808=CARTESIAN_POINT('',(-7.59781266907386,-4.07574630203772,0.00222153505732406));
#50809=CARTESIAN_POINT('',(-7.3021873309261,-4.06485256559003,0.00211562990566405));
#50810=CARTESIAN_POINT('',(-32.3478126690739,-4.0705,-4.82875428449296E-13));
#50811=CARTESIAN_POINT('Ctrl Pts',(-7.59781266907386,-4.07574630203772,
0.00222153505732401));
#50812=CARTESIAN_POINT('Ctrl Pts',(-7.52577416068655,-4.06771182434402,
-1.22161827070251));
#50813=CARTESIAN_POINT('Ctrl Pts',(-7.37418976392616,-2.82963048299844,
-3.81092663700425));
#50814=CARTESIAN_POINT('Ctrl Pts',(-7.14305947879272,1.57860706315775,-4.5482767971816));
#50815=CARTESIAN_POINT('Ctrl Pts',(-6.90442181367349,4.6797195025539,-1.13094980465497));
#50816=CARTESIAN_POINT('Ctrl Pts',(-6.66578414855425,3.48144476711953,3.32541191686152));
#50817=CARTESIAN_POINT('Ctrl Pts',(-6.42714648343504,-0.91532914635784,
4.72662613694493));
#50818=CARTESIAN_POINT('Ctrl Pts',(-6.23782265694156,-3.7363609545651,2.39316384250277));
#50819=CARTESIAN_POINT('Ctrl Pts',(-6.12804471882117,-4.06819446624524,
0.519462284483144));
#50820=CARTESIAN_POINT('Ctrl Pts',(-6.09781266907385,-4.06532783024481,
0.00248275864732861));
#50821=CARTESIAN_POINT('Ctrl Pts',(-7.3021873309261,-4.06485256559003,0.0021156299056644));
#50822=CARTESIAN_POINT('Ctrl Pts',(-7.25450153847633,-4.06102628102932,
-0.813568030876496));
#50823=CARTESIAN_POINT('Ctrl Pts',(-7.12726985765349,-3.42680090686785,
-2.99539080099765));
#50824=CARTESIAN_POINT('Ctrl Pts',(-6.92049228845756,0.134999037069343,
-4.81254552210429));
#50825=CARTESIAN_POINT('Ctrl Pts',(-6.68185462333835,4.1215704771241,-2.48826765871595));
#50826=CARTESIAN_POINT('Ctrl Pts',(-6.44321695821911,4.32154162229638,2.12205022265777));
#50827=CARTESIAN_POINT('Ctrl Pts',(-6.20457929309988,0.551193473920355,
4.78278213002022));
#50828=CARTESIAN_POINT('Ctrl Pts',(-5.99090275066888,-3.27821055126197,
3.23074519309206));
#50829=CARTESIAN_POINT('Ctrl Pts',(-5.85677209661095,-4.06004869975013,
0.928861330231892));
#50830=CARTESIAN_POINT('Ctrl Pts',(-5.80218733092609,-4.06735085704707,
-0.00339183732646849));
#50831=CARTESIAN_POINT('Origin',(-32.3478126690739,0.,0.));
#50832=CARTESIAN_POINT('',(-9.09781266907386,-4.07222943229488,-0.00357906261956567));
#50833=CARTESIAN_POINT('',(-8.8021873309261,-4.07511392925337,0.00260772300212458));
#50834=CARTESIAN_POINT('',(-32.3478126690739,-4.0705,-4.82875428449296E-13));
#50835=CARTESIAN_POINT('Ctrl Pts',(-9.09781266907386,-4.07222943229488,
-0.003579062619565));
#50836=CARTESIAN_POINT('Ctrl Pts',(-9.08259537929808,-4.07461348194488,
-0.262682434050171));
#50837=CARTESIAN_POINT('Ctrl Pts',(-8.98783220114923,-3.93387284883695,
-1.87362564859038));
#50838=CARTESIAN_POINT('Ctrl Pts',(-8.8135231346273,-1.78562688897607,-4.47105789459565));
#50839=CARTESIAN_POINT('Ctrl Pts',(-8.57488546950807,2.79593183551325,-3.91938608134342));
#50840=CARTESIAN_POINT('Ctrl Pts',(-8.33624780438884,4.80879098967182,0.233133655034067));
#50841=CARTESIAN_POINT('Ctrl Pts',(-8.09761013926962,2.40368143941586,4.17146708260569));
#50842=CARTESIAN_POINT('Ctrl Pts',(-7.85897247415039,-2.20975644067261,
4.27735882951057));
#50843=CARTESIAN_POINT('Ctrl Pts',(-7.69237331741847,-4.01320701615423,
1.60783980898199));
#50844=CARTESIAN_POINT('Ctrl Pts',(-7.60532004905963,-4.07658360250915,
0.129762077875785));
#50845=CARTESIAN_POINT('Ctrl Pts',(-7.59781266907386,-4.07574630203772,
0.00222153505732401));
#50846=CARTESIAN_POINT('Ctrl Pts',(-8.8021873309261,-4.07511392925337,0.00260772300212448));
#50847=CARTESIAN_POINT('Ctrl Pts',(-8.73177686871478,-4.06620451024253,
-1.1940613554039));
#50848=CARTESIAN_POINT('Ctrl Pts',(-8.58182051813039,-2.87606084879853,
-3.7580704643467));
#50849=CARTESIAN_POINT('Ctrl Pts',(-8.35231827917293,1.48523158453539,-4.57961857379977));
#50850=CARTESIAN_POINT('Ctrl Pts',(-8.1136806140537,4.65560380841346,-1.22644703115444));
#50851=CARTESIAN_POINT('Ctrl Pts',(-7.87504294893448,3.54874460969979,3.25349517231261));
#50852=CARTESIAN_POINT('Ctrl Pts',(-7.63640528381524,-0.818443985601727,
4.74436176780107));
#50853=CARTESIAN_POINT('Ctrl Pts',(-7.44545341114579,-3.71128559220026,
2.44953276936589));
#50854=CARTESIAN_POINT('Ctrl Pts',(-7.33404742684941,-4.06740900403576,
0.547094717816802));
#50855=CARTESIAN_POINT('Ctrl Pts',(-7.3021873309261,-4.06485256559003,0.0021156299056644));
#50856=CARTESIAN_POINT('Origin',(-32.3478126690739,0.,0.));
#50857=CARTESIAN_POINT('',(-10.5978126690739,-4.06383028861155,-0.000517316456022591));
#50858=CARTESIAN_POINT('',(-10.3021873309261,-4.07305647823417,-0.00339818811806003));
#50859=CARTESIAN_POINT('',(-32.3478126690739,-4.0705,-4.82875428449296E-13));
#50860=CARTESIAN_POINT('Ctrl Pts',(-10.5978126690739,-4.06383028861155,
-0.000517316456022585));
#50861=CARTESIAN_POINT('Ctrl Pts',(-10.5598707095365,-4.06456413075875,
-0.649936894253117));
#50862=CARTESIAN_POINT('Ctrl Pts',(-10.4423828616261,-3.6108734382595,-2.65990611006904));
#50863=CARTESIAN_POINT('Ctrl Pts',(-10.2453491253427,-0.453810659605433,
-4.79300302197796));
#50864=CARTESIAN_POINT('Ctrl Pts',(-10.0067114602234,3.78679836713871,-2.97304224828663));
#50865=CARTESIAN_POINT('Ctrl Pts',(-9.76807379510421,4.54837145493611,1.57833430913225));
#50866=CARTESIAN_POINT('Ctrl Pts',(-9.52943612998497,1.131230436189,4.67965167333008));
#50867=CARTESIAN_POINT('Ctrl Pts',(-9.30601575464153,-3.04102820872573,
3.55803793366217));
#50868=CARTESIAN_POINT('Ctrl Pts',(-9.16214126767116,-4.06215125311643,
1.09173797619339));
#50869=CARTESIAN_POINT('Ctrl Pts',(-9.09781266907386,-4.07222943229488,
-0.003579062619565));
#50870=CARTESIAN_POINT('Ctrl Pts',(-10.3021873309261,-4.07305647823417,
-0.00339818811806027));
#50871=CARTESIAN_POINT('Ctrl Pts',(-10.2885980873263,-4.07512744307457,
-0.234659625407061));
#50872=CARTESIAN_POINT('Ctrl Pts',(-10.1954629553534,-3.95181437733735,
-1.8174227959994));
#50873=CARTESIAN_POINT('Ctrl Pts',(-10.0227819350075,-1.8767184363934,-4.43359301827195));
#50874=CARTESIAN_POINT('Ctrl Pts',(-9.78414426988828,2.71516687463254,-3.97576256635973));
#50875=CARTESIAN_POINT('Ctrl Pts',(-9.54550660476906,4.8125536089566,0.134710437930172));
#50876=CARTESIAN_POINT('Ctrl Pts',(-9.30686893964983,2.48851481691486,4.12142125330121));
#50877=CARTESIAN_POINT('Ctrl Pts',(-9.06823127453061,-2.12179106496689,
4.32166886952238));
#50878=CARTESIAN_POINT('Ctrl Pts',(-8.9000040716227,-3.99762873478501,1.66388105000583));
#50879=CARTESIAN_POINT('Ctrl Pts',(-8.81132275708786,-4.07626988444755,
0.157869905105551));
#50880=CARTESIAN_POINT('Ctrl Pts',(-8.8021873309261,-4.07511392925337,0.00260772300212448));
#50881=CARTESIAN_POINT('Origin',(-32.3478126690739,0.,0.));
#50882=CARTESIAN_POINT('',(-12.0978126690739,-4.07032458744755,0.00376143334710477));
#50883=CARTESIAN_POINT('',(-11.8021873309261,-4.06398132384238,-0.00096959209926889));
#50884=CARTESIAN_POINT('',(-32.3478126690739,-4.0705,-4.82875428449296E-13));
#50885=CARTESIAN_POINT('Ctrl Pts',(-12.0978126690739,-4.07032458744755,
0.00376143334710491));
#50886=CARTESIAN_POINT('Ctrl Pts',(-12.037146039775,-4.06079261000553,-1.03044389103757));
#50887=CARTESIAN_POINT('Ctrl Pts',(-11.8969335221031,-3.13401642257978,
-3.43588983608773));
#50888=CARTESIAN_POINT('Ctrl Pts',(-11.677175116058,0.914762246840484,-4.7267358838015));
#50889=CARTESIAN_POINT('Ctrl Pts',(-11.4385374509388,4.47095080603802,-1.78589500627826));
#50890=CARTESIAN_POINT('Ctrl Pts',(-11.1998997858196,3.91955374080681,2.79569679264203));
#50891=CARTESIAN_POINT('Ctrl Pts',(-10.9612621207003,-0.232845280914501,
4.80880496159049));
#50892=CARTESIAN_POINT('Ctrl Pts',(-10.7605664151184,-3.54512857250201,
2.78629205291713));
#50893=CARTESIAN_POINT('Ctrl Pts',(-10.6394165979096,-4.06302561966876,
0.711581010269389));
#50894=CARTESIAN_POINT('Ctrl Pts',(-10.5978126690739,-4.06383028861155,
-0.000517316456022585));
#50895=CARTESIAN_POINT('Ctrl Pts',(-11.8021873309261,-4.06398132384238,
-0.000969592099269029));
#50896=CARTESIAN_POINT('Ctrl Pts',(-11.7658734175648,-4.06530044997824,
-0.622465582635642));
#50897=CARTESIAN_POINT('Ctrl Pts',(-11.6500136158304,-3.63881171341208,
-2.60363619702803));
#50898=CARTESIAN_POINT('Ctrl Pts',(-11.4546079257229,-0.551767098271795,
-4.78271598680431));
#50899=CARTESIAN_POINT('Ctrl Pts',(-11.2159702606036,3.72518553231084,-3.04988719316482));
#50900=CARTESIAN_POINT('Ctrl Pts',(-10.9773325954844,4.57970763196809,1.48495695118139));
#50901=CARTESIAN_POINT('Ctrl Pts',(-10.7386949303652,1.22672621632081,4.65553025243742));
#50902=CARTESIAN_POINT('Ctrl Pts',(-10.5136465088458,-2.99816785865763,
3.6119546083943));
#50903=CARTESIAN_POINT('Ctrl Pts',(-10.3681439756994,-4.06300485973803,
1.11905048660218));
#50904=CARTESIAN_POINT('Ctrl Pts',(-10.3021873309261,-4.07305647823417,
-0.00339818811806027));
#50905=CARTESIAN_POINT('Origin',(-32.3478126690739,0.,0.));
#50906=CARTESIAN_POINT('',(-13.5978126690739,-4.07681666553846,-0.0012043583654883));
#50907=CARTESIAN_POINT('',(-13.3021873309261,-4.06948780842451,0.00374258894561955));
#50908=CARTESIAN_POINT('',(-32.3478126690739,-4.0705,-4.82875428449296E-13));
#50909=CARTESIAN_POINT('Ctrl Pts',(-13.5978126690739,-4.07681666553846,
-0.00120435836548843));
#50910=CARTESIAN_POINT('Ctrl Pts',(-13.5939672583865,-4.07707083999085,
-0.0664874041950833));
#50911=CARTESIAN_POINT('Ctrl Pts',(-13.5105759593261,-4.04602154531668,
-1.48196385087443));
#50912=CARTESIAN_POINT('Ctrl Pts',(-13.3476387718926,-2.40418173141341,
-4.17117876454601));
#50913=CARTESIAN_POINT('Ctrl Pts',(-13.1090011067734,2.20924341525388,-4.27762382820403));
#50914=CARTESIAN_POINT('Ctrl Pts',(-12.8703634416541,4.79297579923065,-0.454098085715957));
#50915=CARTESIAN_POINT('Ctrl Pts',(-12.6317257765349,2.97326932976115,3.78662007285696));
#50916=CARTESIAN_POINT('Ctrl Pts',(-12.3930881114157,-1.57806154943975,
4.54846609634954));
#50917=CARTESIAN_POINT('Ctrl Pts',(-12.2151170755953,-3.89111272737449,
2.00017169269057));
#50918=CARTESIAN_POINT('Ctrl Pts',(-12.1166919281481,-4.07329090803759,
0.325602789635245));
#50919=CARTESIAN_POINT('Ctrl Pts',(-12.0978126690739,-4.07032458744755,
0.00376143334710491));
#50920=CARTESIAN_POINT('Ctrl Pts',(-13.3021873309261,-4.06948780842451,
0.00374258894561951));
#50921=CARTESIAN_POINT('Ctrl Pts',(-13.2431487478032,-4.06042005381897,
-1.00323625051947));
#50922=CARTESIAN_POINT('Ctrl Pts',(-13.1045642763073,-3.17385622399582,
-3.38123201716333));
#50923=CARTESIAN_POINT('Ctrl Pts',(-12.8864339164382,0.817874959696777,
-4.74445989460021));
#50924=CARTESIAN_POINT('Ctrl Pts',(-12.647796251319,4.43348046720131,-1.87698430683722));
#50925=CARTESIAN_POINT('Ctrl Pts',(-12.4091585861998,3.9759253824068,2.71492845112022));
#50926=CARTESIAN_POINT('Ctrl Pts',(-12.1705209210805,-0.134421838351238,
4.81256167862222));
#50927=CARTESIAN_POINT('Ctrl Pts',(-11.9681971693227,-3.51458600877433,
2.84237865671728));
#50928=CARTESIAN_POINT('Ctrl Pts',(-11.8454193059378,-4.06241089469102,
0.738925854183665));
#50929=CARTESIAN_POINT('Ctrl Pts',(-11.8021873309261,-4.06398132384238,
-0.000969592099269029));
#50930=CARTESIAN_POINT('Origin',(-32.3478126690739,0.,0.));
#50931=CARTESIAN_POINT('',(-15.0978126690739,-4.06666337103388,-0.00316560979000432));
#50932=CARTESIAN_POINT('',(-14.8021873309261,-4.07709762639944,-0.00070430106655972));
#50933=CARTESIAN_POINT('',(-32.3478126690739,-4.0705,-4.82875428449296E-13));
#50934=CARTESIAN_POINT('Ctrl Pts',(-15.0978126690739,-4.06666337103388,
-0.00316560979000423));
#50935=CARTESIAN_POINT('Ctrl Pts',(-15.071242588625,-4.06994301140227,-0.457149458338325));
#50936=CARTESIAN_POINT('Ctrl Pts',(-14.965126619803,-3.79006310537379,-2.26634942371038));
#50937=CARTESIAN_POINT('Ctrl Pts',(-14.7794647626079,-1.13179168699179,
-4.67951596436188));
#50938=CARTESIAN_POINT('Ctrl Pts',(-14.5408270974888,3.32478553700414,-3.48204296590229));
#50939=CARTESIAN_POINT('Ctrl Pts',(-14.3021894323695,4.72679073178803,0.914478792178541));
#50940=CARTESIAN_POINT('Ctrl Pts',(-14.0635517672503,1.78616311715816,4.47084370140194));
#50941=CARTESIAN_POINT('Ctrl Pts',(-13.8287595128184,-2.72163337242562,
3.9286021789031));
#50942=CARTESIAN_POINT('Ctrl Pts',(-13.6735131467596,-4.07181300558473,
1.28395297745419));
#50943=CARTESIAN_POINT('Ctrl Pts',(-13.5978126690739,-4.07681666553846,
-0.00120435836548843));
#50944=CARTESIAN_POINT('Ctrl Pts',(-14.8021873309261,-4.07709762639944,
-0.000704301066560046));
#50945=CARTESIAN_POINT('Ctrl Pts',(-14.7999699664147,-4.07718738154795,
-0.0383412680213716));
#50946=CARTESIAN_POINT('Ctrl Pts',(-14.7182067135303,-4.05963949617112,
-1.42608358607219));
#50947=CARTESIAN_POINT('Ctrl Pts',(-14.5568975722728,-2.48900910600372,
-4.12112276102026));
#50948=CARTESIAN_POINT('Ctrl Pts',(-14.3182599071536,2.12127272581082,-4.32192331767929));
#50949=CARTESIAN_POINT('Ctrl Pts',(-14.0796222420344,4.78268288982128,-0.552053907312987));
#50950=CARTESIAN_POINT('Ctrl Pts',(-13.8409845769151,3.05011057970114,3.72500262990027));
#50951=CARTESIAN_POINT('Ctrl Pts',(-13.6023469117959,-1.48468231248816,
4.57979667366944));
#50952=CARTESIAN_POINT('Ctrl Pts',(-13.4227478297996,-3.8710120869076,2.05648068706029));
#50953=CARTESIAN_POINT('Ctrl Pts',(-13.3226946361763,-4.0726375319069,0.353521010938116));
#50954=CARTESIAN_POINT('Ctrl Pts',(-13.3021873309261,-4.06948780842451,
0.00374258894561951));
#50955=CARTESIAN_POINT('Origin',(-32.3478126690739,0.,0.));
#50956=CARTESIAN_POINT('',(-16.5978126690739,-4.06532180994014,0.00247865735123198));
#50957=CARTESIAN_POINT('',(-16.3021873309261,-4.06735933458706,-0.00339422375240483));
#50958=CARTESIAN_POINT('',(-32.3478126690739,-4.0705,-4.82875428449296E-13));
#50959=CARTESIAN_POINT('Ctrl Pts',(-16.5978126690739,-4.06532180994014,
0.00247865735123177));
#50960=CARTESIAN_POINT('Ctrl Pts',(-16.5485179188634,-4.06065576655941,
-0.840483409511789));
#50961=CARTESIAN_POINT('Ctrl Pts',(-16.4196772802799,-3.39353668499773,
-3.05048344280494));
#50962=CARTESIAN_POINT('Ctrl Pts',(-16.2112907533233,0.232268530165553,
-4.80883285354733));
#50963=CARTESIAN_POINT('Ctrl Pts',(-15.9726530882041,4.17103458301497,-2.40443186444421));
#50964=CARTESIAN_POINT('Ctrl Pts',(-15.7340154230849,4.27775630447756,2.20898689062749));
#50965=CARTESIAN_POINT('Ctrl Pts',(-15.4953777579657,0.454385510193501,
4.79294855924697));
#50966=CARTESIAN_POINT('Ctrl Pts',(-15.2833101732953,-3.31426516276753,
3.17607544524493));
#50967=CARTESIAN_POINT('Ctrl Pts',(-15.1507884769981,-4.06012437697437,
0.9019939062919));
#50968=CARTESIAN_POINT('Ctrl Pts',(-15.0978126690739,-4.06666337103388,
-0.00316560979000423));
#50969=CARTESIAN_POINT('Ctrl Pts',(-16.3021873309261,-4.06735933458706,
-0.0033942237524047));
#50970=CARTESIAN_POINT('Ctrl Pts',(-16.2772452966532,-4.07069882146085,
-0.42937696578519));
#50971=CARTESIAN_POINT('Ctrl Pts',(-16.1727573740072,-3.81276059892577,
-2.20997410073169));
#50972=CARTESIAN_POINT('Ctrl Pts',(-15.9887235629882,-1.22728457340874,
-4.65538309025602));
#50973=CARTESIAN_POINT('Ctrl Pts',(-15.7500858978689,3.25285668605437,-3.54932986930775));
#50974=CARTESIAN_POINT('Ctrl Pts',(-15.5114482327497,4.74450893241555,0.817590442335157));
#50975=CARTESIAN_POINT('Ctrl Pts',(-15.2728105676305,1.8772501705311,4.43336790018713));
#50976=CARTESIAN_POINT('Ctrl Pts',(-15.0363902670226,-2.67202280013241,
3.98033711867999));
#50977=CARTESIAN_POINT('Ctrl Pts',(-14.8795158547878,-4.07396749912098,
1.31184989664949));
#50978=CARTESIAN_POINT('Ctrl Pts',(-14.8021873309261,-4.07709762639944,
-0.000704301066560046));
#50979=CARTESIAN_POINT('Origin',(-32.3478126690739,0.,0.));
#50980=CARTESIAN_POINT('',(-18.0978126690739,-4.0757393762113,0.00222632843356818));
#50981=CARTESIAN_POINT('',(-17.8021873309261,-4.06484746876737,0.00211112861108809));
#50982=CARTESIAN_POINT('',(-32.3478126690739,-4.0705,-4.82875428449296E-13));
#50983=CARTESIAN_POINT('Ctrl Pts',(-18.0978126690739,-4.0757393762113,0.00222632843356826));
#50984=CARTESIAN_POINT('Ctrl Pts',(-18.0257932491019,-4.06769305643308,
-1.22129466881777));
#50985=CARTESIAN_POINT('Ctrl Pts',(-17.8742279407568,-2.83018048694797,
-3.8103087610216));
#50986=CARTESIAN_POINT('Ctrl Pts',(-17.6431167440387,1.5775160130308,-4.54865533010503));
#50987=CARTESIAN_POINT('Ctrl Pts',(-17.4044790789195,4.6794480846352,-1.13207230628853));
#50988=CARTESIAN_POINT('Ctrl Pts',(-17.1658414138002,3.48224234046452,3.3245767197852));
#50989=CARTESIAN_POINT('Ctrl Pts',(-16.927203748681,-0.914195334228,4.72684556277623));
#50990=CARTESIAN_POINT('Ctrl Pts',(-16.7378608337722,-3.73607127850369,
2.39382482140684));
#50991=CARTESIAN_POINT('Ctrl Pts',(-16.6280638072365,-4.06818526137017,
0.519786521610059));
#50992=CARTESIAN_POINT('Ctrl Pts',(-16.5978126690739,-4.06532180994014,
0.00247865735123177));
#50993=CARTESIAN_POINT('Ctrl Pts',(-17.8021873309261,-4.06484746876737,
0.00211112861108823));
#50994=CARTESIAN_POINT('Ctrl Pts',(-17.7545206268917,-4.0610311343114,-0.813248574751964));
#50995=CARTESIAN_POINT('Ctrl Pts',(-17.6273080344841,-3.42719055604098,
-2.99473654818825));
#50996=CARTESIAN_POINT('Ctrl Pts',(-17.4205495537035,0.133844637744424,
-4.81257776603306));
#50997=CARTESIAN_POINT('Ctrl Pts',(-17.1819118885843,4.1209734926491,-2.4892562371223));
#50998=CARTESIAN_POINT('Ctrl Pts',(-16.9432742234651,4.32205051844462,2.12101354478971));
#50999=CARTESIAN_POINT('Ctrl Pts',(-16.7046365583459,0.55234071436891,4.78264977563894));
#51000=CARTESIAN_POINT('Ctrl Pts',(-16.4909409274995,-3.27777761810244,
3.23139288635401));
#51001=CARTESIAN_POINT('Ctrl Pts',(-16.3567911850263,-4.06004842914805,
0.929180049887315));
#51002=CARTESIAN_POINT('Ctrl Pts',(-16.3021873309261,-4.06735933458706,
-0.0033942237524047));
#51003=CARTESIAN_POINT('Origin',(-32.3478126690739,0.,0.));
#51004=CARTESIAN_POINT('',(-19.5978126690739,-4.07223926118534,-0.00357729417079465));
#51005=CARTESIAN_POINT('',(-19.3021873309261,-4.07510605262456,0.00261196768466351));
#51006=CARTESIAN_POINT('',(-32.3478126690739,-4.0705,-4.82875428449296E-13));
#51007=CARTESIAN_POINT('Ctrl Pts',(-19.5978126690739,-4.07223926118534,
-0.00357729417079473));
#51008=CARTESIAN_POINT('Ctrl Pts',(-19.5826144677134,-4.07461978933759,
-0.262354039634738));
#51009=CARTESIAN_POINT('Ctrl Pts',(-19.4878703779799,-3.9340869821028,-1.87296646703573));
#51010=CARTESIAN_POINT('Ctrl Pts',(-19.3135803998733,-1.78669931964703,
-4.4706294438965));
#51011=CARTESIAN_POINT('Ctrl Pts',(-19.074942734754,2.79499160370957,-3.92005663462335));
#51012=CARTESIAN_POINT('Ctrl Pts',(-18.8363050696348,4.80884677358576,0.231980153537627));
#51013=CARTESIAN_POINT('Ctrl Pts',(-18.5976674045156,2.4046819888283,4.1708903864842));
#51014=CARTESIAN_POINT('Ctrl Pts',(-18.3590297393964,-2.20873035805718,
4.27788876536757));
#51015=CARTESIAN_POINT('Ctrl Pts',(-18.1924114942491,-4.01302793193152,
1.60849660347309));
#51016=CARTESIAN_POINT('Ctrl Pts',(-18.1053391374749,-4.07658026567666,
0.130091730952273));
#51017=CARTESIAN_POINT('Ctrl Pts',(-18.0978126690739,-4.0757393762113,0.00222632843356826));
#51018=CARTESIAN_POINT('Ctrl Pts',(-19.3021873309261,-4.07510605262456,
0.00261196768466343));
#51019=CARTESIAN_POINT('Ctrl Pts',(-19.2317959571301,-4.06618795069759,
-1.19373875342118));
#51020=CARTESIAN_POINT('Ctrl Pts',(-19.081858694961,-2.87659949644564,-3.75744888720017));
#51021=CARTESIAN_POINT('Ctrl Pts',(-18.8523755444189,1.48413301908516,-4.57997470766269));
#51022=CARTESIAN_POINT('Ctrl Pts',(-18.6137378792997,4.6553094840529,-1.22756374533297));
#51023=CARTESIAN_POINT('Ctrl Pts',(-18.3751002141804,3.54952493031783,3.25264383390203));
#51024=CARTESIAN_POINT('Ctrl Pts',(-18.1364625490612,-0.817305922033317,
4.74455795316888));
#51025=CARTESIAN_POINT('Ctrl Pts',(-17.9454915879764,-3.71098714745764,
2.45019360063996));
#51026=CARTESIAN_POINT('Ctrl Pts',(-17.8340665152647,-4.06739980864662,
0.547418441384662));
#51027=CARTESIAN_POINT('Ctrl Pts',(-17.8021873309261,-4.06484746876737,
0.00211112861108823));
#51028=CARTESIAN_POINT('Origin',(-32.3478126690739,0.,0.));
#51029=CARTESIAN_POINT('',(-21.0978126690739,-4.06383152666866,-0.000522675918812766));
#51030=CARTESIAN_POINT('',(-20.8021873309261,-4.07306601825716,-0.00339571005182004));
#51031=CARTESIAN_POINT('',(-32.3478126690739,-4.0705,-4.82875428449296E-13));
#51032=CARTESIAN_POINT('Ctrl Pts',(-21.0978126690739,-4.06383152666866,
-0.00052267591881365));
#51033=CARTESIAN_POINT('Ctrl Pts',(-21.0598897979519,-4.06457261097563,
-0.649615040927229));
#51034=CARTESIAN_POINT('Ctrl Pts',(-20.9424210384568,-3.6112055683889,-2.65924661123667));
#51035=CARTESIAN_POINT('Ctrl Pts',(-20.7454063905886,-0.454960354245989,
-4.79289402757069));
#51036=CARTESIAN_POINT('Ctrl Pts',(-20.5067687254694,3.78608510831067,-2.97395051002756));
#51037=CARTESIAN_POINT('Ctrl Pts',(-20.2681310603502,4.54874992244621,1.57724323631644));
#51038=CARTESIAN_POINT('Ctrl Pts',(-20.0294933952309,1.13235292151423,4.67938018808041));
#51039=CARTESIAN_POINT('Ctrl Pts',(-19.8060539314722,-3.04053113635729,
3.55867154707108));
#51040=CARTESIAN_POINT('Ctrl Pts',(-19.6621603560865,-4.06216033955295,
1.09205794767961));
#51041=CARTESIAN_POINT('Ctrl Pts',(-19.5978126690739,-4.07223926118534,
-0.00357729417079473));
#51042=CARTESIAN_POINT('Ctrl Pts',(-20.8021873309261,-4.07306601825716,
-0.0033957100518197));
#51043=CARTESIAN_POINT('Ctrl Pts',(-20.7886171757417,-4.07513318091976,
-0.234330901384573));
#51044=CARTESIAN_POINT('Ctrl Pts',(-20.6955011321841,-3.95202089787016,
-1.81676406404286));
#51045=CARTESIAN_POINT('Ctrl Pts',(-20.5228392002535,-1.87778187766528,
-4.43314271832978));
#51046=CARTESIAN_POINT('Ctrl Pts',(-20.2842015351343,2.71421312200688,-3.97641374475733));
#51047=CARTESIAN_POINT('Ctrl Pts',(-20.045563870015,4.81258578377826,0.133556036718511));
#51048=CARTESIAN_POINT('Ctrl Pts',(-19.8069262048958,2.48950335928912,4.12082420945821));
#51049=CARTESIAN_POINT('Ctrl Pts',(-19.5682885397766,-2.12075435614108,
4.32217770366716));
#51050=CARTESIAN_POINT('Ctrl Pts',(-19.4000422484533,-3.99744242114115,
1.66453839875525));
#51051=CARTESIAN_POINT('Ctrl Pts',(-19.3113418455032,-4.07626586652913,
0.158199357517422));
#51052=CARTESIAN_POINT('Ctrl Pts',(-19.3021873309261,-4.07510605262456,
0.00261196768466343));
#51053=CARTESIAN_POINT('Origin',(-32.3478126690739,0.,0.));
#51054=CARTESIAN_POINT('',(-22.5978126690739,-4.07031468847398,0.00376156571352546));
#51055=CARTESIAN_POINT('',(-22.3021873309261,-4.06398364289261,-0.000974823831897398));
#51056=CARTESIAN_POINT('',(-32.3478126690739,-4.0705,-4.82875428449296E-13));
#51057=CARTESIAN_POINT('Ctrl Pts',(-22.5978126690739,-4.07031468847398,
0.00376156571352537));
#51058=CARTESIAN_POINT('Ctrl Pts',(-22.5371651281903,-4.06078745327604,
-1.03012477253975));
#51059=CARTESIAN_POINT('Ctrl Pts',(-22.3969716989337,-3.13448885277667,
-3.4352501825917));
#51060=CARTESIAN_POINT('Ctrl Pts',(-22.177232381304,0.913628408435968,-4.7269551737383));
#51061=CARTESIAN_POINT('Ctrl Pts',(-21.9385947161847,4.47052229104313,-1.7869674112637));
#51062=CARTESIAN_POINT('Ctrl Pts',(-21.6999570510656,3.92022423769407,2.79475652063351));
#51063=CARTESIAN_POINT('Ctrl Pts',(-21.4613193859463,-0.231691776071347,
4.80886067632815));
#51064=CARTESIAN_POINT('Ctrl Pts',(-21.2606045919491,-3.54477519825892,
2.78695006207459));
#51065=CARTESIAN_POINT('Ctrl Pts',(-21.1394356863249,-4.06301813453931,
0.71190182958246));
#51066=CARTESIAN_POINT('Ctrl Pts',(-21.0978126690739,-4.06383152666866,
-0.00052267591881365));
#51067=CARTESIAN_POINT('Ctrl Pts',(-22.3021873309261,-4.06398364289261,
-0.000974823831896773));
#51068=CARTESIAN_POINT('Ctrl Pts',(-22.2658925059801,-4.06530923181794,
-0.622143240829621));
#51069=CARTESIAN_POINT('Ctrl Pts',(-22.150051792661,-3.63913463819147,-2.60297621081044));
#51070=CARTESIAN_POINT('Ctrl Pts',(-21.9546651909688,-0.552914322524486,
-4.78258349567352));
#51071=CARTESIAN_POINT('Ctrl Pts',(-21.7160275258496,3.72445384229878,-3.05078067349642));
#51072=CARTESIAN_POINT('Ctrl Pts',(-21.4773898607304,4.58006369995296,1.4838583643783));
#51073=CARTESIAN_POINT('Ctrl Pts',(-21.2387521956112,1.22784291284316,4.65523586110807));
#51074=CARTESIAN_POINT('Ctrl Pts',(-21.0136846856764,-2.99765973840581,
3.61258525206308));
#51075=CARTESIAN_POINT('Ctrl Pts',(-20.8681630641147,-4.06301583309485,
1.11937100559103));
#51076=CARTESIAN_POINT('Ctrl Pts',(-20.8021873309261,-4.07306601825716,
-0.0033957100518197));
#51077=CARTESIAN_POINT('Origin',(-32.3478126690739,0.,0.));
#51078=CARTESIAN_POINT('',(-24.0978126690739,-4.07682073202661,-0.00119862600692145));
#51079=CARTESIAN_POINT('',(-23.8021873309261,-4.06947811712022,0.00374200930701507));
#51080=CARTESIAN_POINT('',(-32.3478126690739,-4.0705,-4.82875428449296E-13));
#51081=CARTESIAN_POINT('Ctrl Pts',(-24.0978126690739,-4.07682073202661,
-0.0011986260069221));
#51082=CARTESIAN_POINT('Ctrl Pts',(-24.0939863468019,-4.07707257100012,
-0.0661574373907974));
#51083=CARTESIAN_POINT('Ctrl Pts',(-24.0106141361567,-4.04618464425921,
-1.48130837178561));
#51084=CARTESIAN_POINT('Ctrl Pts',(-23.8476960371386,-2.40518220884904,
-4.17060195021093));
#51085=CARTESIAN_POINT('Ctrl Pts',(-23.6090583720194,2.20821726762825,-4.27815364006511));
#51086=CARTESIAN_POINT('Ctrl Pts',(-23.3704207069001,4.7928667366398,-0.455247774302161));
#51087=CARTESIAN_POINT('Ctrl Pts',(-23.1317830417809,2.97417754833123,3.7859067598156));
#51088=CARTESIAN_POINT('Ctrl Pts',(-22.8931453766616,-1.57697045372341,
4.54884449829819));
#51089=CARTESIAN_POINT('Ctrl Pts',(-22.715155252426,-3.89088098364765,2.00083174485514));
#51090=CARTESIAN_POINT('Ctrl Pts',(-22.6167110165634,-4.07328346509314,
0.325930329695141));
#51091=CARTESIAN_POINT('Ctrl Pts',(-22.5978126690739,-4.07031468847398,
0.00376156571352537));
#51092=CARTESIAN_POINT('Ctrl Pts',(-23.8021873309261,-4.06947811712022,
0.00374200930701521));
#51093=CARTESIAN_POINT('Ctrl Pts',(-23.7431678362185,-4.06041648348459,
-1.00291735298318));
#51094=CARTESIAN_POINT('Ctrl Pts',(-23.6046024531379,-3.17431791098803,
-3.38058997938746));
#51095=CARTESIAN_POINT('Ctrl Pts',(-23.3864911816842,0.816736872430108,
-4.74465594332464));
#51096=CARTESIAN_POINT('Ctrl Pts',(-23.1478535165649,4.43303010358293,-1.87804772118901));
#51097=CARTESIAN_POINT('Ctrl Pts',(-22.9092158514458,3.97657650355884,2.71397465949093));
#51098=CARTESIAN_POINT('Ctrl Pts',(-22.6705781863265,-0.13326743518637,
4.81259378419344));
#51099=CARTESIAN_POINT('Ctrl Pts',(-22.4682353461533,-3.5142230495247,2.84303582389633));
#51100=CARTESIAN_POINT('Ctrl Pts',(-22.3454383943532,-4.06240399260436,
0.739246258441231));
#51101=CARTESIAN_POINT('Ctrl Pts',(-22.3021873309261,-4.06398364289261,
-0.000974823831896773));
#51102=CARTESIAN_POINT('Origin',(-32.3478126690739,0.,0.));
#51103=CARTESIAN_POINT('',(-25.5978126690739,-4.06667116509479,-0.00316860155561062));
#51104=CARTESIAN_POINT('',(-25.3021873309261,-4.07710011149971,-0.000698316132069499));
#51105=CARTESIAN_POINT('',(-32.3478126690739,-4.0705,-4.82875428449296E-13));
#51106=CARTESIAN_POINT('Ctrl Pts',(-25.5978126690739,-4.06667116509479,
-0.00316860155561056));
#51107=CARTESIAN_POINT('Ctrl Pts',(-25.5712616770403,-4.06995198256812,
-0.456824073053871));
#51108=CARTESIAN_POINT('Ctrl Pts',(-25.4651647966337,-3.79033356389561,
-2.26568828448685));
#51109=CARTESIAN_POINT('Ctrl Pts',(-25.2795220278539,-1.132913999441,-4.67924443383647));
#51110=CARTESIAN_POINT('Ctrl Pts',(-25.0408843627347,3.32395012330801,-3.48284034246832));
#51111=CARTESIAN_POINT('Ctrl Pts',(-24.8022466976155,4.72700999182265,0.913344916409211));
#51112=CARTESIAN_POINT('Ctrl Pts',(-24.5636090324962,1.78723547660136,4.47041513471273));
#51113=CARTESIAN_POINT('Ctrl Pts',(-24.3287976896491,-2.72105741290232,
3.9292109076427));
#51114=CARTESIAN_POINT('Ctrl Pts',(-24.1735322351749,-4.07183705933901,
1.28427935068815));
#51115=CARTESIAN_POINT('Ctrl Pts',(-24.0978126690739,-4.07682073202661,
-0.0011986260069221));
#51116=CARTESIAN_POINT('Ctrl Pts',(-25.3021873309261,-4.07710011149971,
-0.000698316132069399));
#51117=CARTESIAN_POINT('Ctrl Pts',(-25.2999890548301,-4.0771883891112,-0.0380112202494885));
#51118=CARTESIAN_POINT('Ctrl Pts',(-25.2182448903609,-4.05979569108433,
-1.42542869581234));
#51119=CARTESIAN_POINT('Ctrl Pts',(-25.0569548375188,-2.48999755919744,
-4.12052561435965));
#51120=CARTESIAN_POINT('Ctrl Pts',(-24.8183171723996,2.12023594681246,-4.32243201928095));
#51121=CARTESIAN_POINT('Ctrl Pts',(-24.5796795072803,4.78255033466597,-0.553201127887688));
#51122=CARTESIAN_POINT('Ctrl Pts',(-24.3410418421611,3.05100401366679,3.72427088853368));
#51123=CARTESIAN_POINT('Ctrl Pts',(-24.1024041770419,-1.48358370303888,
4.58015267461461));
#51124=CARTESIAN_POINT('Ctrl Pts',(-23.9227860066302,-3.87077237514414,
2.05714104990295));
#51125=CARTESIAN_POINT('Ctrl Pts',(-23.8227137245916,-4.07262966323526,
0.353848130340812));
#51126=CARTESIAN_POINT('Ctrl Pts',(-23.8021873309261,-4.06947811712022,
0.00374200930701521));
#51127=CARTESIAN_POINT('Origin',(-32.3478126690739,0.,0.));
#51128=CARTESIAN_POINT('',(-27.0978126690739,-4.06530890290629,0.00247015883041497));
#51129=CARTESIAN_POINT('',(-26.8021873309261,-4.0673676331488,-0.00339676908166275));
#51130=CARTESIAN_POINT('',(-32.3478126690739,-4.0705,-4.82875428449296E-13));
#51131=CARTESIAN_POINT('Ctrl Pts',(-27.0978126690739,-4.06530890290629,
0.0024701588304149));
#51132=CARTESIAN_POINT('Ctrl Pts',(-27.0485370072788,-4.06065548839014,
-0.840166902292313));
#51133=CARTESIAN_POINT('Ctrl Pts',(-26.9197154571106,-3.39394710335117,
-3.04982355875152));
#51134=CARTESIAN_POINT('Ctrl Pts',(-26.7113480185693,0.231122040344854,
-4.80889290141546));
#51135=CARTESIAN_POINT('Ctrl Pts',(-26.4727103534501,4.17045404914302,-2.40542998080026));
#51136=CARTESIAN_POINT('Ctrl Pts',(-26.2340726883308,4.27828796113812,2.20795949931288));
#51137=CARTESIAN_POINT('Ctrl Pts',(-25.9954350232116,0.45553419918425,4.79284005902739));
#51138=CARTESIAN_POINT('Ctrl Pts',(-25.7833483501259,-3.31384212136007,
3.1767246763176));
#51139=CARTESIAN_POINT('Ctrl Pts',(-25.6508075654134,-4.06012276262123,
0.902312619466092));
#51140=CARTESIAN_POINT('Ctrl Pts',(-25.5978126690739,-4.06667116509479,
-0.00316860155561056));
#51141=CARTESIAN_POINT('Ctrl Pts',(-26.8021873309261,-4.0673676331488,-0.00339676908166248));
#51142=CARTESIAN_POINT('Ctrl Pts',(-26.7772643850685,-4.07070764203952,
-0.429051031665485));
#51143=CARTESIAN_POINT('Ctrl Pts',(-26.6727955508379,-3.81302358814286,
-2.20931218578228));
#51144=CARTESIAN_POINT('Ctrl Pts',(-26.4887808282342,-1.22840035655279,
-4.65508935177024));
#51145=CARTESIAN_POINT('Ctrl Pts',(-26.2501431631149,3.25200474977257,-3.55010962682765));
#51146=CARTESIAN_POINT('Ctrl Pts',(-26.0115054979957,4.74470515142096,0.816452129912828));
#51147=CARTESIAN_POINT('Ctrl Pts',(-25.7728678328764,1.87831343359306,4.43291758398628));
#51148=CARTESIAN_POINT('Ctrl Pts',(-25.5364284438533,-2.67143520246076,
3.98094140217226));
#51149=CARTESIAN_POINT('Ctrl Pts',(-25.3795349432031,-4.07399401282602,
1.31217773515604));
#51150=CARTESIAN_POINT('Ctrl Pts',(-25.3021873309261,-4.07710011149971,
-0.000698316132069399));
#51151=CARTESIAN_POINT('Origin',(-32.3478126690739,0.,0.));
#51152=CARTESIAN_POINT('',(-28.5978126690739,-4.07533558288693,0.00197868943318482));
#51153=CARTESIAN_POINT('',(-28.3021873309261,-4.06480101368718,0.00206955444756823));
#51154=CARTESIAN_POINT('',(-32.3478126690739,-4.0705,-4.82875428449296E-13));
#51155=CARTESIAN_POINT('Ctrl Pts',(-28.5978126690739,-4.07533558288693,
0.00197868943318465));
#51156=CARTESIAN_POINT('Ctrl Pts',(-28.5258123375172,-4.0671548117311,-1.22130223361166));
#51157=CARTESIAN_POINT('Ctrl Pts',(-28.3742661175874,-2.83137270070474,
-3.80928172890928));
#51158=CARTESIAN_POINT('Ctrl Pts',(-28.1431740092847,1.57677629758835,-4.54925739906848));
#51159=CARTESIAN_POINT('Ctrl Pts',(-27.9045363441654,4.67899334175034,-1.13307817052668));
#51160=CARTESIAN_POINT('Ctrl Pts',(-27.6658986790463,3.48313507021902,3.32368060727122));
#51161=CARTESIAN_POINT('Ctrl Pts',(-27.4272610139269,-0.913111142894123,
4.72709634916456));
#51162=CARTESIAN_POINT('Ctrl Pts',(-27.2378990106029,-3.7357712242627,2.39447925508501));
#51163=CARTESIAN_POINT('Ctrl Pts',(-27.1280828956518,-4.06816751315389,
0.520105312452931));
#51164=CARTESIAN_POINT('Ctrl Pts',(-27.0978126690739,-4.06530890290629,
0.0024701588304149));
#51165=CARTESIAN_POINT('Ctrl Pts',(-28.3021873309261,-4.06480101368718,
0.00206955444756761));
#51166=CARTESIAN_POINT('Ctrl Pts',(-28.254539715307,-4.06101200920254,-0.812950610202758));
#51167=CARTESIAN_POINT('Ctrl Pts',(-28.1273462113148,-3.42764719991074,
-2.99402214660032));
#51168=CARTESIAN_POINT('Ctrl Pts',(-27.9206068189495,0.132734120902733,
-4.81264906024345));
#51169=CARTESIAN_POINT('Ctrl Pts',(-27.6819691538303,4.12035340306242,-2.4902241816421));
#51170=CARTESIAN_POINT('Ctrl Pts',(-27.4433314887111,4.32257108085691,2.11996606838733));
#51171=CARTESIAN_POINT('Ctrl Pts',(-27.2046938235918,0.55348171480276,4.78252270942354));
#51172=CARTESIAN_POINT('Ctrl Pts',(-26.9909791043302,-3.27734231397027,
3.2320385418624));
#51173=CARTESIAN_POINT('Ctrl Pts',(-26.8568102734416,-4.06004742651346,
0.929498100146529));
#51174=CARTESIAN_POINT('Ctrl Pts',(-26.8021873309261,-4.0673676331488,-0.00339676908166248));
#51175=CARTESIAN_POINT('Ctrl Pts',(-30.0683458050225,-1.79217368492187,
3.65473442716069));
#51176=CARTESIAN_POINT('Ctrl Pts',(-30.028572860836,-2.40105433738203,3.3561573610714));
#51177=CARTESIAN_POINT('Ctrl Pts',(-29.9490269724629,-3.45744192369399,
2.44891896771775));
#51178=CARTESIAN_POINT('Ctrl Pts',(-29.7899351957168,-4.48692818459232,
-0.165939112378094));
#51179=CARTESIAN_POINT('Ctrl Pts',(-29.5910704747841,-3.05580029857719,
-3.71995065683383));
#51180=CARTESIAN_POINT('Ctrl Pts',(-29.3524328096649,1.48524338711596,-4.58231611323432));
#51181=CARTESIAN_POINT('Ctrl Pts',(-29.1137951445456,4.65387018191312,-1.22765401651987));
#51182=CARTESIAN_POINT('Ctrl Pts',(-28.8751574794264,3.55090078994383,3.25125842872222));
#51183=CARTESIAN_POINT('Ctrl Pts',(-28.6365198143072,-0.816478135197904,
4.74503193420896));
#51184=CARTESIAN_POINT('Ctrl Pts',(-28.3978821491879,-4.4326431471991,1.8784345171529));
#51185=CARTESIAN_POINT('Ctrl Pts',(-28.1592444840687,-3.97698621643786,
-2.71342222480818));
#51186=CARTESIAN_POINT('Ctrl Pts',(-27.9206068189495,0.132734120902733,
-4.81264906024345));
#51187=CARTESIAN_POINT('Ctrl Pts',(-27.6819691538303,4.12035340306242,-2.4902241816421));
#51188=CARTESIAN_POINT('Ctrl Pts',(-27.4433314887111,4.32257108085691,2.11996606838733));
#51189=CARTESIAN_POINT('Ctrl Pts',(-27.2046938235918,0.55348171480276,4.78252270942354));
#51190=CARTESIAN_POINT('Ctrl Pts',(-26.9660561584726,-3.72408468243647,
3.05122444962453));
#51191=CARTESIAN_POINT('Ctrl Pts',(-26.7274184933533,-4.58024332037796,
-1.48330752890949));
#51192=CARTESIAN_POINT('Ctrl Pts',(-26.4887808282342,-1.22840035655279,
-4.65508935177024));
#51193=CARTESIAN_POINT('Ctrl Pts',(-26.2501431631149,3.25200474977257,-3.55010962682765));
#51194=CARTESIAN_POINT('Ctrl Pts',(-26.0115054979957,4.74470515142096,0.816452129912828));
#51195=CARTESIAN_POINT('Ctrl Pts',(-25.7728678328764,1.87831343359306,4.43291758398628));
#51196=CARTESIAN_POINT('Ctrl Pts',(-25.5342301677573,-2.71373612241715,
3.97673919017804));
#51197=CARTESIAN_POINT('Ctrl Pts',(-25.295592502638,-4.81260180106317,-0.132978803016981));
#51198=CARTESIAN_POINT('Ctrl Pts',(-25.0569548375188,-2.48999755919744,
-4.12052561435965));
#51199=CARTESIAN_POINT('Ctrl Pts',(-24.8183171723996,2.12023594681246,-4.32243201928095));
#51200=CARTESIAN_POINT('Ctrl Pts',(-24.5796795072803,4.78255033466597,-0.553201127887688));
#51201=CARTESIAN_POINT('Ctrl Pts',(-24.3410418421611,3.05100401366679,3.72427088853368));
#51202=CARTESIAN_POINT('Ctrl Pts',(-24.1024041770419,-1.48358370303888,
4.58015267461461));
#51203=CARTESIAN_POINT('Ctrl Pts',(-23.8637665119226,-4.65516222209766,
1.22812207654118));
#51204=CARTESIAN_POINT('Ctrl Pts',(-23.6251288468034,-3.54991501369184,
-3.25221809482192));
#51205=CARTESIAN_POINT('Ctrl Pts',(-23.3864911816842,0.816736872430108,
-4.74465594332464));
#51206=CARTESIAN_POINT('Ctrl Pts',(-23.1478535165649,4.43303010358293,-1.87804772118901));
#51207=CARTESIAN_POINT('Ctrl Pts',(-22.9092158514458,3.97657650355884,2.71397465949093));
#51208=CARTESIAN_POINT('Ctrl Pts',(-22.6705781863265,-0.13326743518637,
4.81259378419344));
#51209=CARTESIAN_POINT('Ctrl Pts',(-22.4319405212073,-4.12067491146169,
2.48975047251535));
#51210=CARTESIAN_POINT('Ctrl Pts',(-22.1933028560881,-4.32230487333938,
-2.12049515987218));
#51211=CARTESIAN_POINT('Ctrl Pts',(-21.9546651909688,-0.552914322524486,
-4.78258349567352));
#51212=CARTESIAN_POINT('Ctrl Pts',(-21.7160275258496,3.72445384229878,-3.05078067349642));
#51213=CARTESIAN_POINT('Ctrl Pts',(-21.4773898607304,4.58006369995296,1.4838583643783));
#51214=CARTESIAN_POINT('Ctrl Pts',(-21.2387521956112,1.22784291284316,4.65523586110807));
#51215=CARTESIAN_POINT('Ctrl Pts',(-21.0001145304919,-3.25243097005294,
3.54971997856348));
#51216=CARTESIAN_POINT('Ctrl Pts',(-20.7614768653727,-4.74460695685984,
-0.817021398792471));
#51217=CARTESIAN_POINT('Ctrl Pts',(-20.5228392002535,-1.87778187766528,
-4.43314271832978));
#51218=CARTESIAN_POINT('Ctrl Pts',(-20.2842015351343,2.71421312200688,-3.97641374475733));
#51219=CARTESIAN_POINT('Ctrl Pts',(-20.045563870015,4.81258578377826,0.133556036718511));
#51220=CARTESIAN_POINT('Ctrl Pts',(-19.8069262048958,2.48950335928912,4.12082420945821));
#51221=CARTESIAN_POINT('Ctrl Pts',(-19.5682885397766,-2.12075435614108,
4.32217770366716));
#51222=CARTESIAN_POINT('Ctrl Pts',(-19.3296508746574,-4.7826166442574,0.552627519438542));
#51223=CARTESIAN_POINT('Ctrl Pts',(-19.0910132095381,-3.05055731986689,
-3.72463678489262));
#51224=CARTESIAN_POINT('Ctrl Pts',(-18.8523755444189,1.48413301908516,-4.57997470766269));
#51225=CARTESIAN_POINT('Ctrl Pts',(-18.6137378792997,4.6553094840529,-1.22756374533297));
#51226=CARTESIAN_POINT('Ctrl Pts',(-18.3751002141804,3.54952493031783,3.25264383390203));
#51227=CARTESIAN_POINT('Ctrl Pts',(-18.1364625490612,-0.817305922033317,
4.74455795316888));
#51228=CARTESIAN_POINT('Ctrl Pts',(-17.897824883942,-4.43325531722986,1.87751602747407));
#51229=CARTESIAN_POINT('Ctrl Pts',(-17.6591872188228,-3.97625097160617,
-2.71445157480656));
#51230=CARTESIAN_POINT('Ctrl Pts',(-17.4205495537035,0.133844637744424,
-4.81257776603306));
#51231=CARTESIAN_POINT('Ctrl Pts',(-17.1819118885843,4.1209734926491,-2.4892562371223));
#51232=CARTESIAN_POINT('Ctrl Pts',(-16.9432742234651,4.32205051844462,2.12101354478971));
#51233=CARTESIAN_POINT('Ctrl Pts',(-16.7046365583459,0.55234071436891,4.78264977563894));
#51234=CARTESIAN_POINT('Ctrl Pts',(-16.4659988932266,-3.72481971409399,
3.05033395526876));
#51235=CARTESIAN_POINT('Ctrl Pts',(-16.2273612281074,-4.57988569890107,
-1.48440766845576));
#51236=CARTESIAN_POINT('Ctrl Pts',(-15.9887235629882,-1.22728457340874,
-4.65538309025602));
#51237=CARTESIAN_POINT('Ctrl Pts',(-15.7500858978689,3.25285668605437,-3.54932986930775));
#51238=CARTESIAN_POINT('Ctrl Pts',(-15.5114482327497,4.74450893241555,0.817590442335157));
#51239=CARTESIAN_POINT('Ctrl Pts',(-15.2728105676305,1.8772501705311,4.43336790018713));
#51240=CARTESIAN_POINT('Ctrl Pts',(-15.0341729025113,-2.71469001784463,
3.97608818415582));
#51241=CARTESIAN_POINT('Ctrl Pts',(-14.795535237392,-4.81256973098103,-0.134133238289019));
#51242=CARTESIAN_POINT('Ctrl Pts',(-14.5568975722728,-2.48900910600372,
-4.12112276102026));
#51243=CARTESIAN_POINT('Ctrl Pts',(-14.3182599071536,2.12127272581082,-4.32192331767929));
#51244=CARTESIAN_POINT('Ctrl Pts',(-14.0796222420344,4.78268288982128,-0.552053907312987));
#51245=CARTESIAN_POINT('Ctrl Pts',(-13.8409845769151,3.05011057970114,3.72500262990027));
#51246=CARTESIAN_POINT('Ctrl Pts',(-13.6023469117959,-1.48468231248816,
4.57979667366944));
#51247=CARTESIAN_POINT('Ctrl Pts',(-13.3637092466767,-4.65545667971761,
1.22700539707102));
#51248=CARTESIAN_POINT('Ctrl Pts',(-13.1250715815574,-3.5491347955337,-3.25306952650887));
#51249=CARTESIAN_POINT('Ctrl Pts',(-12.8864339164382,0.817874959696777,
-4.74445989460021));
#51250=CARTESIAN_POINT('Ctrl Pts',(-12.647796251319,4.43348046720131,-1.87698430683722));
#51251=CARTESIAN_POINT('Ctrl Pts',(-12.4091585861998,3.9759253824068,2.71492845112022));
#51252=CARTESIAN_POINT('Ctrl Pts',(-12.1705209210805,-0.134421838351238,
4.81256167862222));
#51253=CARTESIAN_POINT('Ctrl Pts',(-11.9318832559613,-4.12127201457121,
2.48876196593426));
#51254=CARTESIAN_POINT('Ctrl Pts',(-11.6932455908421,-4.32179610137161,
-2.12153189920346));
#51255=CARTESIAN_POINT('Ctrl Pts',(-11.4546079257229,-0.551767098271795,
-4.78271598680431));
#51256=CARTESIAN_POINT('Ctrl Pts',(-11.2159702606036,3.72518553231084,-3.04988719316482));
#51257=CARTESIAN_POINT('Ctrl Pts',(-10.9773325954844,4.57970763196809,1.48495695118139));
#51258=CARTESIAN_POINT('Ctrl Pts',(-10.7386949303652,1.22672621632081,4.65553025243742));
#51259=CARTESIAN_POINT('Ctrl Pts',(-10.500057265246,-3.25328235526483,3.54893970899639));
#51260=CARTESIAN_POINT('Ctrl Pts',(-10.2614196001267,-4.74441083972299,
-0.81815947411722));
#51261=CARTESIAN_POINT('Ctrl Pts',(-10.0227819350075,-1.8767184363934,-4.43359301827195));
#51262=CARTESIAN_POINT('Ctrl Pts',(-9.78414426988828,2.71516687463254,-3.97576256635973));
#51263=CARTESIAN_POINT('Ctrl Pts',(-9.54550660476906,4.8125536089566,0.134710437930172));
#51264=CARTESIAN_POINT('Ctrl Pts',(-9.30686893964983,2.48851481691486,4.12142125330121));
#51265=CARTESIAN_POINT('Ctrl Pts',(-9.06823127453061,-2.12179106496689,
4.32166886952238));
#51266=CARTESIAN_POINT('Ctrl Pts',(-8.82959360941138,-4.78274906658767,
0.551480287245675));
#51267=CARTESIAN_POINT('Ctrl Pts',(-8.59095594429215,-3.04966379566106,
-3.72536842132379));
#51268=CARTESIAN_POINT('Ctrl Pts',(-8.35231827917293,1.48523158453539,-4.57961857379977));
#51269=CARTESIAN_POINT('Ctrl Pts',(-8.1136806140537,4.65560380841346,-1.22644703115444));
#51270=CARTESIAN_POINT('Ctrl Pts',(-7.87504294893448,3.54874460969979,3.25349517231261));
#51271=CARTESIAN_POINT('Ctrl Pts',(-7.63640528381524,-0.818443985601727,
4.74436176780107));
#51272=CARTESIAN_POINT('Ctrl Pts',(-7.39776761869602,-4.43370555338651,
1.87645255916802));
#51273=CARTESIAN_POINT('Ctrl Pts',(-7.1591299535768,-3.97559973603849,-2.71540528831811));
#51274=CARTESIAN_POINT('Ctrl Pts',(-6.92049228845756,0.134999037069343,
-4.81254552210429));
#51275=CARTESIAN_POINT('Ctrl Pts',(-6.68185462333835,4.1215704771241,-2.48826765871595));
#51276=CARTESIAN_POINT('Ctrl Pts',(-6.44321695821911,4.32154162229638,2.12205022265777));
#51277=CARTESIAN_POINT('Ctrl Pts',(-6.20457929309988,0.551193473920355,
4.78278213002022));
#51278=CARTESIAN_POINT('Ctrl Pts',(-5.96594162798067,-3.72555129633323,
3.04944038556121));
#51279=CARTESIAN_POINT('Ctrl Pts',(-5.72730396286143,-4.57952950032639,
-1.48550620942175));
#51280=CARTESIAN_POINT('Ctrl Pts',(-5.48866629774222,-1.22616783934351,
-4.65567735364785));
#51281=CARTESIAN_POINT('Ctrl Pts',(-5.25002863262297,3.25370797337249,-3.54854948612432));
#51282=CARTESIAN_POINT('Ctrl Pts',(-5.01139096750376,4.74431268704714,0.818728472038551));
#51283=CARTESIAN_POINT('Ctrl Pts',(-4.77275330238453,1.87618665939981,4.43381811498155));
#51284=CARTESIAN_POINT('Ctrl Pts',(-4.5341156372653,-2.71564366192391,3.97543680999486));
#51285=CARTESIAN_POINT('Ctrl Pts',(-4.29547797214608,-4.812537476128,-0.135287479444116));
#51286=CARTESIAN_POINT('Ctrl Pts',(-4.05684030702684,-2.48802037989938,
-4.12171998606955));
#51287=CARTESIAN_POINT('Ctrl Pts',(-3.81820264190762,2.12230915839156,-4.32141378384957));
#51288=CARTESIAN_POINT('Ctrl Pts',(-3.5795649767884,4.78281558760628,-0.550907763508576));
#51289=CARTESIAN_POINT('Ctrl Pts',(-3.34092731166917,3.04921617498962,3.72573627855867));
#51290=CARTESIAN_POINT('Ctrl Pts',(-3.10228964654994,-1.48577931367711,
4.57943634031457));
#51291=CARTESIAN_POINT('Ctrl Pts',(-2.86365198143072,-4.65575379041631,
1.22589645476151));
#51292=CARTESIAN_POINT('Ctrl Pts',(-2.62501431631149,-3.54834876796527,
-3.25393575552032));
#51293=CARTESIAN_POINT('Ctrl Pts',(-2.38637665119226,0.819002242401078,
-4.74423481374027));
#51294=CARTESIAN_POINT('Ctrl Pts',(-2.14773898607304,4.43395122223712,-1.87597598138563));
#51295=CARTESIAN_POINT('Ctrl Pts',(-1.90910132095381,3.97523440584382,2.71598802545506));
#51296=CARTESIAN_POINT('Ctrl Pts',(-1.67046365583458,-0.135500177452599,
4.81232596646912));
#51297=CARTESIAN_POINT('Ctrl Pts',(-1.43182599071536,-4.12201486774593,
2.48816358626208));
#51298=CARTESIAN_POINT('Ctrl Pts',(-1.19318832559613,-4.32100676816269,
-2.12331775762679));
#51299=CARTESIAN_POINT('Ctrl Pts',(-0.9545506604769,-0.551158953576692,
-4.78140835552346));
#51300=CARTESIAN_POINT('Ctrl Pts',(-0.715912995357679,3.72696190987269,
-3.05177387808086));
#51301=CARTESIAN_POINT('Ctrl Pts',(-0.477275330238447,4.57725222884596,
1.49154630755727));
#51302=CARTESIAN_POINT('Ctrl Pts',(-0.278410609305757,1.78830202401348,
4.11849926473408));
#51303=CARTESIAN_POINT('Ctrl Pts',(-0.119318832559607,-1.02190788268887,
4.1117895186236));
#51304=CARTESIAN_POINT('Ctrl Pts',(-0.0397729441865359,-2.25151393523441,
3.45825666525491));
#51305=CARTESIAN_POINT('Ctrl Pts',(0.,-2.75129702511903,2.99988915288068));
#51306=CARTESIAN_POINT('Ctrl Pts',(-29.9038972033484,-1.91758108071807,
3.91047455474608));
#51307=CARTESIAN_POINT('Ctrl Pts',(-29.8641242591618,-2.56906817116925,
3.59100455142768));
#51308=CARTESIAN_POINT('Ctrl Pts',(-29.7845783707887,-3.69937650370433,
2.62028213013966));
#51309=CARTESIAN_POINT('Ctrl Pts',(-29.6254865940426,-4.80090108994663,
-0.177550705673484));
#51310=CARTESIAN_POINT('Ctrl Pts',(-29.4266218731099,-3.26962999641403,
-3.98025429162597));
#51311=CARTESIAN_POINT('Ctrl Pts',(-29.1879842079907,1.58917332809701,-4.90296379114112));
#51312=CARTESIAN_POINT('Ctrl Pts',(-28.9493465428715,4.97952485746032,-1.31355913522901));
#51313=CARTESIAN_POINT('Ctrl Pts',(-28.7107088777522,3.79937515632038,3.47876531381764));
#51314=CARTESIAN_POINT('Ctrl Pts',(-28.472071212633,-0.873611211930994,
5.07706565551933));
#51315=CARTESIAN_POINT('Ctrl Pts',(-28.2334335475137,-4.74281745578375,
2.00987801671541));
#51316=CARTESIAN_POINT('Ctrl Pts',(-27.9947958823946,-4.25527592056482,
-2.90329400887223));
#51317=CARTESIAN_POINT('Ctrl Pts',(-27.7561582172753,0.142022194137876,
-5.14941429154002));
#51318=CARTESIAN_POINT('Ctrl Pts',(-27.5175205521561,4.40867522944874,-2.66447767738084));
#51319=CARTESIAN_POINT('Ctrl Pts',(-27.2788828870369,4.62504309400783,2.26831074393387));
#51320=CARTESIAN_POINT('Ctrl Pts',(-27.0402452219176,0.59221161082695,5.1171798486122));
#51321=CARTESIAN_POINT('Ctrl Pts',(-26.8016075567984,-3.98467759576748,
3.26473395232318));
#51322=CARTESIAN_POINT('Ctrl Pts',(-26.5629698916792,-4.90074595455584,
-1.58710200816697));
#51323=CARTESIAN_POINT('Ctrl Pts',(-26.3243322265599,-1.31435770042331,
-4.9808293387569));
#51324=CARTESIAN_POINT('Ctrl Pts',(-26.0856945614408,3.47956385870106,-3.79852863154653));
#51325=CARTESIAN_POINT('Ctrl Pts',(-25.8470568963215,5.07671600609805,0.873583386925484));
#51326=CARTESIAN_POINT('Ctrl Pts',(-25.6084192312023,2.00974846033062,4.74311109629157));
#51327=CARTESIAN_POINT('Ctrl Pts',(-25.3697815660831,-2.90362987147378,
4.25501160863666));
#51328=CARTESIAN_POINT('Ctrl Pts',(-25.1311439009638,-5.14936372539749,
-0.14228399788883));
#51329=CARTESIAN_POINT('Ctrl Pts',(-24.8925062358446,-2.66423519702527,
-4.40885949123555));
#51330=CARTESIAN_POINT('Ctrl Pts',(-24.6538685707254,2.26859950710815,-4.62489430159482));
#51331=CARTESIAN_POINT('Ctrl Pts',(-24.4152309056061,5.11720940693162,-0.591911389835893));
#51332=CARTESIAN_POINT('Ctrl Pts',(-24.1765932404869,3.26449809135411,3.98487683164073));
#51333=CARTESIAN_POINT('Ctrl Pts',(-23.9379555753677,-1.58739750758757,
4.90064896585306));
#51334=CARTESIAN_POINT('Ctrl Pts',(-23.6993179102485,-4.9809073081872,1.31405994776134));
#51335=CARTESIAN_POINT('Ctrl Pts',(-23.4606802451292,-3.79832040035196,
-3.47979213257527));
#51336=CARTESIAN_POINT('Ctrl Pts',(-23.22204258001,0.873888054307114,-5.07666335466403));
#51337=CARTESIAN_POINT('Ctrl Pts',(-22.9834049148908,4.74323148944965,-2.00946415469484));
#51338=CARTESIAN_POINT('Ctrl Pts',(-22.7447672497716,4.25483753801745,2.90388510018491));
#51339=CARTESIAN_POINT('Ctrl Pts',(-22.5061295846524,-0.142592827101065,
5.14935514754711));
#51340=CARTESIAN_POINT('Ctrl Pts',(-22.2674919195331,-4.40901923540582,
2.66397082044679));
#51341=CARTESIAN_POINT('Ctrl Pts',(-22.0288542544139,-4.624758258613,-2.26887685860782));
#51342=CARTESIAN_POINT('Ctrl Pts',(-21.7902165892947,-0.591604515260647,
-5.11724488838146));
#51343=CARTESIAN_POINT('Ctrl Pts',(-21.5515789241754,3.98507258759985,-3.26425912295005));
#51344=CARTESIAN_POINT('Ctrl Pts',(-21.3129412590562,4.90055376518737,1.58769138836067));
#51345=CARTESIAN_POINT('Ctrl Pts',(-21.074303593937,1.31376124957698,4.98098610008909));
#51346=CARTESIAN_POINT('Ctrl Pts',(-20.8356659288178,-3.4800199037556,3.7981117176359));
#51347=CARTESIAN_POINT('Ctrl Pts',(-20.5970282636985,-5.0766109403702,-0.874192490408381));
#51348=CARTESIAN_POINT('Ctrl Pts',(-20.3583905985793,-2.00917970876428,
-4.74335198441606));
#51349=CARTESIAN_POINT('Ctrl Pts',(-20.11975293346,2.90414024912104,-4.25466339016496));
#51350=CARTESIAN_POINT('Ctrl Pts',(-19.8811152683409,5.14934658730268,0.142901623532206));
#51351=CARTESIAN_POINT('Ctrl Pts',(-19.6424776032216,2.66370641546674,4.40917898053317));
#51352=CARTESIAN_POINT('Ctrl Pts',(-19.4038399381024,-2.26915419214175,
4.62462219023996));
#51353=CARTESIAN_POINT('Ctrl Pts',(-19.1652022729832,-5.11728035653827,
0.591297643122014));
#51354=CARTESIAN_POINT('Ctrl Pts',(-18.9265646078639,-3.26402014014505,
-3.985268331606));
#51355=CARTESIAN_POINT('Ctrl Pts',(-18.6879269427447,1.58798526203712,-4.90045854565949));
#51356=CARTESIAN_POINT('Ctrl Pts',(-18.4492892776255,4.98106487480121,-1.31346254731367));
#51357=CARTESIAN_POINT('Ctrl Pts',(-18.2106516125063,3.79790302088468,3.48024766275753));
#51358=CARTESIAN_POINT('Ctrl Pts',(-17.9720139473871,-0.874496923169711,
5.07655850764482));
#51359=CARTESIAN_POINT('Ctrl Pts',(-17.7333762822678,-4.74347246242682,
2.00889525569968));
#51360=CARTESIAN_POINT('Ctrl Pts',(-17.4947386171486,-4.25448922695873,
-2.90439538766098));
#51361=CARTESIAN_POINT('Ctrl Pts',(-17.2561009520293,0.143210419421708,
-5.14933800851558));
#51362=CARTESIAN_POINT('Ctrl Pts',(-17.0174632869101,4.40933870981885,-2.66344200092047));
#51363=CARTESIAN_POINT('Ctrl Pts',(-16.7788256217909,4.62448610522848,2.26943151752217));
#51364=CARTESIAN_POINT('Ctrl Pts',(-16.5401879566717,0.590990768860884,
5.11731580628902));
#51365=CARTESIAN_POINT('Ctrl Pts',(-16.3015502915524,-3.98546406128254,
3.2637811456039));
#51366=CARTESIAN_POINT('Ctrl Pts',(-16.0629126264332,-4.90036330850768,
-1.58827913000388));
#51367=CARTESIAN_POINT('Ctrl Pts',(-15.824274961314,-1.31316384032749,-4.98114363160013));
#51368=CARTESIAN_POINT('Ctrl Pts',(-15.5856372961948,3.48047540924424,-3.79769431047581));
#51369=CARTESIAN_POINT('Ctrl Pts',(-15.3469996310755,5.07650605666312,0.874801352786364));
#51370=CARTESIAN_POINT('Ctrl Pts',(-15.1083619659563,2.00861079541087,4.74359292337918));
#51371=CARTESIAN_POINT('Ctrl Pts',(-14.8697243008371,-2.90465051575626,
4.25431504845271));
#51372=CARTESIAN_POINT('Ctrl Pts',(-14.6310866357179,-5.1493294112106,-0.143519214796206));
#51373=CARTESIAN_POINT('Ctrl Pts',(-14.3924489705986,-2.66317757679605,
-4.4094984232478));
#51374=CARTESIAN_POINT('Ctrl Pts',(-14.1538113054794,2.26970883474132,-4.62435000358661));
#51375=CARTESIAN_POINT('Ctrl Pts',(-13.9151736403602,5.11735123763705,-0.590683892474468));
#51376=CARTESIAN_POINT('Ctrl Pts',(-13.676535975241,3.26354213932567,3.98565977662667));
#51377=CARTESIAN_POINT('Ctrl Pts',(-13.4378983101217,-1.58857299225892,
4.90026805373337));
#51378=CARTESIAN_POINT('Ctrl Pts',(-13.1992606450025,-4.98122237048603,
1.31286512861896));
#51379=CARTESIAN_POINT('Ctrl Pts',(-12.9606229798833,-3.79748558640983,
-3.48070314321456));
#51380=CARTESIAN_POINT('Ctrl Pts',(-12.7219853147641,0.87510577925706,-5.0764535874255));
#51381=CARTESIAN_POINT('Ctrl Pts',(-12.4833476496448,4.74371336727283,-2.00832632789875));
#51382=CARTESIAN_POINT('Ctrl Pts',(-12.2447099845256,4.25414085464746,2.90490563340592));
#51383=CARTESIAN_POINT('Ctrl Pts',(-12.0060723194064,-0.143828009654572,
5.14932079538778));
#51384=CARTESIAN_POINT('Ctrl Pts',(-11.7674346542871,-4.40965812081948,
2.66291314309442));
#51385=CARTESIAN_POINT('Ctrl Pts',(-11.5287969891679,-4.6242138853148,-2.26998614379823));
#51386=CARTESIAN_POINT('Ctrl Pts',(-11.2901593240487,-0.590377013963862,
-5.11738665058224));
#51387=CARTESIAN_POINT('Ctrl Pts',(-11.0515216589295,3.98585547763773,-3.26330312131122));
#51388=CARTESIAN_POINT('Ctrl Pts',(-10.8128839938102,4.90017278133687,1.58886684880117));
#51389=CARTESIAN_POINT('Ctrl Pts',(-10.574246328691,1.31256641218918,4.98130109145864));
#51390=CARTESIAN_POINT('Ctrl Pts',(-10.3356086635718,-3.48093086466773,
3.79727684868749));
#51391=CARTESIAN_POINT('Ctrl Pts',(-10.0969709984526,-5.07640109993208,
-0.875410202580779));
#51392=CARTESIAN_POINT('Ctrl Pts',(-9.85833333333333,-2.00804185316436,
-4.74383379410727));
#51393=CARTESIAN_POINT('Ctrl Pts',(-9.61969566821411,2.90516074060913,-4.25396664554368));
#51394=CARTESIAN_POINT('Ctrl Pts',(-9.38105800309488,5.14931216104712,0.14413680399584));
#51395=CARTESIAN_POINT('Ctrl Pts',(-9.14242033797565,2.66264869981656,4.40981780253313));
#51396=CARTESIAN_POINT('Ctrl Pts',(-8.90378267285642,-2.27026344469205,
4.62407775041392));
#51397=CARTESIAN_POINT('Ctrl Pts',(-8.6651450077372,-5.11742204512421,0.590070133329444));
#51398=CARTESIAN_POINT('Ctrl Pts',(-8.42650734261798,-3.26306409156187,
-3.98605116431367));
#51399=CARTESIAN_POINT('Ctrl Pts',(-8.18786967749874,1.58916069963059,-4.90007749132113));
#51400=CARTESIAN_POINT('Ctrl Pts',(-7.94923201237953,4.98137979451584,-1.31226769103422));
#51401=CARTESIAN_POINT('Ctrl Pts',(-7.71059434726029,3.79706809731301,3.48115857359343));
#51402=CARTESIAN_POINT('Ctrl Pts',(-7.47195668214107,-0.875714622763106,
5.07634859420128));
#51403=CARTESIAN_POINT('Ctrl Pts',(-7.23331901702185,-4.74395420386913,
2.00775737117387));
#51404=CARTESIAN_POINT('Ctrl Pts',(-6.99468135190261,-4.25379242116686,
-2.90541583729795));
#51405=CARTESIAN_POINT('Ctrl Pts',(-6.7560436867834,0.144445597866564,-5.14930350831713));
#51406=CARTESIAN_POINT('Ctrl Pts',(-6.51740602166415,4.40997746829655,-2.66238424671687));
#51407=CARTESIAN_POINT('Ctrl Pts',(-6.27876835654495,4.62394159906029,2.27054073694845));
#51408=CARTESIAN_POINT('Ctrl Pts',(-6.04013069142569,0.58976325023493,5.11745742217124));
#51409=CARTESIAN_POINT('Ctrl Pts',(-5.80149302630649,-3.9862468360062,3.26282504833503));
#51410=CARTESIAN_POINT('Ctrl Pts',(-5.56285536118725,-4.89998218492935,
-1.58945454139984));
#51411=CARTESIAN_POINT('Ctrl Pts',(-5.32421769606804,-1.31196896276975,
-4.98145848607974));
#51412=CARTESIAN_POINT('Ctrl Pts',(-5.08558003094879,3.48138626541249,-3.79685931996075));
#51413=CARTESIAN_POINT('Ctrl Pts',(-4.84694236582958,5.07629607902044,0.876019016145047));
#51414=CARTESIAN_POINT('Ctrl Pts',(-4.60830470071035,2.00747286506312,4.74407464196444));
#51415=CARTESIAN_POINT('Ctrl Pts',(-4.36966703559112,-2.90567089110244,
4.25361809436949));
#51416=CARTESIAN_POINT('Ctrl Pts',(-4.1310293704719,-5.14929489932346,-0.144754224003302));
#51417=CARTESIAN_POINT('Ctrl Pts',(-3.89239170535267,-2.66211966455929,
-4.41013743913397));
#51418=CARTESIAN_POINT('Ctrl Pts',(-3.65375404023344,2.27081779171631,-4.62380481511515));
#51419=CARTESIAN_POINT('Ctrl Pts',(-3.41511637511422,5.11749322095267,-0.589457547230361));
#51420=CARTESIAN_POINT('Ctrl Pts',(-3.17647870999498,3.26258514862341,3.98644476236722));
#51421=CARTESIAN_POINT('Ctrl Pts',(-2.93784104487577,-1.58974675613189,
4.89988250604351));
#51422=CARTESIAN_POINT('Ctrl Pts',(-2.69920337975654,-4.98154027151287,
1.31167858804524));
#51423=CARTESIAN_POINT('Ctrl Pts',(-2.46056571463731,-3.79664455654379,
-3.48162998662147));
#51424=CARTESIAN_POINT('Ctrl Pts',(-2.22192804951808,0.876311943595137,
-5.07621275652709));
#51425=CARTESIAN_POINT('Ctrl Pts',(-1.98329038439886,4.74421706340335,-2.00724744484995));
#51426=CARTESIAN_POINT('Ctrl Pts',(-1.74465271927963,4.25340152698323,2.90603935147979));
#51427=CARTESIAN_POINT('Ctrl Pts',(-1.5060150541604,-0.144981805559941,
5.14906858927122));
#51428=CARTESIAN_POINT('Ctrl Pts',(-1.26737738904118,-4.41045295516259,
2.66227289179059));
#51429=CARTESIAN_POINT('Ctrl Pts',(-1.02873972392195,-4.62336931849601,
-2.27189696770677));
#51430=CARTESIAN_POINT('Ctrl Pts',(-0.790102058802722,-0.589726314329404,
-5.11598751777173));
#51431=CARTESIAN_POINT('Ctrl Pts',(-0.551464393683503,3.98775615726128,
-3.26532182704867));
#51432=CARTESIAN_POINT('Ctrl Pts',(-0.312826728564268,4.89754556132347,
1.5959172955446));
#51433=CARTESIAN_POINT('Ctrl Pts',(-0.11396200763158,1.91343850024653,4.40669134774724));
#51434=CARTESIAN_POINT('Ctrl Pts',(0.0451297691145716,-1.09341591083915,
4.39951208699472));
#51435=CARTESIAN_POINT('Ctrl Pts',(0.124675657487642,-2.40906367586066,
3.7002482568252));
#51436=CARTESIAN_POINT('Ctrl Pts',(0.164448601674178,-2.94381909922654,
3.20980646698106));
#51437=CARTESIAN_POINT('Ctrl Pts',(-29.7394486016742,-2.04298847651428,
4.16621468233147));
#51438=CARTESIAN_POINT('Ctrl Pts',(-29.6996756574876,-2.73708200495646,
3.82585174178397));
#51439=CARTESIAN_POINT('Ctrl Pts',(-29.6201297691146,-3.94131108371467,
2.79164529256157));
#51440=CARTESIAN_POINT('Ctrl Pts',(-29.4610379923684,-5.11487399530094,
-0.189162298968872));
#51441=CARTESIAN_POINT('Ctrl Pts',(-29.2621732714358,-3.48345969425087,
-4.2405579264181));
#51442=CARTESIAN_POINT('Ctrl Pts',(-29.0235356063165,1.69310326907807,-5.22361146904792));
#51443=CARTESIAN_POINT('Ctrl Pts',(-28.7848979411973,5.30517953300752,-1.39946425393815));
#51444=CARTESIAN_POINT('Ctrl Pts',(-28.546260276078,4.04784952269694,3.70627219891307));
#51445=CARTESIAN_POINT('Ctrl Pts',(-28.3076226109588,-0.930744288664083,
5.4090993768297));
#51446=CARTESIAN_POINT('Ctrl Pts',(-28.0689849458396,-5.05299176436839,
2.14132151627792));
#51447=CARTESIAN_POINT('Ctrl Pts',(-27.8303472807204,-4.53356562469179,
-3.09316579293629));
#51448=CARTESIAN_POINT('Ctrl Pts',(-27.5917096156012,0.151310267373015,
-5.48617952283658));
#51449=CARTESIAN_POINT('Ctrl Pts',(-27.3530719504819,4.69699705583506,-2.83873117311958));
#51450=CARTESIAN_POINT('Ctrl Pts',(-27.1144342853627,4.92751510715875,2.4166554194804));
#51451=CARTESIAN_POINT('Ctrl Pts',(-26.8757966202434,0.630941506851146,
5.45183698780086));
#51452=CARTESIAN_POINT('Ctrl Pts',(-26.6371589551242,-4.2452705090985,3.47824345502183));
#51453=CARTESIAN_POINT('Ctrl Pts',(-26.398521290005,-5.22124858873371,-1.69089648742445));
#51454=CARTESIAN_POINT('Ctrl Pts',(-26.1598836248858,-1.40031504429382,
-5.30656932574355));
#51455=CARTESIAN_POINT('Ctrl Pts',(-25.9212459597666,3.70712296762955,-4.0469476362654));
#51456=CARTESIAN_POINT('Ctrl Pts',(-25.6826082946473,5.40872686077514,0.930714643938138));
#51457=CARTESIAN_POINT('Ctrl Pts',(-25.4439706295281,2.14118348706817,5.05330460859686));
#51458=CARTESIAN_POINT('Ctrl Pts',(-25.2053329644089,-3.09352362053041,
4.53328402709528));
#51459=CARTESIAN_POINT('Ctrl Pts',(-24.9666952992896,-5.4861256497318,-0.151589192760673));
#51460=CARTESIAN_POINT('Ctrl Pts',(-24.7280576341705,-2.8384728348531,-4.69719336811145));
#51461=CARTESIAN_POINT('Ctrl Pts',(-24.4894199690512,2.41696306740383,-4.92735658390869));
#51462=CARTESIAN_POINT('Ctrl Pts',(-24.250782303932,5.45186847919727,-0.6306216517841));
#51463=CARTESIAN_POINT('Ctrl Pts',(-24.0121446388127,3.47799216904142,4.24548277474778));
#51464=CARTESIAN_POINT('Ctrl Pts',(-23.7735069736936,-1.69121131213625,
5.22114525709151));
#51465=CARTESIAN_POINT('Ctrl Pts',(-23.5348693085742,-5.30665239427673,
1.39999781898149));
#51466=CARTESIAN_POINT('Ctrl Pts',(-23.2962316434551,-4.04672578701207,
-3.70736617032861));
#51467=CARTESIAN_POINT('Ctrl Pts',(-23.0575939783358,0.931039236184116,
-5.40867076600343));
#51468=CARTESIAN_POINT('Ctrl Pts',(-22.8189563132166,5.05343287531637,-2.14088058820066));
#51469=CARTESIAN_POINT('Ctrl Pts',(-22.5803186480974,4.53309857247606,3.09379554087889));
#51470=CARTESIAN_POINT('Ctrl Pts',(-22.3416809829782,-0.151918219015756,
5.48611651090078));
#51471=CARTESIAN_POINT('Ctrl Pts',(-22.1030433178589,-4.69736355934995,
2.83819116837823));
#51472=CARTESIAN_POINT('Ctrl Pts',(-21.8644056527397,-4.92721164388661,
-2.41725855734347));
#51473=CARTESIAN_POINT('Ctrl Pts',(-21.6257679876205,-0.630294707996812,
-5.45190628108939));
#51474=CARTESIAN_POINT('Ctrl Pts',(-21.3871303225012,4.24569133290092,-3.47773757240369));
#51475=CARTESIAN_POINT('Ctrl Pts',(-21.1484926573821,5.22104383042178,1.69152441234305));
#51476=CARTESIAN_POINT('Ctrl Pts',(-20.9098549922628,1.39967958631079,5.3067363390701));
#51477=CARTESIAN_POINT('Ctrl Pts',(-20.6712173271436,-3.70760883745824,
4.04650345670832));
#51478=CARTESIAN_POINT('Ctrl Pts',(-20.4325796620243,-5.40861492388057,
-0.931363582024293));
#51479=CARTESIAN_POINT('Ctrl Pts',(-20.1939419969051,-2.14057753986328,
-5.05356125050234));
#51480=CARTESIAN_POINT('Ctrl Pts',(-19.9553043317859,3.09406737623519,-4.5329130355726));
#51481=CARTESIAN_POINT('Ctrl Pts',(-19.7166666666667,5.48610739082711,0.152247210345901));
#51482=CARTESIAN_POINT('Ctrl Pts',(-19.4780290015475,2.83790947164436,4.69753375160813));
#51483=CARTESIAN_POINT('Ctrl Pts',(-19.2393913364282,-2.41755402814241,
4.92706667681276));
#51484=CARTESIAN_POINT('Ctrl Pts',(-19.000753671309,-5.45194406881915,0.62996776680549));
#51485=CARTESIAN_POINT('Ctrl Pts',(-18.7621160061898,-3.4774829604232,-4.24589987831939));
#51486=CARTESIAN_POINT('Ctrl Pts',(-18.5234783410705,1.69183750498908,-5.22094238365629));
#51487=CARTESIAN_POINT('Ctrl Pts',(-18.2848406759513,5.30682026554953,-1.39936134929439));
#51488=CARTESIAN_POINT('Ctrl Pts',(-18.0462030108321,4.04628111145152,3.70785149161303));
#51489=CARTESIAN_POINT('Ctrl Pts',(-17.8075653457129,-0.931687924306101,
5.40855906212076));
#51490=CARTESIAN_POINT('Ctrl Pts',(-17.5689276805936,-5.05368960762378,
2.14027448392529));
#51491=CARTESIAN_POINT('Ctrl Pts',(-17.3302900154744,-4.53272748231129,
-3.0943392005154));
#51492=CARTESIAN_POINT('Ctrl Pts',(-17.0916523503552,0.152576201098992,
-5.4860982509981));
#51493=CARTESIAN_POINT('Ctrl Pts',(-16.8530146852359,4.6977039269886,-2.83762776471865));
#51494=CARTESIAN_POINT('Ctrl Pts',(-16.6143770201167,4.92692169201234,2.41784949025462));
#51495=CARTESIAN_POINT('Ctrl Pts',(-16.3757393549975,0.62964082335285,5.45198183693909));
#51496=CARTESIAN_POINT('Ctrl Pts',(-16.1371016898783,-4.24610840847109,
3.47722833593904));
#51497=CARTESIAN_POINT('Ctrl Pts',(-15.898464024759,-5.2208409181143,-1.69215059155202));
#51498=CARTESIAN_POINT('Ctrl Pts',(-15.6598263596398,-1.39904310724623,
-5.30690417294424));
#51499=CARTESIAN_POINT('Ctrl Pts',(-15.4211886945206,3.70809413243411,-4.04605875164388));
#51500=CARTESIAN_POINT('Ctrl Pts',(-15.1825510294014,5.40850318091069,0.932012263237568));
#51501=CARTESIAN_POINT('Ctrl Pts',(-14.9439133642821,2.13997142029063,5.05381794657124));
#51502=CARTESIAN_POINT('Ctrl Pts',(-14.7052756991629,-3.09461101366789,
4.53254191274959));
#51503=CARTESIAN_POINT('Ctrl Pts',(-14.4666380340437,-5.48608909144016,
-0.152905191303383));
#51504=CARTESIAN_POINT('Ctrl Pts',(-14.2280003689245,-2.83734604758839,
-4.69787408547534));
#51505=CARTESIAN_POINT('Ctrl Pts',(-13.9893627038052,2.41814494367183,-4.92677668949392));
#51506=CARTESIAN_POINT('Ctrl Pts',(-13.750725038686,5.45201958545282,-0.629313877635948));
#51507=CARTESIAN_POINT('Ctrl Pts',(-13.5120873735668,3.47697369895021,4.24631692335307));
#51508=CARTESIAN_POINT('Ctrl Pts',(-13.2734497084476,-1.69246367202968,
5.2207394337973));
#51509=CARTESIAN_POINT('Ctrl Pts',(-13.0348120433283,-5.30698806125446,
1.3987248601669));
#51510=CARTESIAN_POINT('Ctrl Pts',(-12.7961743782091,-4.04583637728596,
-3.70833675992024));
#51511=CARTESIAN_POINT('Ctrl Pts',(-12.5575367130899,0.932336598817344,
-5.40844728025078));
#51512=CARTESIAN_POINT('Ctrl Pts',(-12.3188990479706,5.05394626734435,-2.13966834896028));
#51513=CARTESIAN_POINT('Ctrl Pts',(-12.0802613828514,4.53235632688813,3.09488281569163));
#51514=CARTESIAN_POINT('Ctrl Pts',(-11.8416237177322,-0.153234180957902,
5.48607991215335));
#51515=CARTESIAN_POINT('Ctrl Pts',(-11.602986052613,-4.69804422706777,2.83706432025457));
#51516=CARTESIAN_POINT('Ctrl Pts',(-11.3643483874937,-4.92663166925799,
-2.41844038839298));
#51517=CARTESIAN_POINT('Ctrl Pts',(-11.1257107223745,-0.628986929655938,
-5.45205731436018));
#51518=CARTESIAN_POINT('Ctrl Pts',(-10.8870730572553,4.24652542296462,-3.47671904945761));
#51519=CARTESIAN_POINT('Ctrl Pts',(-10.6484353921361,5.22063793070565,1.69277674642096));
#51520=CARTESIAN_POINT('Ctrl Pts',(-10.4097977270168,1.39840660805754,5.30707193047986));
#51521=CARTESIAN_POINT('Ctrl Pts',(-10.1711600618976,-3.70857937407062,
4.04561398837858));
#51522=CARTESIAN_POINT('Ctrl Pts',(-9.93252239677838,-5.40839136014118,
-0.93266093104433));
#51523=CARTESIAN_POINT('Ctrl Pts',(-9.69388473165915,-2.13936526993532,
-5.05407456994261));
#51524=CARTESIAN_POINT('Ctrl Pts',(-9.45524706653993,3.09515460658571,-4.53217072472762));
#51525=CARTESIAN_POINT('Ctrl Pts',(-9.21660940142069,5.48607071313765,0.153563170061505));
#51526=CARTESIAN_POINT('Ctrl Pts',(-8.97797173630149,2.83678258271826,4.69821435176505));
#51527=CARTESIAN_POINT('Ctrl Pts',(-8.73933407118223,-2.41873582441721,
4.92648663130547));
#51528=CARTESIAN_POINT('Ctrl Pts',(-8.50069640606304,-5.45209502366077,
0.628659979413207));
#51529=CARTESIAN_POINT('Ctrl Pts',(-8.26205874094379,-3.47646438746268,
-4.24673390730354));
#51530=CARTESIAN_POINT('Ctrl Pts',(-8.02342107582457,1.69308981472579,-5.22053640884249));
#51531=CARTESIAN_POINT('Ctrl Pts',(-7.78478341070535,5.30715578061822,-1.398088350914));
#51532=CARTESIAN_POINT('Ctrl Pts',(-7.54614574558612,4.04539158492623,3.70882197487425));
#51533=CARTESIAN_POINT('Ctrl Pts',(-7.30750808046689,-0.932985259924489,
5.40833542060147));
#51534=CARTESIAN_POINT('Ctrl Pts',(-7.06887041534766,-5.05420285435175,
2.13906218317974));
#51535=CARTESIAN_POINT('Ctrl Pts',(-6.83023275022844,-4.53198510629524,
-3.09542638627781));
#51536=CARTESIAN_POINT('Ctrl Pts',(-6.5915950851092,0.153892158663785,-5.48606149452997));
#51537=CARTESIAN_POINT('Ctrl Pts',(-6.35295741998999,4.69838445946899,-2.83650083471779));
#51538=CARTESIAN_POINT('Ctrl Pts',(-6.11431975487076,4.92634157582419,2.41903125123913));
#51539=CARTESIAN_POINT('Ctrl Pts',(-5.87568208975152,0.628333026549508,
5.45213271432227));
#51540=CARTESIAN_POINT('Ctrl Pts',(-5.63704442463231,-4.24694237567916,
3.47620971110884));
#51541=CARTESIAN_POINT('Ctrl Pts',(-5.39840675951308,-5.22043486953231,
-1.69340287337793));
#51542=CARTESIAN_POINT('Ctrl Pts',(-5.15976909439385,-1.39777008619599,
-5.30723961851162));
#51543=CARTESIAN_POINT('Ctrl Pts',(-4.92113142927462,3.70906455745249,-4.04516915379718));
#51544=CARTESIAN_POINT('Ctrl Pts',(-4.6824937641554,5.40827947099373,0.933309560251545));
#51545=CARTESIAN_POINT('Ctrl Pts',(-4.44385609903617,2.13875907072644,5.05433116894732));
#51546=CARTESIAN_POINT('Ctrl Pts',(-4.20521843391694,-3.09569812028096,
4.53179937874414));
#51547=CARTESIAN_POINT('Ctrl Pts',(-3.96658076879772,-5.48605232251892,
-0.154220968562498));
#51548=CARTESIAN_POINT('Ctrl Pts',(-3.72794310367849,-2.83621894921919,
-4.69855489219838));
#51549=CARTESIAN_POINT('Ctrl Pts',(-3.48930543855926,2.41932642504106,-4.92619584638074));
#51550=CARTESIAN_POINT('Ctrl Pts',(-3.25066777344004,5.45217085429907,-0.62800733095214));
#51551=CARTESIAN_POINT('Ctrl Pts',(-3.01203010832081,3.47595412225719,4.24715324617577));
#51552=CARTESIAN_POINT('Ctrl Pts',(-2.77339244320158,-1.69371419858668,
5.22032867177245));
#51553=CARTESIAN_POINT('Ctrl Pts',(-2.53475477808237,-5.30732675260943,
1.39746072132896));
#51554=CARTESIAN_POINT('Ctrl Pts',(-2.29611711296313,-4.04494034512231,
-3.70932421772263));
#51555=CARTESIAN_POINT('Ctrl Pts',(-2.05747944784391,0.933621644789192,
-5.40819069931389));
#51556=CARTESIAN_POINT('Ctrl Pts',(-1.81884178272468,5.05448290456958,-2.13851890831426));
#51557=CARTESIAN_POINT('Ctrl Pts',(-1.58020411760545,4.53156864812263,3.09609067750451));
#51558=CARTESIAN_POINT('Ctrl Pts',(-1.34156645248623,-0.154463433667277,
5.48581121207333));
#51559=CARTESIAN_POINT('Ctrl Pts',(-1.102928787367,-4.69889104257927,2.83638219731909));
#51560=CARTESIAN_POINT('Ctrl Pts',(-0.86429112224777,-4.92573186882932,
-2.42047617778675));
#51561=CARTESIAN_POINT('Ctrl Pts',(-0.625653457128544,-0.628293675082119,
-5.45056668002));
#51562=CARTESIAN_POINT('Ctrl Pts',(-0.387015792009324,4.24855040464988,
-3.47886977601648));
#51563=CARTESIAN_POINT('Ctrl Pts',(-0.14837812689009,5.21783889380097,1.70028828353193));
#51564=CARTESIAN_POINT('Ctrl Pts',(0.0504865940425981,2.03857497647958,
4.69488343076037));
#51565=CARTESIAN_POINT('Ctrl Pts',(0.209578370788749,-1.16492393898944,
4.68723465536585));
#51566=CARTESIAN_POINT('Ctrl Pts',(0.28912425916182,-2.56661341648691,3.94223984839548));
#51567=CARTESIAN_POINT('Ctrl Pts',(0.328897203348356,-3.13634117333406,
3.41972378108145));
#51568=CARTESIAN_POINT('Ctrl Pts',(-29.575,-2.16839587231048,4.42195480991686));
#51569=CARTESIAN_POINT('Ctrl Pts',(-29.5352270558135,-2.90509583874368,
4.06069893214025));
#51570=CARTESIAN_POINT('Ctrl Pts',(-29.4556811674404,-4.18324566372502,
2.96300845498348));
#51571=CARTESIAN_POINT('Ctrl Pts',(-29.2965893906942,-5.42884690065524,
-0.200773892264263));
#51572=CARTESIAN_POINT('Ctrl Pts',(-29.0977246697616,-3.69728939208772,
-4.50086156121024));
#51573=CARTESIAN_POINT('Ctrl Pts',(-28.8590870046423,1.79703321005912,-5.54425914695472));
#51574=CARTESIAN_POINT('Ctrl Pts',(-28.6204493395231,5.63083420855472,-1.48536937264729));
#51575=CARTESIAN_POINT('Ctrl Pts',(-28.3818116744038,4.2963238890735,3.93377908400849));
#51576=CARTESIAN_POINT('Ctrl Pts',(-28.1431740092847,-0.987877365397176,
5.74113309814008));
#51577=CARTESIAN_POINT('Ctrl Pts',(-27.9045363441654,-5.36316607295304,
2.27276501584044));
#51578=CARTESIAN_POINT('Ctrl Pts',(-27.6658986790462,-4.81185532881875,
-3.28303757700034));
#51579=CARTESIAN_POINT('Ctrl Pts',(-27.4272610139269,0.160598340608156,
-5.82294475413315));
#51580=CARTESIAN_POINT('Ctrl Pts',(-27.1886233488077,4.98531888222138,-3.01298466885832));
#51581=CARTESIAN_POINT('Ctrl Pts',(-26.9499856836885,5.22998712030967,2.56500009502694));
#51582=CARTESIAN_POINT('Ctrl Pts',(-26.7113480185693,0.669671402875337,
5.78649412698952));
#51583=CARTESIAN_POINT('Ctrl Pts',(-26.4727103534501,-4.50586342242951,
3.69175295772048));
#51584=CARTESIAN_POINT('Ctrl Pts',(-26.2340726883308,-5.54175122291158,
-1.79469096668193));
#51585=CARTESIAN_POINT('Ctrl Pts',(-25.9954350232117,-1.48627238816434,
-5.6323093127302));
#51586=CARTESIAN_POINT('Ctrl Pts',(-25.7567973580923,3.93468207655805,-4.29536664098428));
#51587=CARTESIAN_POINT('Ctrl Pts',(-25.5181596929732,5.74073771545223,0.987845900950795));
#51588=CARTESIAN_POINT('Ctrl Pts',(-25.2795220278539,2.27261851380574,5.36349812090215));
#51589=CARTESIAN_POINT('Ctrl Pts',(-25.0408843627347,-3.28341736958705,
4.8115564455539));
#51590=CARTESIAN_POINT('Ctrl Pts',(-24.8022466976155,-5.82288757406612,
-0.160894387632515));
#51591=CARTESIAN_POINT('Ctrl Pts',(-24.5636090324963,-3.01271047268094,
-4.98552724498736));
#51592=CARTESIAN_POINT('Ctrl Pts',(-24.324971367377,2.56532662769952,-5.22981886622255));
#51593=CARTESIAN_POINT('Ctrl Pts',(-24.0863337022578,5.78652755146292,-0.669331913732308));
#51594=CARTESIAN_POINT('Ctrl Pts',(-23.8476960371386,3.69148624672874,4.50608871785483));
#51595=CARTESIAN_POINT('Ctrl Pts',(-23.6090583720193,-1.79502511668494,
5.54164154832996));
#51596=CARTESIAN_POINT('Ctrl Pts',(-23.3704207069001,-5.63239748036626,
1.48593569020165));
#51597=CARTESIAN_POINT('Ctrl Pts',(-23.1317830417809,-4.29513117367219,
-3.93494020808196));
#51598=CARTESIAN_POINT('Ctrl Pts',(-22.8931453766617,0.988190418061122,
-5.74067817734282));
#51599=CARTESIAN_POINT('Ctrl Pts',(-22.6545077115424,5.36363426118309,-2.27229702170649));
#51600=CARTESIAN_POINT('Ctrl Pts',(-22.4158700464232,4.81135960693467,3.28370598157288));
#51601=CARTESIAN_POINT('Ctrl Pts',(-22.177232381304,-0.161243610930449,
5.82287787425445));
#51602=CARTESIAN_POINT('Ctrl Pts',(-21.9385947161848,-4.98570788329408,
3.01241151630967));
#51603=CARTESIAN_POINT('Ctrl Pts',(-21.6999570510655,-5.22966502916022,
-2.56564025607911));
#51604=CARTESIAN_POINT('Ctrl Pts',(-21.4613193859463,-0.668984900732974,
-5.78656767379734));
#51605=CARTESIAN_POINT('Ctrl Pts',(-21.2226817208271,4.50631007820199,-3.69121602185732));
#51606=CARTESIAN_POINT('Ctrl Pts',(-20.9840440557079,5.54153389565618,1.79535743632542));
#51607=CARTESIAN_POINT('Ctrl Pts',(-20.7454063905886,1.4855979230446,5.63248657805113));
#51608=CARTESIAN_POINT('Ctrl Pts',(-20.5067687254694,-3.93519777116089,
4.29489519578073));
#51609=CARTESIAN_POINT('Ctrl Pts',(-20.2681310603502,-5.74061890739093,
-0.988534673640199));
#51610=CARTESIAN_POINT('Ctrl Pts',(-20.0294933952309,-2.27197537096228,
-5.36377051658862));
#51611=CARTESIAN_POINT('Ctrl Pts',(-19.7908557301117,3.28399450334934,-4.81116268098024));
#51612=CARTESIAN_POINT('Ctrl Pts',(-19.5522180649925,5.82286819435154,0.161592797159601));
#51613=CARTESIAN_POINT('Ctrl Pts',(-19.3135803998733,3.01211252782197,4.98588852268307));
#51614=CARTESIAN_POINT('Ctrl Pts',(-19.074942734754,-2.56595386414308,5.22951116338557));
#51615=CARTESIAN_POINT('Ctrl Pts',(-18.8363050696348,-5.78660778110002,
0.668637890488963));
#51616=CARTESIAN_POINT('Ctrl Pts',(-18.5976674045156,-3.69094578070135,
-4.50653142503277));
#51617=CARTESIAN_POINT('Ctrl Pts',(-18.3590297393963,1.79568974794104,-5.54142622165309));
#51618=CARTESIAN_POINT('Ctrl Pts',(-18.1203920742771,5.63257565629784,-1.48526015127511));
#51619=CARTESIAN_POINT('Ctrl Pts',(-17.8817544091579,4.29465920201836,3.93545532046853));
#51620=CARTESIAN_POINT('Ctrl Pts',(-17.6431167440387,-0.988878925442489,
5.74055961659669));
#51621=CARTESIAN_POINT('Ctrl Pts',(-17.4044790789195,-5.36390675282074,
2.2716537121509));
#51622=CARTESIAN_POINT('Ctrl Pts',(-17.1658414138002,-4.81096573766385,
-3.28428301336982));
#51623=CARTESIAN_POINT('Ctrl Pts',(-16.927203748681,0.161941982776275,-5.82285849348062));
#51624=CARTESIAN_POINT('Ctrl Pts',(-16.6885660835618,4.98606914415835,-3.01181352851682));
#51625=CARTESIAN_POINT('Ctrl Pts',(-16.4499284184425,5.22935727879621,2.56626746298708));
#51626=CARTESIAN_POINT('Ctrl Pts',(-16.2112907533233,0.668290877844823,
5.78664786758917));
#51627=CARTESIAN_POINT('Ctrl Pts',(-15.9726530882041,-4.50675275565964,
3.69067552627418));
#51628=CARTESIAN_POINT('Ctrl Pts',(-15.7340154230849,-5.5413185277209,-1.79602205310015));
#51629=CARTESIAN_POINT('Ctrl Pts',(-15.4953777579656,-1.48492237416498,
-5.63266471428835));
#51630=CARTESIAN_POINT('Ctrl Pts',(-15.2567400928464,3.93571285562398,-4.29442319281195));
#51631=CARTESIAN_POINT('Ctrl Pts',(-15.0181024277272,5.74050030515826,0.989223173688781));
#51632=CARTESIAN_POINT('Ctrl Pts',(-14.779464762608,2.2713320451704,5.36404296976328));
#51633=CARTESIAN_POINT('Ctrl Pts',(-14.5408270974887,-3.28457151157951,
4.81076877704648));
#51634=CARTESIAN_POINT('Ctrl Pts',(-14.3021894323695,-5.82284877166972,
-0.16229116781057));
#51635=CARTESIAN_POINT('Ctrl Pts',(-14.0635517672503,-3.01151451838073,
-4.98624974770287));
#51636=CARTESIAN_POINT('Ctrl Pts',(-13.824914102131,2.56658105260234,-5.22920337540123));
#51637=CARTESIAN_POINT('Ctrl Pts',(-13.5862764370118,5.78668793326858,-0.667943862797434));
#51638=CARTESIAN_POINT('Ctrl Pts',(-13.3476387718926,3.69040525857474,4.50697407007948));
#51639=CARTESIAN_POINT('Ctrl Pts',(-13.1090011067734,-1.79635435180044,
5.54121081386123));
#51640=CARTESIAN_POINT('Ctrl Pts',(-12.8703634416541,-5.63275375202288,
1.48458459171485));
#51641=CARTESIAN_POINT('Ctrl Pts',(-12.6317257765349,-4.29418716816209,
-3.93597037662593));
#51642=CARTESIAN_POINT('Ctrl Pts',(-12.3930881114157,0.989567418377627,
-5.74044097307606));
#51643=CARTESIAN_POINT('Ctrl Pts',(-12.1544504462965,5.36417916741587,-2.27101037002181));
#51644=CARTESIAN_POINT('Ctrl Pts',(-11.9158127811772,4.81057179912879,3.28485999797732));
#51645=CARTESIAN_POINT('Ctrl Pts',(-11.677175116058,-0.162640352261234,
5.82283902891891));
#51646=CARTESIAN_POINT('Ctrl Pts',(-11.4385374509388,-4.98643033331604,
3.01121549741473));
#51647=CARTESIAN_POINT('Ctrl Pts',(-11.1998997858196,-5.22904945320118,
-2.56689463298775));
#51648=CARTESIAN_POINT('Ctrl Pts',(-10.9612621207004,-0.667596845348008,
-5.78672797813811));
#51649=CARTESIAN_POINT('Ctrl Pts',(-10.7226244555811,4.50719536829151,-3.69013497760401));
#51650=CARTESIAN_POINT('Ctrl Pts',(-10.4839867904619,5.54110308007444,1.79668664404075));
#51651=CARTESIAN_POINT('Ctrl Pts',(-10.2453491253427,1.48424680392591,5.63284276950108));
#51652=CARTESIAN_POINT('Ctrl Pts',(-10.0067114602234,-3.93622788347351,
4.29395112806967));
#51653=CARTESIAN_POINT('Ctrl Pts',(-9.7680737951042,-5.74038162035028,-0.989911659507881));
#51654=CARTESIAN_POINT('Ctrl Pts',(-9.52943612998498,-2.27068868670629,
-5.36431534577795));
#51655=CARTESIAN_POINT('Ctrl Pts',(-9.29079846486575,3.2851484725623,-4.81037480391155));
#51656=CARTESIAN_POINT('Ctrl Pts',(-9.05216079974653,5.82282926522816,0.162989536127165));
#51657=CARTESIAN_POINT('Ctrl Pts',(-8.81352313462729,3.01091646561997,4.98661090099698));
#51658=CARTESIAN_POINT('Ctrl Pts',(-8.57488546950808,-2.56720820414237,
5.22889551219701));
#51659=CARTESIAN_POINT('Ctrl Pts',(-8.33624780438884,-5.78676800219732,
0.667249825496974));
#51660=CARTESIAN_POINT('Ctrl Pts',(-8.09761013926962,-3.6898646833635,-4.50741665029341));
#51661=CARTESIAN_POINT('Ctrl Pts',(-7.85897247415039,1.79701892982099,-5.54099532636385));
#51662=CARTESIAN_POINT('Ctrl Pts',(-7.62033480903117,5.6329317667206,-1.48390901079377));
#51663=CARTESIAN_POINT('Ctrl Pts',(-7.38169714391194,4.29371507253944,3.93648537615507));
#51664=CARTESIAN_POINT('Ctrl Pts',(-7.14305947879271,-0.990255897085868,
5.74032224700168));
#51665=CARTESIAN_POINT('Ctrl Pts',(-6.90442181367349,-5.36445150483438,
2.27036699518559));
#51666=CARTESIAN_POINT('Ctrl Pts',(-6.66578414855427,-4.81017779142361,
-3.28543693525765));
#51667=CARTESIAN_POINT('Ctrl Pts',(-6.42714648343502,0.163338719461003,
-5.82281948074281));
#51668=CARTESIAN_POINT('Ctrl Pts',(-6.18850881831581,4.98679145064144,-3.0106174227187));
#51669=CARTESIAN_POINT('Ctrl Pts',(-5.94987115319658,5.2287415525881,2.56752176552981));
#51670=CARTESIAN_POINT('Ctrl Pts',(-5.71123348807735,0.666902802864079,
5.78680800647329));
#51671=CARTESIAN_POINT('Ctrl Pts',(-5.47259582295812,-4.50763791535213,
3.68959437388266));
#51672=CARTESIAN_POINT('Ctrl Pts',(-5.2339581578389,-5.54088755413527,-1.79735120535602));
#51673=CARTESIAN_POINT('Ctrl Pts',(-4.99532049271967,-1.48357120962223,
-5.63302075094351));
#51674=CARTESIAN_POINT('Ctrl Pts',(-4.75668282760044,3.93674284949249,-4.29347898763361));
#51675=CARTESIAN_POINT('Ctrl Pts',(-4.51804516248123,5.74026286296703,0.990600104358038));
#51676=CARTESIAN_POINT('Ctrl Pts',(-4.27940749736199,2.27004527638976,5.36458769593022));
#51677=CARTESIAN_POINT('Ctrl Pts',(-4.04076983224277,-3.28572534945949,
4.80998066311877));
#51678=CARTESIAN_POINT('Ctrl Pts',(-3.80213216712354,-5.82280974571438,
-0.16368771312168));
#51679=CARTESIAN_POINT('Ctrl Pts',(-3.56349450200431,-3.0103182338791,-4.98697234526281));
#51680=CARTESIAN_POINT('Ctrl Pts',(-3.32485683688509,2.56783505836581,-5.22858687764632));
#51681=CARTESIAN_POINT('Ctrl Pts',(-3.08621917176586,5.78684848764546,-0.666557114673928));
#51682=CARTESIAN_POINT('Ctrl Pts',(-2.84758150664664,3.68932309589099,4.50786172998432));
#51683=CARTESIAN_POINT('Ctrl Pts',(-2.60894384152741,-1.79768164104147,
5.54077483750139));
#51684=CARTESIAN_POINT('Ctrl Pts',(-2.37030617640819,-5.63311323370599,
1.48324285461269));
#51685=CARTESIAN_POINT('Ctrl Pts',(-2.13166851128895,-4.29323613370083,
-3.93701844882378));
#51686=CARTESIAN_POINT('Ctrl Pts',(-1.89303084616973,0.990931345983249,
-5.7401686421007));
#51687=CARTESIAN_POINT('Ctrl Pts',(-1.65439318105051,5.36474874573582,-2.26979037177858));
#51688=CARTESIAN_POINT('Ctrl Pts',(-1.41575551593128,4.80973576926203,3.28614200352924));
#51689=CARTESIAN_POINT('Ctrl Pts',(-1.17711785081205,-0.163945061774615,
5.82255383487542));
#51690=CARTESIAN_POINT('Ctrl Pts',(-0.938480185692826,-4.98732912999593,
3.0104915028476));
#51691=CARTESIAN_POINT('Ctrl Pts',(-0.699842520573593,-5.22809441916263,
-2.56905538786673));
#51692=CARTESIAN_POINT('Ctrl Pts',(-0.461204855454365,-0.666861035834833,
-5.78514584226827));
#51693=CARTESIAN_POINT('Ctrl Pts',(-0.222567190335147,4.50934465203849,
-3.6924177249843));
#51694=CARTESIAN_POINT('Ctrl Pts',(0.016070474784088,5.53813222627847,1.80465927151925));
#51695=CARTESIAN_POINT('Ctrl Pts',(0.214935195716776,2.16371145271264,4.98307551377353));
#51696=CARTESIAN_POINT('Ctrl Pts',(0.374026972462927,-1.23643196713973,
4.97495722373696));
#51697=CARTESIAN_POINT('Ctrl Pts',(0.453572860835998,-2.72416315711316,
4.18423143996577));
#51698=CARTESIAN_POINT('Ctrl Pts',(0.493345805022534,-3.32886324744157,
3.62964109518183));
#51699=CARTESIAN_POINT('',(0.,4.77615934004779,1.20163511869213));
#51700=CARTESIAN_POINT('Ctrl Pts',(1.27675647831893E-15,4.78202092340378,
1.20708649626074));
#51701=CARTESIAN_POINT('Ctrl Pts',(1.54554986213376E-15,4.74680432306751,
1.31141193121661));
#51702=CARTESIAN_POINT('Ctrl Pts',(-1.2200289887242E-15,4.70790283853999,
1.41429721113204));
#51703=CARTESIAN_POINT('Ctrl Pts',(-1.0547118733939E-15,4.66526667899838,
1.51554882908261));
#51704=CARTESIAN_POINT('Ctrl Pts',(-8.36120983837436E-16,4.60951044466766,
1.64795777485803));
#51705=CARTESIAN_POINT('Ctrl Pts',(1.7406482083505E-15,4.5473685300075,
1.77757428418243));
#51706=CARTESIAN_POINT('Ctrl Pts',(9.99200722162641E-16,4.47921304648044,
1.90412989878513));
#51707=CARTESIAN_POINT('Ctrl Pts',(5.41776053129587E-16,4.43716556493129,
1.98220644662206));
#51708=CARTESIAN_POINT('Ctrl Pts',(-6.14882986343895E-16,4.39282838373583,
2.05911740148693));
#51709=CARTESIAN_POINT('Ctrl Pts',(-5.55111512312578E-16,4.34628172346416,
2.13479307691151));
#51710=CARTESIAN_POINT('Ctrl Pts',(-5.12735502418862E-16,4.31328167171442,
2.18844464268728));
#51711=CARTESIAN_POINT('Ctrl Pts',(7.5446052363616E-15,4.27917094813153,
2.24147520753853));
#51712=CARTESIAN_POINT('Ctrl Pts',(7.32747196252603E-15,4.24397679643589,
2.29385817644388));
#51713=CARTESIAN_POINT('Ctrl Pts',(7.25033478916171E-15,4.23147398038747,
2.31246736554886));
#51714=CARTESIAN_POINT('Ctrl Pts',(1.1248375135418E-15,4.21883292816165,
2.33099695996549));
#51715=CARTESIAN_POINT('Ctrl Pts',(9.43689570931383E-16,4.20605981758978,
2.34943854375472));
#51716=CARTESIAN_POINT('Ctrl Pts',(-2.0749684309091E-16,4.12488731768033,
2.46663391680332));
#51717=CARTESIAN_POINT('Ctrl Pts',(1.20832359191774E-15,4.03848405238999,
2.58013740696103));
#51718=CARTESIAN_POINT('Ctrl Pts',(2.72004641033163E-15,3.94721695353052,
2.68968900864157));
#51719=CARTESIAN_POINT('Ctrl Pts',(4.18855970728122E-15,3.85855853902716,
2.79610930064906));
#51720=CARTESIAN_POINT('Ctrl Pts',(1.88596569557423E-15,3.7653095628778,
2.89880063696627));
#51721=CARTESIAN_POINT('Ctrl Pts',(-4.9960036108132E-16,3.66777702457831,
2.99748899318237));
#51722=CARTESIAN_POINT('Ctrl Pts',(-2.58697066065493E-15,3.58243605356626,
3.08384130487147));
#51723=CARTESIAN_POINT('Ctrl Pts',(-1.9993502333868E-15,3.49381479608703,
3.16712847527816));
#51724=CARTESIAN_POINT('Ctrl Pts',(-3.60822483003176E-15,3.40210641955682,
3.24714114973565));
#51725=CARTESIAN_POINT('Ctrl Pts',(-3.93090312754506E-15,3.38371325027676,
3.26318861150008));
#51726=CARTESIAN_POINT('Ctrl Pts',(-8.00198331154243E-15,3.36519389765555,
3.27910584403603));
#51727=CARTESIAN_POINT('Ctrl Pts',(-7.93809462606987E-15,3.34656787360052,
3.29487610387643));
#51728=CARTESIAN_POINT('Ctrl Pts',(-7.56940933970987E-15,3.23908184596226,
3.38588224560911));
#51729=CARTESIAN_POINT('Ctrl Pts',(9.69472795872832E-15,3.12792305846971,
3.4721065544235));
#51730=CARTESIAN_POINT('Ctrl Pts',(8.60422844084496E-15,3.01343370374636,
3.55329630674216));
#51731=CARTESIAN_POINT('Ctrl Pts',(7.5193745599244E-15,2.89953707311163,
3.63406573070746));
#51732=CARTESIAN_POINT('Ctrl Pts',(1.54891535256133E-14,2.78234353560187,
3.70985298607676));
#51733=CARTESIAN_POINT('Ctrl Pts',(1.29340982368831E-14,2.66216592270983,
3.78036399292217));
#51734=CARTESIAN_POINT('Ctrl Pts',(1.04428067996356E-14,2.54498745723108,
3.84911533006954));
#51735=CARTESIAN_POINT('Ctrl Pts',(9.06092894879522E-15,2.42497131537325,
3.91285066923259));
#51736=CARTESIAN_POINT('Ctrl Pts',(1.10467190950203E-14,2.30239503897639,
3.9712502394403));
#51737=CARTESIAN_POINT('Ctrl Pts',(1.25360617046891E-14,2.21046283167875,
4.01504991709609));
#51738=CARTESIAN_POINT('Ctrl Pts',(1.14694130650435E-14,2.11709024431302,
4.05584730347416));
#51739=CARTESIAN_POINT('Ctrl Pts',(1.04916075827077E-14,2.02239293435179,
4.09348836738669));
#51740=CARTESIAN_POINT('Ctrl Pts',(1.01019433215215E-14,1.98465520635888,
4.10848866921022));
#51741=CARTESIAN_POINT('Ctrl Pts',(1.58900622876451E-14,1.94670710034945,
4.12298752598548));
#51742=CARTESIAN_POINT('Ctrl Pts',(1.63757896132211E-14,1.90855596787325,
4.1369744095719));
#51743=CARTESIAN_POINT('Ctrl Pts',(1.66667902990066E-14,1.8856995109076,
4.14535399313934));
#51744=CARTESIAN_POINT('Ctrl Pts',(-3.74501732116749E-15,1.8627701834264,
4.15354980834729));
#51745=CARTESIAN_POINT('Ctrl Pts',(-4.38538094726937E-15,1.83976957424201,
4.16155951178909));
#51746=CARTESIAN_POINT('Ctrl Pts',(-4.90190327326717E-15,1.8212171023791,
4.16802020144052));
#51747=CARTESIAN_POINT('Ctrl Pts',(9.50430379515547E-15,1.80262497700585,
4.17435742449665));
#51748=CARTESIAN_POINT('Ctrl Pts',(9.38138455808257E-15,1.784001553863,
4.18056782352897));
#51749=CARTESIAN_POINT('Ctrl Pts',(8.54497039802425E-15,1.65727692396478,
4.22282699966724));
#51750=CARTESIAN_POINT('Ctrl Pts',(7.75693411885647E-15,1.52899676754921,
4.25925543233605));
#51751=CARTESIAN_POINT('Ctrl Pts',(7.66053886991358E-15,1.39943774817802,
4.28958765120325));
#51752=CARTESIAN_POINT('Ctrl Pts',(7.59729281300995E-15,1.31443255133079,
4.30948897685494));
#51753=CARTESIAN_POINT('Ctrl Pts',(1.2113674912629E-15,1.2288765362281,
4.32676501145738));
#51754=CARTESIAN_POINT('Ctrl Pts',(1.0547118733939E-15,1.14284625117365,
4.34132862407617));
#51755=CARTESIAN_POINT('Ctrl Pts',(8.68428161696615E-16,1.01006019941622,
4.36380727351629));
#51756=CARTESIAN_POINT('Ctrl Pts',(4.15203095003235E-15,0.876143569520156,
4.37982636972409));
#51757=CARTESIAN_POINT('Ctrl Pts',(4.94049245958195E-15,0.741565045486008,
4.38948206088079));
#51758=CARTESIAN_POINT('Ctrl Pts',(5.72761812915067E-15,0.607214529250332,
4.39912139301662));
#51759=CARTESIAN_POINT('Ctrl Pts',(1.10432148395374E-14,0.472203479324102,
4.40241856966672));
#51760=CARTESIAN_POINT('Ctrl Pts',(1.14075415780235E-14,0.337013667456073,
4.39942001130783));
#51761=CARTESIAN_POINT('Ctrl Pts',(1.15826238267446E-14,0.272046335208114,
4.39797901265212));
#51762=CARTESIAN_POINT('Ctrl Pts',(9.92588300807085E-15,0.207038030887552,
4.39508336506645));
#51763=CARTESIAN_POINT('Ctrl Pts',(1.02695629777827E-14,0.142044407157708,
4.39073446593813));
#51764=CARTESIAN_POINT('Ctrl Pts',(1.03617903745677E-14,0.124603202396043,
4.38956742776066));
#51765=CARTESIAN_POINT('Ctrl Pts',(4.4841957176862E-15,0.107164810159224,
4.38829579344102));
#51766=CARTESIAN_POINT('Ctrl Pts',(4.69069227904129E-15,0.0897419980454403,
4.38692068583962));
#51767=CARTESIAN_POINT('Ctrl Pts',(6.25118297356027E-15,-0.0419218708223804,
4.37652902313169));
#51768=CARTESIAN_POINT('Ctrl Pts',(-5.49571088697169E-16,-0.17288184694056,
4.36022055581769));
#51769=CARTESIAN_POINT('Ctrl Pts',(8.60422844084496E-16,-0.302702434116573,
4.33812072407467));
#51770=CARTESIAN_POINT('Ctrl Pts',(2.26456079903569E-15,-0.431983851255918,
4.31611267721224));
#51771=CARTESIAN_POINT('Ctrl Pts',(1.75511797657805E-14,-0.560136154997887,
4.28836093293126));
#51772=CARTESIAN_POINT('Ctrl Pts',(1.48214773787458E-14,-0.686713620784949,
4.25494071804226));
#51773=CARTESIAN_POINT('Ctrl Pts',(1.23397585715295E-14,-0.80179198203985,
4.22455660868837));
#51774=CARTESIAN_POINT('Ctrl Pts',(-2.35332166972068E-15,-0.915568901399882,
4.18948643033132));
#51775=CARTESIAN_POINT('Ctrl Pts',(-5.99520433297585E-15,-1.02768958167645,
4.14975498030284));
#51776=CARTESIAN_POINT('Ctrl Pts',(-8.67136215211543E-15,-1.11007901125274,
4.12055919326328));
#51777=CARTESIAN_POINT('Ctrl Pts',(6.0234625807556E-15,-1.19157368030025,
4.08884575090022));
#51778=CARTESIAN_POINT('Ctrl Pts',(4.84334794492725E-15,-1.27206424811892,
4.05464924064616));
#51779=CARTESIAN_POINT('Ctrl Pts',(4.19130181297638E-15,-1.31653752369003,
4.03575471840195));
#51780=CARTESIAN_POINT('Ctrl Pts',(7.59797375755575E-15,-1.36070412856013,
4.01610202232593));
#51781=CARTESIAN_POINT('Ctrl Pts',(7.70217223333702E-15,-1.40454455699869,
3.99569611765175));
#51782=CARTESIAN_POINT('Ctrl Pts',(7.75609059491098E-15,-1.42723014864851,
3.98513691380336));
#51783=CARTESIAN_POINT('Ctrl Pts',(-7.46205461605755E-15,-1.44982838930905,
3.97437601887541));
#51784=CARTESIAN_POINT('Ctrl Pts',(-8.10462807976364E-15,-1.47233648956831,
3.96341406098191));
#51785=CARTESIAN_POINT('Ctrl Pts',(-8.59111957832261E-15,-1.48937734177172,
3.95511477751635));
#51786=CARTESIAN_POINT('Ctrl Pts',(5.51713801836789E-15,-1.50635977342605,
3.94670349607368));
#51787=CARTESIAN_POINT('Ctrl Pts',(5.68989300120393E-15,-1.52327621904144,
3.93818410740871));
#51788=CARTESIAN_POINT('Ctrl Pts',(6.8760654734775E-15,-1.63942813424693,
3.87968817201454));
#51789=CARTESIAN_POINT('Ctrl Pts',(4.1445617132442E-15,-1.75256979369442,
3.81605162100472));
#51790=CARTESIAN_POINT('Ctrl Pts',(4.69069227904129E-15,-1.8623899266764,
3.74745962400277));
#51791=CARTESIAN_POINT('Ctrl Pts',(5.22545435247209E-15,-1.96992399580907,
3.68029546796622));
#51792=CARTESIAN_POINT('Ctrl Pts',(5.0249819177936E-15,-2.07427385910768,
3.60837941731036));
#51793=CARTESIAN_POINT('Ctrl Pts',(6.27276008913213E-15,-2.17511326369545,
3.53184659443599));
#51794=CARTESIAN_POINT('Ctrl Pts',(7.56032798375268E-15,-2.27916828152011,
3.45287325776349));
#51795=CARTESIAN_POINT('Ctrl Pts',(-5.02292661063484E-15,-2.37948625932775,
3.36898369722969));
#51796=CARTESIAN_POINT('Ctrl Pts',(-4.60395610524245E-15,-2.47566144275777,
3.28029126749575));
#51797=CARTESIAN_POINT('Ctrl Pts',(-4.21077948966132E-15,-2.56591560775799,
3.19705918098456));
#51798=CARTESIAN_POINT('Ctrl Pts',(5.23948052523968E-15,-2.65252139743486,
3.10959674386589));
#51799=CARTESIAN_POINT('Ctrl Pts',(5.31345800691696E-15,-2.73509733308257,
3.0179750570285));
#51800=CARTESIAN_POINT('Ctrl Pts',(5.31831121266542E-15,-2.74051463029901,
3.01196432393565));
#51801=CARTESIAN_POINT('Ctrl Pts',(2.3894388675905E-18,-2.74591456605251,
3.00593568341939));
#51802=CARTESIAN_POINT('Ctrl Pts',(-1.38777878078145E-17,-2.75129702511903,
2.99988915288068));
#51803=CARTESIAN_POINT('Ctrl Pts',(-0.808841525903593,-4.91703434725887,
-0.0013692803956027));
#51804=CARTESIAN_POINT('Ctrl Pts',(-0.772508524126926,-4.91859034973346,
-0.753815327274128));
#51805=CARTESIAN_POINT('Ctrl Pts',(-0.73617552235026,-4.75666071795644,
-1.50557039925234));
#51806=CARTESIAN_POINT('Ctrl Pts',(-0.699842520573593,-4.42776130708021,
-2.1751459818146));
#51807=CARTESIAN_POINT('Ctrl Pts',(-0.620296632200516,-3.70768329138669,
-3.64108553933391));
#51808=CARTESIAN_POINT('Ctrl Pts',(-0.540750743827439,-2.18727216361073,
-4.71311569080111));
#51809=CARTESIAN_POINT('Ctrl Pts',(-0.461204855454364,-0.564365651743867,
-4.90034274698736));
#51810=CARTESIAN_POINT('Ctrl Pts',(-0.381658967081291,1.05854086012297,
-5.08756980317361));
#51811=CARTESIAN_POINT('Ctrl Pts',(-0.302113078708221,2.78394275608069,
-4.38999376407897));
#51812=CARTESIAN_POINT('Ctrl Pts',(-0.222567190335146,3.81810829976624,
-3.12502624511441));
#51813=CARTESIAN_POINT('Ctrl Pts',(-0.148378126890099,4.78263047309757,
-1.94524489575994));
#51814=CARTESIAN_POINT('Ctrl Pts',(-0.0741890634450472,5.14588079318518,
-0.271918139693744));
#51815=CARTESIAN_POINT('Ctrl Pts',(1.31838984174237E-15,4.78202092340378,
1.20708649626074));
#51816=CARTESIAN_POINT('',(-29.575,-2.36230756092323,-3.31488661006752));
#51817=CARTESIAN_POINT('Ctrl Pts',(-29.575,-2.36826780557339,-3.31775809990771));
#51818=CARTESIAN_POINT('Ctrl Pts',(-29.575,-2.44830306796112,-3.27276844726465));
#51819=CARTESIAN_POINT('Ctrl Pts',(-29.575,-2.52655779909889,-3.22498344987375));
#51820=CARTESIAN_POINT('Ctrl Pts',(-29.575,-2.60286326628888,-3.1744359090982));
#51821=CARTESIAN_POINT('Ctrl Pts',(-29.575,-2.70499541343267,-3.106779828055));
#51822=CARTESIAN_POINT('Ctrl Pts',(-29.575,-2.80363682654566,-3.03417684171155));
#51823=CARTESIAN_POINT('Ctrl Pts',(-29.575,-2.89869614562238,-2.9570330604008));
#51824=CARTESIAN_POINT('Ctrl Pts',(-29.575,-2.96224887403662,-2.90545791942454));
#51825=CARTESIAN_POINT('Ctrl Pts',(-29.575,-3.02420016779924,-2.85185208063885));
#51826=CARTESIAN_POINT('Ctrl Pts',(-29.575,-3.08451737823507,-2.79632528183713));
#51827=CARTESIAN_POINT('Ctrl Pts',(-29.575,-3.11868159705198,-2.76487439591655));
#51828=CARTESIAN_POINT('Ctrl Pts',(-29.575,-3.15232148638354,-2.73280706845916));
#51829=CARTESIAN_POINT('Ctrl Pts',(-29.575,-3.18543039276807,-2.70014206823866));
#51830=CARTESIAN_POINT('Ctrl Pts',(-29.575,-3.20694675023592,-2.67891419035985));
#51831=CARTESIAN_POINT('Ctrl Pts',(-29.575,-3.22824271002023,-2.65742973362904));
#51832=CARTESIAN_POINT('Ctrl Pts',(-29.575,-3.24929376278556,-2.63571743596404));
#51833=CARTESIAN_POINT('Ctrl Pts',(-29.575,-3.33714135858251,-2.54511041643103));
#51834=CARTESIAN_POINT('Ctrl Pts',(-29.575,-3.42079165100367,-2.45047748262222));
#51835=CARTESIAN_POINT('Ctrl Pts',(-29.575,-3.50014704916176,-2.35224076529156));
#51836=CARTESIAN_POINT('Ctrl Pts',(-29.575,-3.58105807397336,-2.25207828538672));
#51837=CARTESIAN_POINT('Ctrl Pts',(-29.575,-3.65750467553342,-2.14816887047587));
#51838=CARTESIAN_POINT('Ctrl Pts',(-29.575,-3.72935582339607,-2.04091404902635));
#51839=CARTESIAN_POINT('Ctrl Pts',(-29.575,-3.76079070058598,-1.99399006464218));
#51840=CARTESIAN_POINT('Ctrl Pts',(-29.575,-3.79134558154171,-1.94642520728123));
#51841=CARTESIAN_POINT('Ctrl Pts',(-29.575,-3.82100749080666,-1.89825079032625));
#51842=CARTESIAN_POINT('Ctrl Pts',(-29.575,-3.83626358617193,-1.87347310347317));
#51843=CARTESIAN_POINT('Ctrl Pts',(-29.575,-3.85128343521349,-1.84853414389017));
#51844=CARTESIAN_POINT('Ctrl Pts',(-29.575,-3.86606513313638,-1.82343804723132));
#51845=CARTESIAN_POINT('Ctrl Pts',(-29.575,-3.87962032072916,-1.80042429740151));
#51846=CARTESIAN_POINT('Ctrl Pts',(-29.575,-3.8929775187076,-1.77727417891757));
#51847=CARTESIAN_POINT('Ctrl Pts',(-29.575,-3.90612065588015,-1.75401710046083));
#51848=CARTESIAN_POINT('Ctrl Pts',(-29.575,-3.97117453777595,-1.63890278526318));
#51849=CARTESIAN_POINT('Ctrl Pts',(-29.575,-4.03105238509688,-1.52106386401277));
#51850=CARTESIAN_POINT('Ctrl Pts',(-29.575,-4.08564840782879,-1.40094223444012));
#51851=CARTESIAN_POINT('Ctrl Pts',(-29.575,-4.14101887615531,-1.27911667732505));
#51852=CARTESIAN_POINT('Ctrl Pts',(-29.575,-4.19095714201348,-1.1549425736421));
#51853=CARTESIAN_POINT('Ctrl Pts',(-29.575,-4.23531866325731,-1.0288395166209));
#51854=CARTESIAN_POINT('Ctrl Pts',(-29.575,-4.27963521656908,-0.902864286453708));
#51855=CARTESIAN_POINT('Ctrl Pts',(-29.575,-4.31838678906507,-0.774963270506112));
#51856=CARTESIAN_POINT('Ctrl Pts',(-29.575,-4.35138804153719,-0.645524185385383));
#51857=CARTESIAN_POINT('Ctrl Pts',(-29.575,-4.37561871456528,-0.550485484921972));
#51858=CARTESIAN_POINT('Ctrl Pts',(-29.575,-4.39674856572066,-0.45461692513887));
#51859=CARTESIAN_POINT('Ctrl Pts',(-29.575,-4.41468782191536,-0.358064990641669));
#51860=CARTESIAN_POINT('Ctrl Pts',(-29.575,-4.42224607172046,-0.317385286189321));
#51861=CARTESIAN_POINT('Ctrl Pts',(-29.575,-4.42923776471172,-0.27658421805809));
#51862=CARTESIAN_POINT('Ctrl Pts',(-29.575,-4.43565536938885,-0.235672547990024));
#51863=CARTESIAN_POINT('Ctrl Pts',(-29.575,-4.43961660695444,-0.210420004011757));
#51864=CARTESIAN_POINT('Ctrl Pts',(-29.575,-4.44335980044231,-0.185119699039305));
#51865=CARTESIAN_POINT('Ctrl Pts',(-29.575,-4.44687885001345,-0.159806585076518));
#51866=CARTESIAN_POINT('Ctrl Pts',(-29.575,-4.46586121538066,-0.0232632462829367));
#51867=CARTESIAN_POINT('Ctrl Pts',(-29.575,-4.47835132040759,0.113799339019299));
#51868=CARTESIAN_POINT('Ctrl Pts',(-29.575,-4.48420367058679,0.25094774090325));
#51869=CARTESIAN_POINT('Ctrl Pts',(-29.575,-4.48802427633214,0.340482706542299));
#51870=CARTESIAN_POINT('Ctrl Pts',(-29.575,-4.4890151135886,0.430054946692756));
#51871=CARTESIAN_POINT('Ctrl Pts',(-29.575,-4.48712517877637,0.519549617577561));
#51872=CARTESIAN_POINT('Ctrl Pts',(-29.575,-4.48432359350001,0.652213956389896));
#51873=CARTESIAN_POINT('Ctrl Pts',(-29.575,-4.47519448741699,0.784707646574493));
#51874=CARTESIAN_POINT('Ctrl Pts',(-29.575,-4.45999947400341,0.916663774321655));
#51875=CARTESIAN_POINT('Ctrl Pts',(-29.575,-4.44456005012953,1.05074240482977));
#51876=CARTESIAN_POINT('Ctrl Pts',(-29.575,-4.42285792068252,1.1842667673282));
#51877=CARTESIAN_POINT('Ctrl Pts',(-29.575,-4.39511381888785,1.31685585528468));
#51878=CARTESIAN_POINT('Ctrl Pts',(-29.575,-4.38178896280792,1.38053535472801));
#51879=CARTESIAN_POINT('Ctrl Pts',(-29.575,-4.36706965006509,1.44399910643623));
#51880=CARTESIAN_POINT('Ctrl Pts',(-29.575,-4.35097613979996,1.50720443522242));
#51881=CARTESIAN_POINT('Ctrl Pts',(-29.575,-4.34482928679442,1.53134546218391));
#51882=CARTESIAN_POINT('Ctrl Pts',(-29.575,-4.33848058918165,1.55545340805442));
#51883=CARTESIAN_POINT('Ctrl Pts',(-29.575,-4.3319391871451,1.57949701586949));
#51884=CARTESIAN_POINT('Ctrl Pts',(-29.575,-4.29596876934752,1.71171005118469));
#51885=CARTESIAN_POINT('Ctrl Pts',(-29.575,-4.25413965605729,1.84212793058693));
#51886=CARTESIAN_POINT('Ctrl Pts',(-29.575,-4.20675605414909,1.97036806915586));
#51887=CARTESIAN_POINT('Ctrl Pts',(-29.575,-4.15824257123346,2.10166614530495));
#51888=CARTESIAN_POINT('Ctrl Pts',(-29.575,-4.10390647699439,2.23068214498256));
#51889=CARTESIAN_POINT('Ctrl Pts',(-29.575,-4.04401911667263,2.35700945357488));
#51890=CARTESIAN_POINT('Ctrl Pts',(-29.575,-3.98492825956341,2.48165660617797));
#51891=CARTESIAN_POINT('Ctrl Pts',(-29.575,-3.92043243319514,2.60368687307991));
#51892=CARTESIAN_POINT('Ctrl Pts',(-29.575,-3.85074314886284,2.72270204804338));
#51893=CARTESIAN_POINT('Ctrl Pts',(-29.575,-3.79985133012436,2.80961496111749));
#51894=CARTESIAN_POINT('Ctrl Pts',(-29.575,-3.74618885745191,2.89491983557514));
#51895=CARTESIAN_POINT('Ctrl Pts',(-29.575,-3.68984439893471,2.97851803505928));
#51896=CARTESIAN_POINT('Ctrl Pts',(-29.575,-3.66391228552828,3.01699347783834));
#51897=CARTESIAN_POINT('Ctrl Pts',(-29.575,-3.63741189415848,3.05510731852617));
#51898=CARTESIAN_POINT('Ctrl Pts',(-29.575,-3.61035102303907,3.09284943609328));
#51899=CARTESIAN_POINT('Ctrl Pts',(-29.575,-3.59584650743156,3.11307905586041));
#51900=CARTESIAN_POINT('Ctrl Pts',(-29.575,-3.58118096187307,3.13320187682416));
#51901=CARTESIAN_POINT('Ctrl Pts',(-29.575,-3.56635552732019,3.15321629747535));
#51902=CARTESIAN_POINT('Ctrl Pts',(-29.575,-3.5546900145129,3.16896480586503));
#51903=CARTESIAN_POINT('Ctrl Pts',(-29.575,-3.54292488679082,3.18464691960963));
#51904=CARTESIAN_POINT('Ctrl Pts',(-29.575,-3.53107100158975,3.20024854439494));
#51905=CARTESIAN_POINT('Ctrl Pts',(-29.575,-3.444915061959,3.31364365665938));
#51906=CARTESIAN_POINT('Ctrl Pts',(-29.575,-3.353952606715,3.42295435898676));
#51907=CARTESIAN_POINT('Ctrl Pts',(-29.575,-3.25851212336527,3.52794677560707));
#51908=CARTESIAN_POINT('Ctrl Pts',(-29.575,-3.1617890061929,3.63435019539871));
#51909=CARTESIAN_POINT('Ctrl Pts',(-29.575,-3.06046638882771,3.73631912635592));
#51910=CARTESIAN_POINT('Ctrl Pts',(-29.575,-2.95483635071748,3.83359158033952));
#51911=CARTESIAN_POINT('Ctrl Pts',(-29.575,-2.84930340889874,3.93077462041477));
#51912=CARTESIAN_POINT('Ctrl Pts',(-29.575,-2.73947053698142,4.02327043490703));
#51913=CARTESIAN_POINT('Ctrl Pts',(-29.575,-2.62558525501093,4.11078989098106));
#51914=CARTESIAN_POINT('Ctrl Pts',(-29.575,-2.51319651570498,4.19715927219268));
#51915=CARTESIAN_POINT('Ctrl Pts',(-29.575,-2.39686069001292,4.27868275896332));
#51916=CARTESIAN_POINT('Ctrl Pts',(-29.575,-2.27677987968084,4.3550468235479));
#51917=CARTESIAN_POINT('Ctrl Pts',(-29.575,-2.24098328939054,4.37781126963447));
#51918=CARTESIAN_POINT('Ctrl Pts',(-29.575,-2.20485367910692,4.40011694506889));
#51919=CARTESIAN_POINT('Ctrl Pts',(-29.575,-2.16839587231048,4.42195480991686));
#51920=CARTESIAN_POINT('Ctrl Pts',(-29.575,-2.36826780557337,-3.31775809990772));
#51921=CARTESIAN_POINT('Ctrl Pts',(-29.5008109365549,-1.33928601121754,
-4.04293436335451));
#51922=CARTESIAN_POINT('Ctrl Pts',(-29.3470759847368,1.55637121596689,-4.50701225231274));
#51923=CARTESIAN_POINT('Ctrl Pts',(-29.1137951445456,4.65387018191312,-1.22765401651987));
#51924=CARTESIAN_POINT('Ctrl Pts',(-28.8751574794264,3.55090078994383,3.25125842872222));
#51925=CARTESIAN_POINT('Ctrl Pts',(-28.6365198143072,-0.816478135197904,
4.74503193420896));
#51926=CARTESIAN_POINT('Ctrl Pts',(-28.4455297648071,-3.71062116286106,
2.45079400531014));
#51927=CARTESIAN_POINT('Ctrl Pts',(-28.3340856036801,-4.06733760858173,
0.547694664417248));
#51928=CARTESIAN_POINT('Ctrl Pts',(-28.3021873309261,-4.06480101368718,
0.00206955444756761));
#51929=CARTESIAN_POINT('Origin',(-29.575,-4.52129938221115E-16,0.));
#51930=CARTESIAN_POINT('',(-29.575,-4.925,-6.03138548580071E-16));
#51931=CARTESIAN_POINT('Origin',(-29.575,0.,0.));
#51932=CARTESIAN_POINT('Origin',(-29.575,0.,0.));
#51933=CARTESIAN_POINT('',(-29.575,2.36230756092324,-3.31488661006752));
#51934=CARTESIAN_POINT('Ctrl Pts',(-29.575,2.17494790042119,4.42655504786424));
#51935=CARTESIAN_POINT('Ctrl Pts',(-29.575,2.26967152441801,4.37041752782518));
#51936=CARTESIAN_POINT('Ctrl Pts',(-29.575,2.36222031470781,4.31097507135364));
#51937=CARTESIAN_POINT('Ctrl Pts',(-29.575,2.45239463893034,4.24821920794634));
#51938=CARTESIAN_POINT('Ctrl Pts',(-29.575,2.57031754301399,4.16615201503894));
#51939=CARTESIAN_POINT('Ctrl Pts',(-29.575,2.68418134028915,4.07841926504524));
#51940=CARTESIAN_POINT('Ctrl Pts',(-29.575,2.793800816624,3.98544075385194));
#51941=CARTESIAN_POINT('Ctrl Pts',(-29.575,2.86142888819741,3.928079073063));
#51942=CARTESIAN_POINT('Ctrl Pts',(-29.575,2.92744077307288,3.8687200679563));
#51943=CARTESIAN_POINT('Ctrl Pts',(-29.575,2.99178498903163,3.80745669486626));
#51944=CARTESIAN_POINT('Ctrl Pts',(-29.575,3.03740293232873,3.76402296833516));
#51945=CARTESIAN_POINT('Ctrl Pts',(-29.575,3.08218251964483,3.71963195357705));
#51946=CARTESIAN_POINT('Ctrl Pts',(-29.575,3.12610340234575,3.67431582845979));
#51947=CARTESIAN_POINT('Ctrl Pts',(-29.575,3.14170642099533,3.65821714596868));
#51948=CARTESIAN_POINT('Ctrl Pts',(-29.575,3.15720284290207,3.64199979656664));
#51949=CARTESIAN_POINT('Ctrl Pts',(-29.575,3.17258572052557,3.62567157287578));
#51950=CARTESIAN_POINT('Ctrl Pts',(-29.575,3.27034309847291,3.52190657040855));
#51951=CARTESIAN_POINT('Ctrl Pts',(-29.575,3.36340172212969,3.41379269192058));
#51952=CARTESIAN_POINT('Ctrl Pts',(-29.575,3.45158356813246,3.30174290977256));
#51953=CARTESIAN_POINT('Ctrl Pts',(-29.575,3.53724490642985,3.19289585417305));
#51954=CARTESIAN_POINT('Ctrl Pts',(-29.575,3.61830434560196,3.08033384565738));
#51955=CARTESIAN_POINT('Ctrl Pts',(-29.575,3.69455768842054,2.96441414844495));
#51956=CARTESIAN_POINT('Ctrl Pts',(-29.575,3.76127936338681,2.86298441338408));
#51957=CARTESIAN_POINT('Ctrl Pts',(-29.575,3.82432087679273,2.75898335344391));
#51958=CARTESIAN_POINT('Ctrl Pts',(-29.575,3.88351761773973,2.65264344251299));
#51959=CARTESIAN_POINT('Ctrl Pts',(-29.575,3.89539020296671,2.63131575393826));
#51960=CARTESIAN_POINT('Ctrl Pts',(-29.575,3.90710917047629,2.60989171569305));
#51961=CARTESIAN_POINT('Ctrl Pts',(-29.575,3.91866219954629,2.58839389445723));
#51962=CARTESIAN_POINT('Ctrl Pts',(-29.575,3.98533187012549,2.46433529032153));
#51963=CARTESIAN_POINT('Ctrl Pts',(-29.575,4.04656060379988,2.33767837925172));
#51964=CARTESIAN_POINT('Ctrl Pts',(-29.575,4.10217235556336,2.20881042226382));
#51965=CARTESIAN_POINT('Ctrl Pts',(-29.575,4.15749625211679,2.08060950617376));
#51966=CARTESIAN_POINT('Ctrl Pts',(-29.575,4.20726139736363,1.95021957273537));
#51967=CARTESIAN_POINT('Ctrl Pts',(-29.575,4.25124518841383,1.81800776290176));
#51968=CARTESIAN_POINT('Ctrl Pts',(-29.575,4.29413119192342,1.68909581590603));
#51969=CARTESIAN_POINT('Ctrl Pts',(-29.575,4.33152087503006,1.55845109390724));
#51970=CARTESIAN_POINT('Ctrl Pts',(-29.575,4.36315916984956,1.42641155759016));
#51971=CARTESIAN_POINT('Ctrl Pts',(-29.575,4.38688789096419,1.32738190535235));
#51972=CARTESIAN_POINT('Ctrl Pts',(-29.575,4.40738049178401,1.22756756386048));
#51973=CARTESIAN_POINT('Ctrl Pts',(-29.575,4.42451035861733,1.12711368795651));
#51974=CARTESIAN_POINT('Ctrl Pts',(-29.575,4.43133674032546,1.08708205737504));
#51975=CARTESIAN_POINT('Ctrl Pts',(-29.575,4.4376289049131,1.04694890359475));
#51976=CARTESIAN_POINT('Ctrl Pts',(-29.575,4.44337808320161,1.00672360633312));
#51977=CARTESIAN_POINT('Ctrl Pts',(-29.575,4.44682246179442,0.982624309733816));
#51978=CARTESIAN_POINT('Ctrl Pts',(-29.575,4.45007193773189,0.958491942467769));
#51979=CARTESIAN_POINT('Ctrl Pts',(-29.575,4.45312454919313,0.934328545878378));
#51980=CARTESIAN_POINT('Ctrl Pts',(-29.575,4.45558677843594,0.914838406879834));
#51981=CARTESIAN_POINT('Ctrl Pts',(-29.575,4.45791999829306,0.895335151707175));
#51982=CARTESIAN_POINT('Ctrl Pts',(-29.575,4.46012266207708,0.87582765091181));
#51983=CARTESIAN_POINT('Ctrl Pts',(-29.575,4.47511104469547,0.743085700928035));
#51984=CARTESIAN_POINT('Ctrl Pts',(-29.575,4.48407271847718,0.610034498076699));
#51985=CARTESIAN_POINT('Ctrl Pts',(-29.575,4.48680554393477,0.476999857930275));
#51986=CARTESIAN_POINT('Ctrl Pts',(-29.575,4.48859856927288,0.389714927249725));
#51987=CARTESIAN_POINT('Ctrl Pts',(-29.575,4.48770920842808,0.302437045899035));
#51988=CARTESIAN_POINT('Ctrl Pts',(-29.575,4.48406815367479,0.215259203818982));
#51989=CARTESIAN_POINT('Ctrl Pts',(-29.575,4.47844824112982,0.0807015326092455));
#51990=CARTESIAN_POINT('Ctrl Pts',(-29.575,4.46627498023888,-0.0536189903864601));
#51991=CARTESIAN_POINT('Ctrl Pts',(-29.575,4.44773981895834,-0.187263918132325));
#51992=CARTESIAN_POINT('Ctrl Pts',(-29.575,4.42923611011045,-0.320682062953368));
#51993=CARTESIAN_POINT('Ctrl Pts',(-29.575,4.40439160268717,-0.453427703408474));
#51994=CARTESIAN_POINT('Ctrl Pts',(-29.575,4.37335182340664,-0.58503925570624));
#51995=CARTESIAN_POINT('Ctrl Pts',(-29.575,4.35843537009352,-0.648286405680295));
#51996=CARTESIAN_POINT('Ctrl Pts',(-29.575,4.34208757622849,-0.711271201901602));
#51997=CARTESIAN_POINT('Ctrl Pts',(-29.575,4.32432137404194,-0.773939500968908));
#51998=CARTESIAN_POINT('Ctrl Pts',(-29.575,4.31955371135246,-0.790756899990894));
#51999=CARTESIAN_POINT('Ctrl Pts',(-29.575,4.31468432223976,-0.807549803851364));
#52000=CARTESIAN_POINT('Ctrl Pts',(-29.575,4.30971696019155,-0.824305954558689));
#52001=CARTESIAN_POINT('Ctrl Pts',(-29.575,4.27217870230904,-0.950931857858156));
#52002=CARTESIAN_POINT('Ctrl Pts',(-29.575,4.22899927473913,-1.07563909243635));
#52003=CARTESIAN_POINT('Ctrl Pts',(-29.575,4.18039187949891,-1.19802776435577));
#52004=CARTESIAN_POINT('Ctrl Pts',(-29.575,4.13198650007613,-1.3199077801853));
#52005=CARTESIAN_POINT('Ctrl Pts',(-29.575,4.07819767353095,-1.43948920797592));
#52006=CARTESIAN_POINT('Ctrl Pts',(-29.575,4.01919161106764,-1.55635171305596));
#52007=CARTESIAN_POINT('Ctrl Pts',(-29.575,3.96554454554038,-1.66260063403094));
#52008=CARTESIAN_POINT('Ctrl Pts',(-29.575,3.90758410693226,-1.7666021746683));
#52009=CARTESIAN_POINT('Ctrl Pts',(-29.575,3.84540829196954,-1.86801442537029));
#52010=CARTESIAN_POINT('Ctrl Pts',(-29.575,3.79972079463418,-1.9425333027907));
#52011=CARTESIAN_POINT('Ctrl Pts',(-29.575,3.7517566228007,-2.01565352617642));
#52012=CARTESIAN_POINT('Ctrl Pts',(-29.575,3.70157235710967,-2.08727533440549));
#52013=CARTESIAN_POINT('Ctrl Pts',(-29.575,3.67384420437395,-2.12684830434812));
#52014=CARTESIAN_POINT('Ctrl Pts',(-29.575,3.64543819285622,-2.16596367436737));
#52015=CARTESIAN_POINT('Ctrl Pts',(-29.575,3.61636323740365,-2.20460339725076));
#52016=CARTESIAN_POINT('Ctrl Pts',(-29.575,3.60131842230507,-2.22459749447954));
#52017=CARTESIAN_POINT('Ctrl Pts',(-29.575,3.58609448820911,-2.24446422067884));
#52018=CARTESIAN_POINT('Ctrl Pts',(-29.575,3.57069262976354,-2.26420097811176));
#52019=CARTESIAN_POINT('Ctrl Pts',(-29.575,3.55903139036739,-2.27914430810939));
#52020=CARTESIAN_POINT('Ctrl Pts',(-29.575,3.54727273939743,-2.29400720550239));
#52021=CARTESIAN_POINT('Ctrl Pts',(-29.575,3.53542205698418,-2.30878307744774));
#52022=CARTESIAN_POINT('Ctrl Pts',(-29.575,3.45405476451608,-2.41023484639433));
#52023=CARTESIAN_POINT('Ctrl Pts',(-29.575,3.36828498238971,-2.50767334973966));
#52024=CARTESIAN_POINT('Ctrl Pts',(-29.575,3.27835860536771,-2.60083261446428));
#52025=CARTESIAN_POINT('Ctrl Pts',(-29.575,3.19030403000318,-2.69205278554481));
#52026=CARTESIAN_POINT('Ctrl Pts',(-29.575,3.09826340014138,-2.77917034507256));
#52027=CARTESIAN_POINT('Ctrl Pts',(-29.575,3.00243676957963,-2.86189425854725));
#52028=CARTESIAN_POINT('Ctrl Pts',(-29.575,2.90355461728311,-2.94725590136843));
#52029=CARTESIAN_POINT('Ctrl Pts',(-29.575,2.80064068610558,-3.02794003035809));
#52030=CARTESIAN_POINT('Ctrl Pts',(-29.575,2.69389027200841,-3.10357332294541));
#52031=CARTESIAN_POINT('Ctrl Pts',(-29.575,2.59371175266095,-3.17455038967486));
#52032=CARTESIAN_POINT('Ctrl Pts',(-29.575,2.49015393838355,-3.24107925145737));
#52033=CARTESIAN_POINT('Ctrl Pts',(-29.575,2.38336574054609,-3.30280154424992));
#52034=CARTESIAN_POINT('Ctrl Pts',(-29.575,2.37636023875519,-3.30685063995014));
#52035=CARTESIAN_POINT('Ctrl Pts',(-29.575,2.36934083188486,-3.31087903158254));
#52036=CARTESIAN_POINT('Ctrl Pts',(-29.575,2.36230756092332,-3.31488661006746));
#52037=CARTESIAN_POINT('Origin',(-29.575,0.,0.));
#52038=CARTESIAN_POINT('Origin',(-32.3478126690739,0.,0.));
#52039=CARTESIAN_POINT('Ctrl Pts',(-29.575,2.36230756092324,-3.31488661006752));
#52040=CARTESIAN_POINT('Ctrl Pts',(-29.5352270558135,2.91456939066647,-2.92132494432319));
#52041=CARTESIAN_POINT('Ctrl Pts',(-29.4556811674404,3.80947864266608,-1.85446537575054));
#52042=CARTESIAN_POINT('Ctrl Pts',(-29.2965893906943,4.40029930288375,0.892938679230673));
#52043=CARTESIAN_POINT('Ctrl Pts',(-29.0977246697615,2.41062119233501,4.16711865021482));
#52044=CARTESIAN_POINT('Ctrl Pts',(-28.8590870046423,-2.21020820766824,
4.28001845847083));
#52045=CARTESIAN_POINT('Ctrl Pts',(-28.6924496710798,-4.01269863755865,
1.60905902128973));
#52046=CARTESIAN_POINT('Ctrl Pts',(-28.6053582258903,-4.07619291884947,
0.130177206130288));
#52047=CARTESIAN_POINT('Ctrl Pts',(-28.5978126690739,-4.07533558288693,
0.00197868943318465));
#52048=CARTESIAN_POINT('Ctrl Pts',(-30.0683458050225,2.85821514250009,-4.01076441581692));
#52049=CARTESIAN_POINT('Ctrl Pts',(-30.028572860836,3.52641057585851,-3.5345842895939));
#52050=CARTESIAN_POINT('Ctrl Pts',(-29.9490269724629,4.60918371579173,-2.24376415073622));
#52051=CARTESIAN_POINT('Ctrl Pts',(-29.7899351957168,5.32403244483542,1.08038889453645));
#52052=CARTESIAN_POINT('Ctrl Pts',(-29.5910704747841,2.91667101639856,5.0419013271853));
#52053=CARTESIAN_POINT('Ctrl Pts',(-29.3524328096649,-2.6741863217702,5.17850163566369));
#52054=CARTESIAN_POINT('Ctrl Pts',(-29.1137951445457,-5.7973743179944,0.550511209599409));
#52055=CARTESIAN_POINT('Ctrl Pts',(-28.8751574794264,-3.59989778886694,
-4.57971187869854));
#52056=CARTESIAN_POINT('Ctrl Pts',(-28.6365198143073,1.9077811732274,-5.50426057988267));
#52057=CARTESIAN_POINT('Ctrl Pts',(-28.3978821491879,5.66123134949523,-1.37093968550409));
#52058=CARTESIAN_POINT('Ctrl Pts',(-28.1592444840688,4.21433244584917,4.02140449350459));
#52059=CARTESIAN_POINT('Ctrl Pts',(-27.9206068189495,-1.10479606405923,
5.71943238413845));
#52060=CARTESIAN_POINT('Ctrl Pts',(-27.6819691538303,-5.40870633854705,
2.16272545229035));
#52061=CARTESIAN_POINT('Ctrl Pts',(-27.4433314887111,-4.74359941984978,
-3.380866692594));
#52062=CARTESIAN_POINT('Ctrl Pts',(-27.2046938235918,0.279640350988314,
-5.8184000833979));
#52063=CARTESIAN_POINT('Ctrl Pts',(-26.9660561584726,5.04593690996907,-2.91039003941573));
#52064=CARTESIAN_POINT('Ctrl Pts',(-26.7274184933533,5.17640786355619,2.67146555315453));
#52065=CARTESIAN_POINT('Ctrl Pts',(-26.4887808282342,0.551162248122564,
5.79897734693768));
#52066=CARTESIAN_POINT('Ctrl Pts',(-26.2501431631149,-4.58044707277724,
3.59880626920218));
#52067=CARTESIAN_POINT('Ctrl Pts',(-26.0115054979957,-5.50387573699426,
-1.90768582721621));
#52068=CARTESIAN_POINT('Ctrl Pts',(-25.7728678328765,-1.37074105079164,
-5.66153515210527));
#52069=CARTESIAN_POINT('Ctrl Pts',(-25.5342301677573,4.02173058771444,-4.21397584735458));
#52070=CARTESIAN_POINT('Ctrl Pts',(-25.295592502638,5.71932789822544,1.10507891249598));
#52071=CARTESIAN_POINT('Ctrl Pts',(-25.0569548375188,2.16242101025971,5.40886734761332));
#52072=CARTESIAN_POINT('Ctrl Pts',(-24.8183171723995,-3.38116152304108,
4.74338034983671));
#52073=CARTESIAN_POINT('Ctrl Pts',(-24.5796795072803,-5.81837790032782,
-0.27998076825629));
#52074=CARTESIAN_POINT('Ctrl Pts',(-24.3410418421611,-2.91009025392015,
-5.04611585917912));
#52075=CARTESIAN_POINT('Ctrl Pts',(-24.1024041770419,2.67177743350171,-5.17624534512243));
#52076=CARTESIAN_POINT('Ctrl Pts',(-23.8637665119226,5.79900962484977,-0.550815695476877));
#52077=CARTESIAN_POINT('Ctrl Pts',(-23.6251288468035,3.59853198023136,4.58066350376895));
#52078=CARTESIAN_POINT('Ctrl Pts',(-23.3864911816842,-1.90801608760284,
5.50376100088902));
#52079=CARTESIAN_POINT('Ctrl Pts',(-23.147853516565,-5.66161723459444,1.37040170709392));
#52080=CARTESIAN_POINT('Ctrl Pts',(-22.9092158514458,-4.21373472077718,
-4.02198337277209));
#52081=CARTESIAN_POINT('Ctrl Pts',(-22.6705781863265,1.10542191660648,-5.71926157245085));
#52082=CARTESIAN_POINT('Ctrl Pts',(-22.4319405212073,5.40899699874395,-2.16209667128711));
#52083=CARTESIAN_POINT('Ctrl Pts',(-22.1933028560881,4.74317758767807,3.38144598062146));
#52084=CARTESIAN_POINT('Ctrl Pts',(-21.9546651909688,-0.280329688527433,
5.81836109345686));
#52085=CARTESIAN_POINT('Ctrl Pts',(-21.7160275258496,-5.04629036031444,
2.90978764647796));
#52086=CARTESIAN_POINT('Ctrl Pts',(-21.4773898607304,-5.17608511572218,
-2.67208783967747));
#52087=CARTESIAN_POINT('Ctrl Pts',(-21.2387521956112,-0.55046793874511,
-5.79904264483125));
#52088=CARTESIAN_POINT('Ctrl Pts',(-21.0001145304919,4.58087929208444,-3.59825728089574));
#52089=CARTESIAN_POINT('Ctrl Pts',(-20.7614768653727,5.50364657119464,1.90834613410097));
#52090=CARTESIAN_POINT('Ctrl Pts',(-20.5228392002535,1.37006218854147,5.66169940456846));
#52091=CARTESIAN_POINT('Ctrl Pts',(-20.2842015351343,-4.02223605484748,
4.21349352286768));
#52092=CARTESIAN_POINT('Ctrl Pts',(-20.045563870015,-5.71919527222015,-1.10576488747686));
#52093=CARTESIAN_POINT('Ctrl Pts',(-19.8069262048958,-2.16177230051888,
-5.40912664566764));
#52094=CARTESIAN_POINT('Ctrl Pts',(-19.5682885397766,3.38173041352887,-4.74297480052089));
#52095=CARTESIAN_POINT('Ctrl Pts',(-19.3296508746573,5.81834427218029,0.28067860365368));
#52096=CARTESIAN_POINT('Ctrl Pts',(-19.0910132095381,2.90948502517622,5.04646484545742));
#52097=CARTESIAN_POINT('Ctrl Pts',(-18.8523755444189,-2.67239823447518,
5.17592486658531));
#52098=CARTESIAN_POINT('Ctrl Pts',(-18.6137378792997,-5.79907564487983,
0.550120180618539));
#52099=CARTESIAN_POINT('Ctrl Pts',(-18.3751002141804,-3.59798256814023,
-4.58109506423096));
#52100=CARTESIAN_POINT('Ctrl Pts',(-18.1364625490612,1.90867617348636,-5.50353212154956));
#52101=CARTESIAN_POINT('Ctrl Pts',(-17.897824883942,5.66178155431231,-1.3697226651447));
#52102=CARTESIAN_POINT('Ctrl Pts',(-17.6591872188228,4.2132523097379,4.02248872250135));
#52103=CARTESIAN_POINT('Ctrl Pts',(-17.4205495537035,-1.10610785433544,
5.71912895139983));
#52104=CARTESIAN_POINT('Ctrl Pts',(-17.1819118885843,-5.40925627315763,
2.16144792198822));
#52105=CARTESIAN_POINT('Ctrl Pts',(-16.9432742234651,-4.74277199629759,
-3.38201483428115));
#52106=CARTESIAN_POINT('Ctrl Pts',(-16.7046365583458,0.281027517765593,
-5.81832742997681));
#52107=CARTESIAN_POINT('Ctrl Pts',(-16.4659988932266,5.04663931245511,-2.90918239341314));
#52108=CARTESIAN_POINT('Ctrl Pts',(-16.2273612281074,5.17576459883361,2.67270861966342));
#52109=CARTESIAN_POINT('Ctrl Pts',(-15.9887235629882,0.549772420514306,
5.79910862407352));
#52110=CARTESIAN_POINT('Ctrl Pts',(-15.750085897869,-4.5813108199035,3.597707842446));
#52111=CARTESIAN_POINT('Ctrl Pts',(-15.5114482327497,-5.50341765211267,
-1.90900620600798));
#52112=CARTESIAN_POINT('Ctrl Pts',(-15.2728105676305,-1.36938313682227,
-5.66186368369541));
#52113=CARTESIAN_POINT('Ctrl Pts',(-15.0341729025113,4.02274137568974,-4.21301108145661));
#52114=CARTESIAN_POINT('Ctrl Pts',(-14.7955352373921,5.71906261001256,1.10645081721627));
#52115=CARTESIAN_POINT('Ctrl Pts',(-14.5568975722728,2.16112353568466,5.40938588119503));
#52116=CARTESIAN_POINT('Ctrl Pts',(-14.3182599071536,-3.38229924287111,
4.74256917501852));
#52117=CARTESIAN_POINT('Ctrl Pts',(-14.0796222420344,-5.81831056684969,
-0.281376430866862));
#52118=CARTESIAN_POINT('Ctrl Pts',(-13.8409845769151,-2.90887975118817,
-5.04681376130423));
#52119=CARTESIAN_POINT('Ctrl Pts',(-13.6023469117959,2.67301899524012,-5.17560431246901));
#52120=CARTESIAN_POINT('Ctrl Pts',(-13.3637092466767,5.79914158241269,-0.549424658433007));
#52121=CARTESIAN_POINT('Ctrl Pts',(-13.1250715815575,3.5974331038138,4.5815265591009));
#52122=CARTESIAN_POINT('Ctrl Pts',(-12.8864339164382,-1.90933623166449,
5.50330316288458));
#52123=CARTESIAN_POINT('Ctrl Pts',(-12.647796251319,-5.66194579271754,1.3690436035753));
#52124=CARTESIAN_POINT('Ctrl Pts',(-12.4091585861998,-4.21276983802462,
-4.0229940144117));
#52125=CARTESIAN_POINT('Ctrl Pts',(-12.1705209210806,1.10679377611814,-5.7189962480586));
#52126=CARTESIAN_POINT('Ctrl Pts',(-11.9318832559613,5.4095154697794,-2.16079914160935));
#52127=CARTESIAN_POINT('Ctrl Pts',(-11.6932455908421,4.74236633668439,3.38258363929778));
#52128=CARTESIAN_POINT('Ctrl Pts',(-11.4546079257229,-0.281725342956251,
5.81829368279896));
#52129=CARTESIAN_POINT('Ctrl Pts',(-11.2159702606036,-5.04698819200419,
2.9085770985024));
#52130=CARTESIAN_POINT('Ctrl Pts',(-10.9773325954844,-5.17544400749208,
-2.67332936120422));
#52131=CARTESIAN_POINT('Ctrl Pts',(-10.7386949303652,-0.549076894375944,
-5.79917451989717));
#52132=CARTESIAN_POINT('Ctrl Pts',(-10.5000572652459,4.58174228182235,-3.5971583522447));
#52133=CARTESIAN_POINT('Ctrl Pts',(-10.2614196001268,5.50318865386573,1.9096662504547));
#52134=CARTESIAN_POINT('Ctrl Pts',(-10.0227819350075,1.36870406540507,5.66202788137834));
#52135=CARTESIAN_POINT('Ctrl Pts',(-9.78414426988828,-4.02324663866633,
4.21252857944289));
#52136=CARTESIAN_POINT('Ctrl Pts',(-9.54550660476906,-5.71892986553813,
-1.10713673103989));
#52137=CARTESIAN_POINT('Ctrl Pts',(-9.30686893964983,-2.16047473976357,
-5.40964503891006));
#52138=CARTESIAN_POINT('Ctrl Pts',(-9.0682312745306,3.38286802356034,-4.74216348129631));
#52139=CARTESIAN_POINT('Ctrl Pts',(-8.82959360941138,5.81827677782428,0.282074254033242));
#52140=CARTESIAN_POINT('Ctrl Pts',(-8.59095594429215,2.90827443535771,5.04716260455295));
#52141=CARTESIAN_POINT('Ctrl Pts',(-8.35231827917293,-2.67363971755611,
5.1752836839061));
#52142=CARTESIAN_POINT('Ctrl Pts',(-8.1136806140537,-5.79920743652394,0.548729128339138));
#52143=CARTESIAN_POINT('Ctrl Pts',(-7.87504294893448,-3.59688358774524,
-4.58195798805725));
#52144=CARTESIAN_POINT('Ctrl Pts',(-7.63640528381524,1.90999626238828,-5.50307412507543));
#52145=CARTESIAN_POINT('Ctrl Pts',(-7.39776761869603,5.66210994965676,-1.36836452227643));
#52146=CARTESIAN_POINT('Ctrl Pts',(-7.15912995357678,4.21228730575213,4.0234992483829));
#52147=CARTESIAN_POINT('Ctrl Pts',(-6.92049228845757,-1.10747968205672,
5.7188634625854));
#52148=CARTESIAN_POINT('Ctrl Pts',(-6.68185462333833,-5.40977458843978,
2.16015032989127));
#52149=CARTESIAN_POINT('Ctrl Pts',(-6.44321695821912,-4.74196060913677,
-3.38315239516401));
#52150=CARTESIAN_POINT('Ctrl Pts',(-6.20457929309988,0.282423164637435,
-5.81825985287354));
#52151=CARTESIAN_POINT('Ctrl Pts',(-5.96594162798066,5.04733699791161,-2.90797175993565));
#52152=CARTESIAN_POINT('Ctrl Pts',(-5.72730396286144,5.17512334370478,2.6739500608018));
#52153=CARTESIAN_POINT('Ctrl Pts',(-5.4886662977422,0.548381356497653,5.79924033899806));
#52154=CARTESIAN_POINT('Ctrl Pts',(-5.25002863262299,-4.58217367045971,
3.59660879744466));
#52155=CARTESIAN_POINT('Ctrl Pts',(-5.01139096750376,-5.5029595906143,-1.91032624275442));
#52156=CARTESIAN_POINT('Ctrl Pts',(-4.77275330238452,-1.3680249471228,-5.66219204498688));
#52157=CARTESIAN_POINT('Ctrl Pts',(-4.53411563726531,4.02375179159935,-4.21204592589478));
#52158=CARTESIAN_POINT('Ctrl Pts',(-4.29547797214607,5.71879713894916,1.10782245436525));
#52159=CARTESIAN_POINT('Ctrl Pts',(-4.05684030702685,2.1598257205091,5.40990445393106));
#52160=CARTESIAN_POINT('Ctrl Pts',(-3.81820264190762,-3.38343638652024,
4.74175707603558));
#52161=CARTESIAN_POINT('Ctrl Pts',(-3.57956497678839,-5.8182436135944,-0.282770838170588));
#52162=CARTESIAN_POINT('Ctrl Pts',(-3.34092731166917,-2.90766771762518,
-5.04751374594047));
#52163=CARTESIAN_POINT('Ctrl Pts',(-3.10228964654994,2.67425779052882,-5.17495842985376));
#52164=CARTESIAN_POINT('Ctrl Pts',(-2.86365198143071,5.79927821925697,-0.54804232686631));
#52165=CARTESIAN_POINT('Ctrl Pts',(-2.62501431631149,3.59632439845965,4.58240612234822));
#52166=CARTESIAN_POINT('Ctrl Pts',(-2.38637665119227,-1.91063779555211,
5.5028128128105));
#52167=CARTESIAN_POINT('Ctrl Pts',(-2.14773898607303,-5.66230948168428,
1.36774722574033));
#52168=CARTESIAN_POINT('Ctrl Pts',(-1.90910132095381,-4.21173664772448,
-4.02412306903384));
#52169=CARTESIAN_POINT('Ctrl Pts',(-1.67046365583459,1.10803490710056,-5.71850283364837));
#52170=CARTESIAN_POINT('Ctrl Pts',(-1.43182599071535,5.41028448303652,-2.15993873727599));
#52171=CARTESIAN_POINT('Ctrl Pts',(-1.19318832559614,4.74107307396736,3.3845606937213));
#52172=CARTESIAN_POINT('Ctrl Pts',(-0.954550660476906,-0.282194523950606,
5.81661222925236));
#52173=CARTESIAN_POINT('Ctrl Pts',(-0.715912995357673,-5.049479635978,2.91048227618002));
#52174=CARTESIAN_POINT('Ctrl Pts',(-0.477275330238451,-5.17121721536142,
-2.68071843402506));
#52175=CARTESIAN_POINT('Ctrl Pts',(-0.278410609305759,-1.32510607804596,
-5.26845855246328));
#52176=CARTESIAN_POINT('Ctrl Pts',(-0.119318832559609,2.02851289583626,
-4.70788567421457));
#52177=CARTESIAN_POINT('Ctrl Pts',(-0.0397729441865337,3.3679595299544,
-3.68587930545211));
#52178=CARTESIAN_POINT('Ctrl Pts',(4.44089209850063E-15,3.87448963569911,
-3.0403873211912));
#52179=CARTESIAN_POINT('Ctrl Pts',(-29.9038972033484,2.6929126153078,-3.77880514723378));
#52180=CARTESIAN_POINT('Ctrl Pts',(-29.8641242591618,3.32246351412783,-3.330164507837));
#52181=CARTESIAN_POINT('Ctrl Pts',(-29.7845783707887,4.34261535808318,-2.11399789240766));
#52182=CARTESIAN_POINT('Ctrl Pts',(-29.6254865940426,5.0161213975182,1.01790548943452));
#52183=CARTESIAN_POINT('Ctrl Pts',(-29.4266218731099,2.74798774171071,4.75030710152848));
#52184=CARTESIAN_POINT('Ctrl Pts',(-29.1879842079907,-2.51952695040288,
4.87900724326607));
#52185=CARTESIAN_POINT('Ctrl Pts',(-28.9493465428715,-5.46208793188772,
0.518672845565351));
#52186=CARTESIAN_POINT('Ctrl Pts',(-28.7107088777522,-3.39170065447864,
-4.31484800050243));
#52187=CARTESIAN_POINT('Ctrl Pts',(-28.472071212633,1.79744621468105,-5.18592618627794));
#52188=CARTESIAN_POINT('Ctrl Pts',(-28.2334335475138,5.33381868024693,-1.29165251384495));
#52189=CARTESIAN_POINT('Ctrl Pts',(-27.9947958823946,3.97059998730579,3.78882986476014));
#52190=CARTESIAN_POINT('Ctrl Pts',(-27.7561582172753,-1.04090109033753,
5.38865370581382));
#52191=CARTESIAN_POINT('Ctrl Pts',(-27.5175205521561,-5.09589824607407,
2.03764600058257));
#52192=CARTESIAN_POINT('Ctrl Pts',(-27.2788828870369,-4.4692572402043,-3.18533704191237));
#52193=CARTESIAN_POINT('Ctrl Pts',(-27.0402452219176,0.26346758077383,-5.48189768940374));
#52194=CARTESIAN_POINT('Ctrl Pts',(-26.8016075567985,4.75410928969372,-2.74207001987724));
#52195=CARTESIAN_POINT('Ctrl Pts',(-26.5629698916792,4.87703456275017,2.51696353520732));
#52196=CARTESIAN_POINT('Ctrl Pts',(-26.32433222656,0.519286231809787,5.46359825096759));
#52197=CARTESIAN_POINT('Ctrl Pts',(-26.0856945614407,-4.31554067523491,
3.39067226195794));
#52198=CARTESIAN_POINT('Ctrl Pts',(-25.8470568963215,-5.18556360046217,
-1.79735638292817));
#52199=CARTESIAN_POINT('Ctrl Pts',(-25.6084192312023,-1.29146536700809,
-5.33410491268233));
#52200=CARTESIAN_POINT('Ctrl Pts',(-25.3697815660831,3.78913709957896,-3.97026401239249));
#52201=CARTESIAN_POINT('Ctrl Pts',(-25.1311439009638,5.38855526275784,1.04116758046706));
#52202=CARTESIAN_POINT('Ctrl Pts',(-24.8925062358446,2.03735916570693,5.09604994331312));
#52203=CARTESIAN_POINT('Ctrl Pts',(-24.6538685707254,-3.18561482108248,
4.46905083992566));
#52204=CARTESIAN_POINT('Ctrl Pts',(-24.4152309056062,-5.48187678927333,
-0.263788310288471));
#52205=CARTESIAN_POINT('Ctrl Pts',(-24.1765932404869,-2.74178757222978,
-4.75427788952306));
#52206=CARTESIAN_POINT('Ctrl Pts',(-23.9379555753677,2.51725737821055,-4.87688144343666));
#52207=CARTESIAN_POINT('Ctrl Pts',(-23.6993179102484,5.46362866211312,-0.518959721751974));
#52208=CARTESIAN_POINT('Ctrl Pts',(-23.4606802451293,3.39041383626465,4.31574458911784));
#52209=CARTESIAN_POINT('Ctrl Pts',(-23.22204258001,-1.79766754297636,5.1854555000254));
#52210=CARTESIAN_POINT('Ctrl Pts',(-22.9834049148908,-5.33418224799811,
1.29114564897465));
#52211=CARTESIAN_POINT('Ctrl Pts',(-22.7447672497716,-3.97003683117282,
-3.78937526502026));
#52212=CARTESIAN_POINT('Ctrl Pts',(-22.5061295846523,1.04149074721631,-5.38849277288));
#52213=CARTESIAN_POINT('Ctrl Pts',(-22.2674919195332,5.09617209617701,-2.03705358461264));
#52214=CARTESIAN_POINT('Ctrl Pts',(-22.0288542544139,4.46885980435008,3.18588282729214));
#52215=CARTESIAN_POINT('Ctrl Pts',(-21.7902165892947,-0.264117051042074,
5.48186095441396));
#52216=CARTESIAN_POINT('Ctrl Pts',(-21.5515789241754,-4.75444229852842,
2.74150246584068));
#52217=CARTESIAN_POINT('Ctrl Pts',(-21.3129412590562,-4.87673048077228,
-2.51754983229987));
#52218=CARTESIAN_POINT('Ctrl Pts',(-21.074303593937,-0.518632077245404,
-5.46365977241106));
#52219=CARTESIAN_POINT('Ctrl Pts',(-20.8356659288178,4.31594789749319,-3.39015502393968));
#52220=CARTESIAN_POINT('Ctrl Pts',(-20.5970282636985,5.1853476882785,1.79797850150613));
#52221=CARTESIAN_POINT('Ctrl Pts',(-20.3583905985793,1.29082576619906,5.3342596657391));
#52222=CARTESIAN_POINT('Ctrl Pts',(-20.1197529334601,-3.78961333343518,
3.96980958274648));
#52223=CARTESIAN_POINT('Ctrl Pts',(-19.8811152683408,-5.38843030706872,
-1.04181388264786));
#52224=CARTESIAN_POINT('Ctrl Pts',(-19.6424776032216,-2.0367479735616,-5.09629424507725));
#52225=CARTESIAN_POINT('Ctrl Pts',(-19.4038399381024,3.18615081025577,-4.46866874522171));
#52226=CARTESIAN_POINT('Ctrl Pts',(-19.1652022729832,5.48184510598211,0.264445786948331));
#52227=CARTESIAN_POINT('Ctrl Pts',(-18.9265646078639,2.74121734639358,4.75460669246635));
#52228=CARTESIAN_POINT('Ctrl Pts',(-18.6879269427447,-2.51784227566918,
4.87657949951273));
#52229=CARTESIAN_POINT('Ctrl Pts',(-18.4492892776255,-5.46369086392892,
0.518304431424697));
#52230=CARTESIAN_POINT('Ctrl Pts',(-18.2106516125063,-3.38989619897094,
-4.31615119063469));
#52231=CARTESIAN_POINT('Ctrl Pts',(-17.972013947387,1.7982894533345,-5.18523985773471));
#52232=CARTESIAN_POINT('Ctrl Pts',(-17.7333762822678,5.33433706441994,-1.29050587885931));
#52233=CARTESIAN_POINT('Ctrl Pts',(-17.4947386171486,3.96958231998011,3.78985138826264));
#52234=CARTESIAN_POINT('Ctrl Pts',(-17.2561009520293,-1.04213701429963,
5.38836782185863));
#52235=CARTESIAN_POINT('Ctrl Pts',(-17.0174632869101,-5.09641637566774,
2.03644235519705));
#52236=CARTESIAN_POINT('Ctrl Pts',(-16.7788256217909,-4.46847767001423,
-3.18641878176725));
#52237=CARTESIAN_POINT('Ctrl Pts',(-16.5401879566717,0.264774521898913,
-5.48182923783365));
#52238=CARTESIAN_POINT('Ctrl Pts',(-16.3015502915525,4.7547710693084,-2.74093221709016));
#52239=CARTESIAN_POINT('Ctrl Pts',(-16.0629126264332,4.87642850071492,2.51813470998477));
#52240=CARTESIAN_POINT('Ctrl Pts',(-15.824274961314,0.517976783740707,5.46372193579801));
#52241=CARTESIAN_POINT('Ctrl Pts',(-15.5856372961948,-4.31635446825496,
3.38963736181178));
#52242=CARTESIAN_POINT('Ctrl Pts',(-15.3469996310756,-5.18513200854378,
-1.79860039869607));
#52243=CARTESIAN_POINT('Ctrl Pts',(-15.1083619659563,-1.29018598687877,
-5.33441444391757));
#52244=CARTESIAN_POINT('Ctrl Pts',(-14.8697243008371,3.7900894294612,-3.9693550429385));
#52245=CARTESIAN_POINT('Ctrl Pts',(-14.6310866357179,5.38830531727106,1.0424601422037));
#52246=CARTESIAN_POINT('Ctrl Pts',(-14.3924489705986,2.03613672950916,5.09653848793067));
#52247=CARTESIAN_POINT('Ctrl Pts',(-14.1538113054794,-3.18668674181981,
4.46828657873739));
#52248=CARTESIAN_POINT('Ctrl Pts',(-13.9151736403602,-5.48181334997165,
-0.265103255897302));
#52249=CARTESIAN_POINT('Ctrl Pts',(-13.6765359752409,-2.74064707792992,
-4.75493542905149));
#52250=CARTESIAN_POINT('Ctrl Pts',(-13.4378983101217,2.51842713524471,-4.87627748438068));
#52251=CARTESIAN_POINT('Ctrl Pts',(-13.1992606450025,5.46375298801868,-0.517649134193991));
#52252=CARTESIAN_POINT('Ctrl Pts',(-12.9606229798833,3.38937851246291,4.31655773035292));
#52253=CARTESIAN_POINT('Ctrl Pts',(-12.721985314764,-1.79891133758957,5.18502414070623));
#52254=CARTESIAN_POINT('Ctrl Pts',(-12.4833476496448,-5.33449180423179,
1.28986609025851));
#52255=CARTESIAN_POINT('Ctrl Pts',(-12.2447099845256,-3.96912775162243,
-3.79032745703001));
#52256=CARTESIAN_POINT('Ctrl Pts',(-12.0060723194064,1.04278326635893,-5.38824279330623));
#52257=CARTESIAN_POINT('Ctrl Pts',(-11.7674346542871,5.0966605818656,-2.03583109649899));
#52258=CARTESIAN_POINT('Ctrl Pts',(-11.5287969891679,4.46809547139186,3.18695469041253));
#52259=CARTESIAN_POINT('Ctrl Pts',(-11.2901593240487,-0.265431988942334,
5.48179744239614));
#52260=CARTESIAN_POINT('Ctrl Pts',(-11.0515216589295,-4.75509977169506,
2.74036192891386));
#52261=CARTESIAN_POINT('Ctrl Pts',(-10.8128839938102,-4.87612645051055,
-2.51871955144797));
#52262=CARTESIAN_POINT('Ctrl Pts',(-10.574246328691,-0.517321482785775,
-5.46378402059077));
#52263=CARTESIAN_POINT('Ctrl Pts',(-10.3356086635718,4.3167609769278,-3.38911965092534));
#52264=CARTESIAN_POINT('Ctrl Pts',(-10.0969709984526,5.18491625422252,1.79922227001388));
#52265=CARTESIAN_POINT('Ctrl Pts',(-9.85833333333333,1.28954618899972,5.33456914536226));
#52266=CARTESIAN_POINT('Ctrl Pts',(-9.61969566821411,-3.79056547096819,
3.96890044603278));
#52267=CARTESIAN_POINT('Ctrl Pts',(-9.38105800309488,-5.38818024996436,
-1.04310638676421));
#52268=CARTESIAN_POINT('Ctrl Pts',(-9.14242033797565,-2.03552545616774,
-5.09678265747193));
#52269=CARTESIAN_POINT('Ctrl Pts',(-8.90378267285643,3.18722262754464,-4.46790434797868));
#52270=CARTESIAN_POINT('Ctrl Pts',(-8.6651450077372,5.48178151510679,0.265760721033513));
#52271=CARTESIAN_POINT('Ctrl Pts',(-8.42650734261798,2.74007677004376,4.7552640972372));
#52272=CARTESIAN_POINT('Ctrl Pts',(-8.18786967749874,-2.51901195859494,
4.87597539910758));
#52273=CARTESIAN_POINT('Ctrl Pts',(-7.94923201237954,-5.46381503351144,
0.516993829512319));
#52274=CARTESIAN_POINT('Ctrl Pts',(-7.71059434726029,-3.38886077720523,
-4.31696420796962));
#52275=CARTESIAN_POINT('Ctrl Pts',(-7.47195668214107,1.7995331959781,-5.18480834911082));
#52276=CARTESIAN_POINT('Ctrl Pts',(-7.23331901702184,5.33464646728914,-1.28922628306928));
#52277=CARTESIAN_POINT('Ctrl Pts',(-6.99468135190262,3.96867312620793,3.79080347120911));
#52278=CARTESIAN_POINT('Ctrl Pts',(-6.75604368678338,-1.04342950349043,
5.38811768737191));
#52279=CARTESIAN_POINT('Ctrl Pts',(-6.51740602166417,-5.09690471461091,
2.03521980827418));
#52280=CARTESIAN_POINT('Ctrl Pts',(-6.27876835654494,-4.467713208764,-3.18749055274999));
#52281=CARTESIAN_POINT('Ctrl Pts',(-6.04013069142571,0.266089452679246,
-5.48176556899668));
#52282=CARTESIAN_POINT('Ctrl Pts',(-5.80149302630648,4.75542840469908,-2.73979159960635));
#52283=CARTESIAN_POINT('Ctrl Pts',(-5.56285536118726,4.87582433205023,2.5193043533937));
#52284=CARTESIAN_POINT('Ctrl Pts',(-5.32421769606802,0.516666170769886,
5.46384603309797));
#52285=CARTESIAN_POINT('Ctrl Pts',(-5.08558003094881,-4.31716741655734,
3.38860187917618));
#52286=CARTESIAN_POINT('Ctrl Pts',(-4.84694236582958,-5.18470043865627,
-1.79984409220056));
#52287=CARTESIAN_POINT('Ctrl Pts',(-4.60830470071034,-1.28890634696599,
-5.3347238147032));
#52288=CARTESIAN_POINT('Ctrl Pts',(-4.36966703559113,3.79104140879587,-3.96844570635655));
#52289=CARTESIAN_POINT('Ctrl Pts',(-4.13102937047189,5.38805519950874,1.04375245184379));
#52290=CARTESIAN_POINT('Ctrl Pts',(-3.89239170535267,2.03491397240924,5.09702706943807));
#52291=CARTESIAN_POINT('Ctrl Pts',(-3.65375404023344,-3.18775811969919,
4.46752144683269));
#52292=CARTESIAN_POINT('Ctrl Pts',(-3.41511637511422,-5.48175026890294,
-0.266417018798925));
#52293=CARTESIAN_POINT('Ctrl Pts',(-3.17647870999499,-2.7395051413334,-4.75559493065073));
#52294=CARTESIAN_POINT('Ctrl Pts',(-2.93784104487577,2.51959428582449,-4.87566895585645));
#52295=CARTESIAN_POINT('Ctrl Pts',(-2.69920337975653,5.4638817225832,-0.516346748639057));
#52296=CARTESIAN_POINT('Ctrl Pts',(-2.46056571463731,3.38833392817308,4.31738642478165));
#52297=CARTESIAN_POINT('Ctrl Pts',(-2.22192804951809,-1.80013762659788,
5.18456214962629));
#52298=CARTESIAN_POINT('Ctrl Pts',(-1.98329038439885,-5.33483445954559,
1.28864468737176));
#52299=CARTESIAN_POINT('Ctrl Pts',(-1.74465271927964,-3.96815431503542,
-3.79139121370463));
#52300=CARTESIAN_POINT('Ctrl Pts',(-1.50601505416041,1.0439526175495,-5.38777791511351));
#52301=CARTESIAN_POINT('Ctrl Pts',(-1.26737738904118,5.09738511987209,-2.03502045294416));
#52302=CARTESIAN_POINT('Ctrl Pts',(-1.02873972392196,4.46687700346276,3.18881740351592));
#52303=CARTESIAN_POINT('Ctrl Pts',(-0.790102058802729,-0.265874035238907,
5.48021323433553));
#52304=CARTESIAN_POINT('Ctrl Pts',(-0.551464393683494,-4.75744712505124,
2.74215692220397));
#52305=CARTESIAN_POINT('Ctrl Pts',(-0.312826728564273,-4.87214411143407,
-2.52568128330601));
#52306=CARTESIAN_POINT('Ctrl Pts',(-0.113962007631581,-1.24846965546114,
-4.96376157560509));
#52307=CARTESIAN_POINT('Ctrl Pts',(0.0451297691145686,1.91119551719046,
-4.43560896973968));
#52308=CARTESIAN_POINT('Ctrl Pts',(0.124675657487644,3.17317635443185,-3.47270950061224));
#52309=CARTESIAN_POINT('Ctrl Pts',(0.164448601674182,3.65041170719118,-2.86454901554259));
#52310=CARTESIAN_POINT('Ctrl Pts',(-29.7394486016742,2.52761008811552,-3.54684587865065));
#52311=CARTESIAN_POINT('Ctrl Pts',(-29.6996756574876,3.11851645239715,-3.12574472608009));
#52312=CARTESIAN_POINT('Ctrl Pts',(-29.6201297691146,4.07604700037463,-1.9842316340791));
#52313=CARTESIAN_POINT('Ctrl Pts',(-29.4610379923684,4.70821035020098,0.955422084332599));
#52314=CARTESIAN_POINT('Ctrl Pts',(-29.2621732714357,2.57930446702286,4.45871287587165));
#52315=CARTESIAN_POINT('Ctrl Pts',(-29.0235356063165,-2.36486757903556,
4.57951285086845));
#52316=CARTESIAN_POINT('Ctrl Pts',(-28.7848979411973,-5.12680154578104,
0.486834481531294));
#52317=CARTESIAN_POINT('Ctrl Pts',(-28.546260276078,-3.18350352009034,-4.04998412230631));
#52318=CARTESIAN_POINT('Ctrl Pts',(-28.3076226109588,1.6871112561347,-4.86759179267321));
#52319=CARTESIAN_POINT('Ctrl Pts',(-28.0689849458396,5.00640601099863,-1.21236534218581));
#52320=CARTESIAN_POINT('Ctrl Pts',(-27.8303472807204,3.72686752876241,3.55625523601567));
#52321=CARTESIAN_POINT('Ctrl Pts',(-27.5917096156011,-0.977006116615824,
5.05787502748919));
#52322=CARTESIAN_POINT('Ctrl Pts',(-27.3530719504819,-4.7830901536011,1.91256654887478));
#52323=CARTESIAN_POINT('Ctrl Pts',(-27.1144342853627,-4.19491506055882,
-2.98980739123073));
#52324=CARTESIAN_POINT('Ctrl Pts',(-26.8757966202435,0.247294810559338,
-5.1453952954096));
#52325=CARTESIAN_POINT('Ctrl Pts',(-26.6371589551242,4.46228166941837,-2.57375000033875));
#52326=CARTESIAN_POINT('Ctrl Pts',(-26.398521290005,4.57766126194414,2.3624615172601));
#52327=CARTESIAN_POINT('Ctrl Pts',(-26.1598836248858,0.487410215497018,
5.12821915499749));
#52328=CARTESIAN_POINT('Ctrl Pts',(-25.9212459597666,-4.05063427769259,
3.1825382547137));
#52329=CARTESIAN_POINT('Ctrl Pts',(-25.6826082946473,-4.86725146393007,
-1.68702693864012));
#52330=CARTESIAN_POINT('Ctrl Pts',(-25.4439706295281,-1.21218968322454,
-5.0066746732594));
#52331=CARTESIAN_POINT('Ctrl Pts',(-25.2053329644089,3.55654361144349,-3.7265521774304));
#52332=CARTESIAN_POINT('Ctrl Pts',(-24.9666952992897,5.05778262729025,0.977256248438136));
#52333=CARTESIAN_POINT('Ctrl Pts',(-24.7280576341704,1.91229732115414,4.78323253901292));
#52334=CARTESIAN_POINT('Ctrl Pts',(-24.4894199690512,-2.99006811912389,
4.19472133001462));
#52335=CARTESIAN_POINT('Ctrl Pts',(-24.250782303932,-5.14537567821884,-0.247595852320659));
#52336=CARTESIAN_POINT('Ctrl Pts',(-24.0121446388127,-2.57348489053941,
-4.46243991986699));
#52337=CARTESIAN_POINT('Ctrl Pts',(-23.7735069736935,2.3627373229194,-4.57751754175089));
#52338=CARTESIAN_POINT('Ctrl Pts',(-23.5348693085743,5.12824769937646,-0.487103748027066));
#52339=CARTESIAN_POINT('Ctrl Pts',(-23.2962316434551,3.18229569229794,4.05082567446672));
#52340=CARTESIAN_POINT('Ctrl Pts',(-23.0575939783358,-1.68731899834989,
4.8671499991618));
#52341=CARTESIAN_POINT('Ctrl Pts',(-22.8189563132166,-5.00674726140177,
1.21188959085538));
#52342=CARTESIAN_POINT('Ctrl Pts',(-22.5803186480974,-3.72633894156846,
-3.55676715726841));
#52343=CARTESIAN_POINT('Ctrl Pts',(-22.3416809829781,0.97755957782614,-5.05772397330915));
#52344=CARTESIAN_POINT('Ctrl Pts',(-22.1030433178589,4.78334719361007,-1.91201049793817));
#52345=CARTESIAN_POINT('Ctrl Pts',(-21.8644056527397,4.19454202102207,2.99031967396282));
#52346=CARTESIAN_POINT('Ctrl Pts',(-21.6257679876205,-0.247904413556711,
5.14536081537106));
#52347=CARTESIAN_POINT('Ctrl Pts',(-21.3871303225013,-4.4625942367424,2.57321728520339));
#52348=CARTESIAN_POINT('Ctrl Pts',(-21.148492657382,-4.57737584582237,-2.36301182492228));
#52349=CARTESIAN_POINT('Ctrl Pts',(-20.9098549922628,-0.486796215745698,
-5.12827689999088));
#52350=CARTESIAN_POINT('Ctrl Pts',(-20.6712173271436,4.05101650290193,-3.18205276698362));
#52351=CARTESIAN_POINT('Ctrl Pts',(-20.4325796620244,4.86704880536236,1.68761086891128));
#52352=CARTESIAN_POINT('Ctrl Pts',(-20.1939419969051,1.21158934385664,5.00681992690976));
#52353=CARTESIAN_POINT('Ctrl Pts',(-19.9553043317859,-3.55699061202287,
3.72612564262527));
#52354=CARTESIAN_POINT('Ctrl Pts',(-19.7166666666667,-5.05766534191731,
-0.977862877818859));
#52355=CARTESIAN_POINT('Ctrl Pts',(-19.4780290015474,-1.91172364660431,
-4.78346184448688));
#52356=CARTESIAN_POINT('Ctrl Pts',(-19.2393913364282,2.99057120698267,-4.19436268992253));
#52357=CARTESIAN_POINT('Ctrl Pts',(-19.000753671309,5.14534593978394,0.248212970242977));
#52358=CARTESIAN_POINT('Ctrl Pts',(-18.7621160061898,2.57294966761094,4.46274853947527));
#52359=CARTESIAN_POINT('Ctrl Pts',(-18.5234783410705,-2.36328631686318,
4.57723413244015));
#52360=CARTESIAN_POINT('Ctrl Pts',(-18.2848406759513,-5.12830608297801,
0.486488682230852));
#52361=CARTESIAN_POINT('Ctrl Pts',(-18.0462030108321,-3.18180982980166,
-4.0512073170384));
#52362=CARTESIAN_POINT('Ctrl Pts',(-17.8075653457129,1.68790273318265,-4.86694759391988));
#52363=CARTESIAN_POINT('Ctrl Pts',(-17.5689276805936,5.00689257452757,-1.21128909257392));
#52364=CARTESIAN_POINT('Ctrl Pts',(-17.3302900154744,3.72591233022232,3.55721405402392));
#52365=CARTESIAN_POINT('Ctrl Pts',(-17.0916523503552,-0.978166174263816,
5.05760669231743));
#52366=CARTESIAN_POINT('Ctrl Pts',(-16.8530146852359,-4.78357647817786,
1.91143678840589));
#52367=CARTESIAN_POINT('Ctrl Pts',(-16.6143770201167,-4.19418334373088,
-2.99082272925335));
#52368=CARTESIAN_POINT('Ctrl Pts',(-16.3757393549975,0.248521526032233,
-5.14533104569049));
#52369=CARTESIAN_POINT('Ctrl Pts',(-16.1371016898783,4.46290282616169,-2.57268204076719));
#52370=CARTESIAN_POINT('Ctrl Pts',(-15.8984640247591,4.57709240259623,2.36356080030613));
#52371=CARTESIAN_POINT('Ctrl Pts',(-15.6598263596398,0.486181146967108,
5.12833524752249));
#52372=CARTESIAN_POINT('Ctrl Pts',(-15.4211886945206,-4.05139811660642,
3.18156688117757));
#52373=CARTESIAN_POINT('Ctrl Pts',(-15.1825510294014,-4.86684636497488,
-1.68819459138417));
#52374=CARTESIAN_POINT('Ctrl Pts',(-14.9439133642821,-1.21098883693528,
-5.00696520413972));
#52375=CARTESIAN_POINT('Ctrl Pts',(-14.7052756991629,3.55743748323268,-3.7256990044204));
#52376=CARTESIAN_POINT('Ctrl Pts',(-14.4666380340437,5.05754802452954,0.978469467191119));
#52377=CARTESIAN_POINT('Ctrl Pts',(-14.2280003689245,1.91114992333367,4.7836910946663));
#52378=CARTESIAN_POINT('Ctrl Pts',(-13.9893627038052,-2.99107424076851,
4.19400398245627));
#52379=CARTESIAN_POINT('Ctrl Pts',(-13.750725038686,-5.1453161330936,-0.248830080927746));
#52380=CARTESIAN_POINT('Ctrl Pts',(-13.5120873735668,-2.57241440467166,
-4.46305709679875));
#52381=CARTESIAN_POINT('Ctrl Pts',(-13.2734497084476,2.3638352752493,-4.57695065629236));
#52382=CARTESIAN_POINT('Ctrl Pts',(-13.0348120433283,5.12836439362466,-0.485873609954974));
#52383=CARTESIAN_POINT('Ctrl Pts',(-12.7961743782091,3.18132392111204,4.05158890160494));
#52384=CARTESIAN_POINT('Ctrl Pts',(-12.5575367130899,-1.68848644351467,
4.86674511852789));
#52385=CARTESIAN_POINT('Ctrl Pts',(-12.3188990479707,-5.00703781574603,
1.21068857694173));
#52386=CARTESIAN_POINT('Ctrl Pts',(-12.0802613828514,-3.72548566522024,
-3.55766089964832));
#52387=CARTESIAN_POINT('Ctrl Pts',(-11.8416237177322,0.978772756599708,
-5.05748933855386));
#52388=CARTESIAN_POINT('Ctrl Pts',(-11.602986052613,4.78380569395181,-1.91086305138862));
#52389=CARTESIAN_POINT('Ctrl Pts',(-11.3643483874938,4.19382460609933,2.99132574152728));
#52390=CARTESIAN_POINT('Ctrl Pts',(-11.1257107223745,-0.249138634928415,
5.14530120199331));
#52391=CARTESIAN_POINT('Ctrl Pts',(-10.8870730572553,-4.46321135138594,
2.57214675932532));
#52392=CARTESIAN_POINT('Ctrl Pts',(-10.6484353921361,-4.57680889352901,
-2.36410974169172));
#52393=CARTESIAN_POINT('Ctrl Pts',(-10.4097977270168,-0.485566071195607,
-5.12839352128436));
#52394=CARTESIAN_POINT('Ctrl Pts',(-10.1711600618976,4.05177967203326,-3.18108094960599));
#52395=CARTESIAN_POINT('Ctrl Pts',(-9.93252239677838,4.86664385457931,1.68877828957306));
#52396=CARTESIAN_POINT('Ctrl Pts',(-9.69388473165916,1.21038831259436,5.00711040934616));
#52397=CARTESIAN_POINT('Ctrl Pts',(-9.45524706653992,-3.55788430327004,
3.72527231262268));
#52398=CARTESIAN_POINT('Ctrl Pts',(-9.21660940142071,-5.0574306343906,-0.979076042488542));
#52399=CARTESIAN_POINT('Ctrl Pts',(-8.97797173630147,-1.91057617257191,
-4.78392027603378));
#52400=CARTESIAN_POINT('Ctrl Pts',(-8.73933407118225,2.99157723152894,-4.19364521466106));
#52401=CARTESIAN_POINT('Ctrl Pts',(-8.50069640606303,5.14528625238931,0.249447188033793));
#52402=CARTESIAN_POINT('Ctrl Pts',(-8.26205874094379,2.57187910472981,4.46336558992145));
#52403=CARTESIAN_POINT('Ctrl Pts',(-8.02342107582458,-2.36438419963377,
4.57666711430907));
#52404=CARTESIAN_POINT('Ctrl Pts',(-7.78478341070534,-5.12842263049894,
0.485258530685497));
#52405=CARTESIAN_POINT('Ctrl Pts',(-7.54614574558613,-3.18083796666522,
-4.051970427882));
#52406=CARTESIAN_POINT('Ctrl Pts',(-7.30750808046688,1.68907012956793,-4.86654257314621));
#52407=CARTESIAN_POINT('Ctrl Pts',(-7.06887041534768,5.00718298492152,-1.21008804386212));
#52408=CARTESIAN_POINT('Ctrl Pts',(-6.83023275022843,3.72505894666373,3.55810769403531));
#52409=CARTESIAN_POINT('Ctrl Pts',(-6.59159508510922,-0.979379324924138,
5.05737191215842));
#52410=CARTESIAN_POINT('Ctrl Pts',(-6.35295741998998,-4.78403484078203,
1.91028928665709));
#52411=CARTESIAN_POINT('Ctrl Pts',(-6.11431975487076,-4.19346580839123,
-2.99182871033596));
#52412=CARTESIAN_POINT('Ctrl Pts',(-5.87568208975153,0.24975574072106,-5.14527128511983));
#52413=CARTESIAN_POINT('Ctrl Pts',(-5.63704442463231,4.46351981148654,-2.57161143927705));
#52414=CARTESIAN_POINT('Ctrl Pts',(-5.39840675951308,4.57652532039568,2.3646586459856));
#52415=CARTESIAN_POINT('Ctrl Pts',(-5.15976909439384,0.48495098504212,5.12845172719788));
#52416=CARTESIAN_POINT('Ctrl Pts',(-4.92113142927463,-4.05216116265496,
3.18059496090769));
#52417=CARTESIAN_POINT('Ctrl Pts',(-4.68249376415541,-4.86644128669823,
-1.68936194164671));
#52418=CARTESIAN_POINT('Ctrl Pts',(-4.44385609903616,-1.20978774680917,
-5.00725558441954));
#52419=CARTESIAN_POINT('Ctrl Pts',(-4.20521843391696,3.55833102599239,-3.72484548681831));
#52420=CARTESIAN_POINT('Ctrl Pts',(-3.96658076879771,5.05731326006834,0.97968244932232));
#52421=CARTESIAN_POINT('Ctrl Pts',(-3.7279431036785,1.91000222430937,4.78414968494508));
#52422=CARTESIAN_POINT('Ctrl Pts',(-3.48930543855926,-2.99207985287812,
4.1932858176298));
#52423=CARTESIAN_POINT('Ctrl Pts',(-3.25066777344004,-5.14525692421147,
-0.250063199427267));
#52424=CARTESIAN_POINT('Ctrl Pts',(-3.01203010832081,-2.57134256504161,
-4.46367611536099));
#52425=CARTESIAN_POINT('Ctrl Pts',(-2.77339244320159,2.36493078112016,-4.57637948185914));
#52426=CARTESIAN_POINT('Ctrl Pts',(-2.53475477808235,5.12848522590942,-0.484651170411792));
#52427=CARTESIAN_POINT('Ctrl Pts',(-2.29611711296313,3.1803434578865,4.05236672721506));
#52428=CARTESIAN_POINT('Ctrl Pts',(-2.0574794478439,-1.68963745764365,4.86631148644208));
#52429=CARTESIAN_POINT('Ctrl Pts',(-1.81884178272468,-5.00735943740691,
1.20954214900319));
#52430=CARTESIAN_POINT('Ctrl Pts',(-1.58020411760546,-3.72457198234636,
-3.55865935837542));
#52431=CARTESIAN_POINT('Ctrl Pts',(-1.34156645248623,0.979870327998434,
-5.05705299657864));
#52432=CARTESIAN_POINT('Ctrl Pts',(-1.102928787367,4.78448575670765,-1.91010216861234));
#52433=CARTESIAN_POINT('Ctrl Pts',(-0.86429112224778,4.19268093295817,2.99307411331055));
#52434=CARTESIAN_POINT('Ctrl Pts',(-0.62565345712855,-0.24955354652721,
5.14381423941869));
#52435=CARTESIAN_POINT('Ctrl Pts',(-0.387015792009318,-4.46541461412448,
2.57383156822791));
#52436=CARTESIAN_POINT('Ctrl Pts',(-0.148378126890095,-4.57307100750672,
-2.37064413258696));
#52437=CARTESIAN_POINT('Ctrl Pts',(0.050486594042596,-1.17183323287632,
-4.6590645987469));
#52438=CARTESIAN_POINT('Ctrl Pts',(0.209578370788747,1.79387813854466,-4.16333226526479));
#52439=CARTESIAN_POINT('Ctrl Pts',(0.289124259161822,2.9783931789093,-3.25953969577237));
#52440=CARTESIAN_POINT('Ctrl Pts',(0.32889720334836,3.42633377868325,-2.68871070989398));
#52441=CARTESIAN_POINT('Ctrl Pts',(-29.575,2.36230756092324,-3.31488661006752));
#52442=CARTESIAN_POINT('Ctrl Pts',(-29.5352270558135,2.91456939066647,-2.92132494432319));
#52443=CARTESIAN_POINT('Ctrl Pts',(-29.4556811674404,3.80947864266608,-1.85446537575054));
#52444=CARTESIAN_POINT('Ctrl Pts',(-29.2965893906943,4.40029930288375,0.892938679230673));
#52445=CARTESIAN_POINT('Ctrl Pts',(-29.0977246697615,2.41062119233501,4.16711865021482));
#52446=CARTESIAN_POINT('Ctrl Pts',(-28.8590870046423,-2.21020820766824,
4.28001845847083));
#52447=CARTESIAN_POINT('Ctrl Pts',(-28.6204493395231,-4.79151515967436,
0.454996117497237));
#52448=CARTESIAN_POINT('Ctrl Pts',(-28.3818116744039,-2.97530638570203,
-3.7851202441102));
#52449=CARTESIAN_POINT('Ctrl Pts',(-28.1431740092847,1.57677629758835,-4.54925739906848));
#52450=CARTESIAN_POINT('Ctrl Pts',(-27.9045363441654,4.67899334175034,-1.13307817052668));
#52451=CARTESIAN_POINT('Ctrl Pts',(-27.6658986790463,3.48313507021902,3.32368060727122));
#52452=CARTESIAN_POINT('Ctrl Pts',(-27.4272610139269,-0.913111142894123,
4.72709634916456));
#52453=CARTESIAN_POINT('Ctrl Pts',(-27.1886233488078,-4.47028206112812,
1.78748709716699));
#52454=CARTESIAN_POINT('Ctrl Pts',(-26.9499856836885,-3.92057288091334,
-2.79427774054909));
#52455=CARTESIAN_POINT('Ctrl Pts',(-26.7113480185693,0.231122040344854,
-4.80889290141546));
#52456=CARTESIAN_POINT('Ctrl Pts',(-26.4727103534501,4.17045404914302,-2.40542998080026));
#52457=CARTESIAN_POINT('Ctrl Pts',(-26.2340726883308,4.27828796113812,2.20795949931288));
#52458=CARTESIAN_POINT('Ctrl Pts',(-25.9954350232116,0.45553419918425,4.79284005902739));
#52459=CARTESIAN_POINT('Ctrl Pts',(-25.7567973580924,-3.78572788015027,
2.97440424746946));
#52460=CARTESIAN_POINT('Ctrl Pts',(-25.5181596929732,-4.54893932739796,
-1.57669749435209));
#52461=CARTESIAN_POINT('Ctrl Pts',(-25.2795220278539,-1.132913999441,-4.67924443383647));
#52462=CARTESIAN_POINT('Ctrl Pts',(-25.0408843627347,3.32395012330801,-3.48284034246832));
#52463=CARTESIAN_POINT('Ctrl Pts',(-24.8022466976155,4.72700999182265,0.913344916409211));
#52464=CARTESIAN_POINT('Ctrl Pts',(-24.5636090324962,1.78723547660136,4.47041513471273));
#52465=CARTESIAN_POINT('Ctrl Pts',(-24.324971367377,-2.7945214171653,3.92039182010356));
#52466=CARTESIAN_POINT('Ctrl Pts',(-24.0863337022578,-4.80887456716434,
-0.231403394352836));
#52467=CARTESIAN_POINT('Ctrl Pts',(-23.8476960371386,-2.40518220884904,
-4.17060195021093));
#52468=CARTESIAN_POINT('Ctrl Pts',(-23.6090583720194,2.20821726762825,-4.27815364006511));
#52469=CARTESIAN_POINT('Ctrl Pts',(-23.3704207069001,4.7928667366398,-0.455247774302161));
#52470=CARTESIAN_POINT('Ctrl Pts',(-23.1317830417809,2.97417754833123,3.7859067598156));
#52471=CARTESIAN_POINT('Ctrl Pts',(-22.8931453766616,-1.57697045372341,
4.54884449829819));
#52472=CARTESIAN_POINT('Ctrl Pts',(-22.6545077115425,-4.67931227480544,
1.13263353273611));
#52473=CARTESIAN_POINT('Ctrl Pts',(-22.4158700464232,-3.48264105196409,
-3.32415904951658));
#52474=CARTESIAN_POINT('Ctrl Pts',(-22.177232381304,0.913628408435968,-4.7269551737383));
#52475=CARTESIAN_POINT('Ctrl Pts',(-21.9385947161847,4.47052229104313,-1.7869674112637));
#52476=CARTESIAN_POINT('Ctrl Pts',(-21.6999570510656,3.92022423769407,2.79475652063351));
#52477=CARTESIAN_POINT('Ctrl Pts',(-21.4613193859463,-0.231691776071347,
4.80886067632815));
#52478=CARTESIAN_POINT('Ctrl Pts',(-21.2226817208271,-4.17074617495639,
2.40493210456611));
#52479=CARTESIAN_POINT('Ctrl Pts',(-20.9840440557078,-4.27802121087247,
-2.20847381754468));
#52480=CARTESIAN_POINT('Ctrl Pts',(-20.7454063905886,-0.454960354245989,
-4.79289402757069));
#52481=CARTESIAN_POINT('Ctrl Pts',(-20.5067687254694,3.78608510831067,-2.97395051002756));
#52482=CARTESIAN_POINT('Ctrl Pts',(-20.2681310603502,4.54874992244621,1.57724323631644));
#52483=CARTESIAN_POINT('Ctrl Pts',(-20.0294933952309,1.13235292151423,4.67938018808041));
#52484=CARTESIAN_POINT('Ctrl Pts',(-19.7908557301117,-3.32436789061056,
3.48244170250407));
#52485=CARTESIAN_POINT('Ctrl Pts',(-19.5522180649925,-4.7269003767659,-0.91391187298986));
#52486=CARTESIAN_POINT('Ctrl Pts',(-19.3135803998733,-1.78669931964703,
-4.4706294438965));
#52487=CARTESIAN_POINT('Ctrl Pts',(-19.074942734754,2.79499160370957,-3.92005663462335));
#52488=CARTESIAN_POINT('Ctrl Pts',(-18.8363050696348,4.80884677358576,0.231980153537627));
#52489=CARTESIAN_POINT('Ctrl Pts',(-18.5976674045156,2.4046819888283,4.1708903864842));
#52490=CARTESIAN_POINT('Ctrl Pts',(-18.3590297393964,-2.20873035805718,
4.27788876536757));
#52491=CARTESIAN_POINT('Ctrl Pts',(-18.1203920742771,-4.79292130202709,
0.454672933037013));
#52492=CARTESIAN_POINT('Ctrl Pts',(-17.8817544091579,-2.97372346063237,
-3.78626344344212));
#52493=CARTESIAN_POINT('Ctrl Pts',(-17.6431167440387,1.5775160130308,-4.54865533010503));
#52494=CARTESIAN_POINT('Ctrl Pts',(-17.4044790789195,4.6794480846352,-1.13207230628853));
#52495=CARTESIAN_POINT('Ctrl Pts',(-17.1658414138002,3.48224234046452,3.3245767197852));
#52496=CARTESIAN_POINT('Ctrl Pts',(-16.927203748681,-0.914195334228,4.72684556277623));
#52497=CARTESIAN_POINT('Ctrl Pts',(-16.6885660835618,-4.47073658068798,
1.78643122161473));
#52498=CARTESIAN_POINT('Ctrl Pts',(-16.4499284184426,-3.91988901744752,
-2.79522667673945));
#52499=CARTESIAN_POINT('Ctrl Pts',(-16.2112907533233,0.232268530165553,
-4.80883285354733));
#52500=CARTESIAN_POINT('Ctrl Pts',(-15.9726530882041,4.17103458301497,-2.40443186444421));
#52501=CARTESIAN_POINT('Ctrl Pts',(-15.7340154230849,4.27775630447756,2.20898689062749));
#52502=CARTESIAN_POINT('Ctrl Pts',(-15.4953777579657,0.454385510193501,
4.79294855924697));
#52503=CARTESIAN_POINT('Ctrl Pts',(-15.2567400928464,-3.78644176495787,
2.97349640054336));
#52504=CARTESIAN_POINT('Ctrl Pts',(-15.0181024277272,-4.54856072140599,
-1.57778878407227));
#52505=CARTESIAN_POINT('Ctrl Pts',(-14.7794647626079,-1.13179168699179,
-4.67951596436188));
#52506=CARTESIAN_POINT('Ctrl Pts',(-14.5408270974888,3.32478553700414,-3.48204296590229));
#52507=CARTESIAN_POINT('Ctrl Pts',(-14.3021894323695,4.72679073178803,0.914478792178541));
#52508=CARTESIAN_POINT('Ctrl Pts',(-14.0635517672503,1.78616311715816,4.47084370140194));
#52509=CARTESIAN_POINT('Ctrl Pts',(-13.8249141021311,-2.79546173971721,
3.91972138617514));
#52510=CARTESIAN_POINT('Ctrl Pts',(-13.5862764370118,-4.80881891621556,
-0.232556905958181));
#52511=CARTESIAN_POINT('Ctrl Pts',(-13.3476387718926,-2.40418173141341,
-4.17117876454601));
#52512=CARTESIAN_POINT('Ctrl Pts',(-13.1090011067734,2.20924341525388,-4.27762382820403));
#52513=CARTESIAN_POINT('Ctrl Pts',(-12.8703634416541,4.79297579923065,-0.454098085715957));
#52514=CARTESIAN_POINT('Ctrl Pts',(-12.6317257765349,2.97326932976115,3.78662007285696));
#52515=CARTESIAN_POINT('Ctrl Pts',(-12.3930881114157,-1.57806154943975,
4.54846609634954));
#52516=CARTESIAN_POINT('Ctrl Pts',(-12.1544504462965,-4.67958382726028,
1.13151106362493));
#52517=CARTESIAN_POINT('Ctrl Pts',(-11.9158127811773,-3.48184357881804,
-3.32499434226663));
#52518=CARTESIAN_POINT('Ctrl Pts',(-11.677175116058,0.914762246840484,-4.7267358838015));
#52519=CARTESIAN_POINT('Ctrl Pts',(-11.4385374509388,4.47095080603802,-1.78589500627826));
#52520=CARTESIAN_POINT('Ctrl Pts',(-11.1998997858196,3.91955374080681,2.79569679264203));
#52521=CARTESIAN_POINT('Ctrl Pts',(-10.9612621207003,-0.232845280914501,
4.80880496159049));
#52522=CARTESIAN_POINT('Ctrl Pts',(-10.7226244555811,-4.17132293107681,
2.40393158973677));
#52523=CARTESIAN_POINT('Ctrl Pts',(-10.4839867904619,-4.27749133654748,
-2.20949993193547));
#52524=CARTESIAN_POINT('Ctrl Pts',(-10.2453491253427,-0.453810659605433,
-4.79300302197796));
#52525=CARTESIAN_POINT('Ctrl Pts',(-10.0067114602234,3.78679836713871,-2.97304224828663));
#52526=CARTESIAN_POINT('Ctrl Pts',(-9.76807379510421,4.54837145493611,1.57833430913225));
#52527=CARTESIAN_POINT('Ctrl Pts',(-9.52943612998497,1.131230436189,4.67965167333008));
#52528=CARTESIAN_POINT('Ctrl Pts',(-9.29079846486575,-3.3252031355719,3.48164417921258));
#52529=CARTESIAN_POINT('Ctrl Pts',(-9.05216079974653,-4.72668101881683,
-0.915045698212859));
#52530=CARTESIAN_POINT('Ctrl Pts',(-8.8135231346273,-1.78562688897607,-4.47105789459565));
#52531=CARTESIAN_POINT('Ctrl Pts',(-8.57488546950807,2.79593183551325,-3.91938608134342));
#52532=CARTESIAN_POINT('Ctrl Pts',(-8.33624780438884,4.80879098967182,0.233133655034067));
#52533=CARTESIAN_POINT('Ctrl Pts',(-8.09761013926962,2.40368143941586,4.17146708260569));
#52534=CARTESIAN_POINT('Ctrl Pts',(-7.85897247415039,-2.20975644067261,
4.27735882951057));
#52535=CARTESIAN_POINT('Ctrl Pts',(-7.62033480903117,-4.79303022748644,
0.453523231858677));
#52536=CARTESIAN_POINT('Ctrl Pts',(-7.38169714391193,-2.97281515612521,
-3.78697664779438));
#52537=CARTESIAN_POINT('Ctrl Pts',(-7.14305947879272,1.57860706315775,-4.5482767971816));
#52538=CARTESIAN_POINT('Ctrl Pts',(-6.90442181367349,4.6797195025539,-1.13094980465497));
#52539=CARTESIAN_POINT('Ctrl Pts',(-6.66578414855425,3.48144476711953,3.32541191686152));
#52540=CARTESIAN_POINT('Ctrl Pts',(-6.42714648343504,-0.91532914635784,
4.72662613694493));
#52541=CARTESIAN_POINT('Ctrl Pts',(-6.1885088183158,-4.47116496695316,1.78535876503999));
#52542=CARTESIAN_POINT('Ctrl Pts',(-5.94987115319659,-3.91921840801846,
-2.79616686792193));
#52543=CARTESIAN_POINT('Ctrl Pts',(-5.71123348807733,0.233422028762872,
-4.80877700124299));
#52544=CARTESIAN_POINT('Ctrl Pts',(-5.47259582295814,4.171611218274,-2.40343127894775));
#52545=CARTESIAN_POINT('Ctrl Pts',(-5.23395815783889,4.27722630874114,2.21001293857749));
#52546=CARTESIAN_POINT('Ctrl Pts',(-4.99532049271968,0.453235799314355,
4.7930574212978));
#52547=CARTESIAN_POINT('Ctrl Pts',(-4.75668282760044,-3.7871549087526,2.97258804263921));
#52548=CARTESIAN_POINT('Ctrl Pts',(-4.51804516248123,-4.54818213474018,
-1.57887979109285));
#52549=CARTESIAN_POINT('Ctrl Pts',(-4.27940749736198,-1.13066914665236,
-4.67978735413588));
#52550=CARTESIAN_POINT('Ctrl Pts',(-4.04076983224278,3.32562064318893,-3.48124526728007));
#52551=CARTESIAN_POINT('Ctrl Pts',(-3.80213216712354,4.72657132062792,0.915612446800854));
#52552=CARTESIAN_POINT('Ctrl Pts',(-3.56349450200431,1.78509047620951,4.4712723004521));
#52553=CARTESIAN_POINT('Ctrl Pts',(-3.32485683688509,-2.79640158605707,
3.91905018842691));
#52554=CARTESIAN_POINT('Ctrl Pts',(-3.08621917176585,-4.80876357952,-0.233709380055606));
#52555=CARTESIAN_POINT('Ctrl Pts',(-2.84758150664664,-2.40317998874982,
-4.17175730007125));
#52556=CARTESIAN_POINT('Ctrl Pts',(-2.60894384152741,2.21026727641583,-4.27709000786183));
#52557=CARTESIAN_POINT('Ctrl Pts',(-2.37030617640818,4.79308872923565,-0.452955592184536));
#52558=CARTESIAN_POINT('Ctrl Pts',(-2.13166851128895,2.97235298759993,3.78734702964848));
#52559=CARTESIAN_POINT('Ctrl Pts',(-1.89303084616973,-1.57913728868941,
4.54806082325786));
#52560=CARTESIAN_POINT('Ctrl Pts',(-1.6543931810505,-4.67988441526822,1.13043961063463));
#52561=CARTESIAN_POINT('Ctrl Pts',(-1.41575551593128,-3.4809896496573,-3.32592750304621));
#52562=CARTESIAN_POINT('Ctrl Pts',(-1.17711785081205,0.915788038447374,
-4.72632807804377));
#52563=CARTESIAN_POINT('Ctrl Pts',(-0.938480185692821,4.47158639354322,
-1.78518388428051));
#52564=CARTESIAN_POINT('Ctrl Pts',(-0.699842520573601,3.91848486245357,
2.79733082310517));
#52565=CARTESIAN_POINT('Ctrl Pts',(-0.461204855454373,-0.233233057815519,
4.80741524450186));
#52566=CARTESIAN_POINT('Ctrl Pts',(-0.222567190335139,-4.17338210319771,
2.40550621425186));
#52567=CARTESIAN_POINT('Ctrl Pts',(0.0160704747840829,-4.27399790357938,
-2.21560698186791));
#52568=CARTESIAN_POINT('Ctrl Pts',(0.214935195716774,-1.0951968102915,-4.35436762188871));
#52569=CARTESIAN_POINT('Ctrl Pts',(0.374026972462925,1.67656075989886,-3.8910555607899));
#52570=CARTESIAN_POINT('Ctrl Pts',(0.453572860836,2.78361000338674,-3.0463698909325));
#52571=CARTESIAN_POINT('Ctrl Pts',(0.493345805022538,3.20225585017532,-2.51287240424537));
#52572=CARTESIAN_POINT('',(4.44089209850063E-15,3.87448963569911,-3.0403873211912));
#52573=CARTESIAN_POINT('Ctrl Pts',(1.88737914186277E-15,-3.73764785372982,
-1.62671566533137));
#52574=CARTESIAN_POINT('Ctrl Pts',(2.39994637830129E-15,-3.71028158849173,
-1.71435575517499));
#52575=CARTESIAN_POINT('Ctrl Pts',(-1.76827187884598E-15,-3.67981086869404,
-1.80083539107987));
#52576=CARTESIAN_POINT('Ctrl Pts',(-3.27515792264421E-15,-3.64623269726973,
-1.88598270617316));
#52577=CARTESIAN_POINT('Ctrl Pts',(-5.28932042256129E-15,-3.60128953503947,
-1.99994929319637));
#52578=CARTESIAN_POINT('Ctrl Pts',(4.56536624768121E-15,-3.55078180752455,
-2.11152991672815));
#52579=CARTESIAN_POINT('Ctrl Pts',(6.43929354282591E-15,-3.49508775615109,
-2.22055078808827));
#52580=CARTESIAN_POINT('Ctrl Pts',(7.69212451415013E-15,-3.45785299647819,
-2.29343767356915));
#52581=CARTESIAN_POINT('Ctrl Pts',(-5.3505723180461E-15,-3.41829895641058,
-2.36518031524366));
#52582=CARTESIAN_POINT('Ctrl Pts',(-5.38458166943201E-15,-3.3765261879658,
-2.43572396492932));
#52583=CARTESIAN_POINT('Ctrl Pts',(-5.40384490325929E-15,-3.35286567774219,
-2.47568058755071));
#52584=CARTESIAN_POINT('Ctrl Pts',(-3.07309964203322E-15,-3.3284931802157,
-2.51525250052437));
#52585=CARTESIAN_POINT('Ctrl Pts',(-2.55351295663786E-15,-3.30342567080822,
-2.55442929399667));
#52586=CARTESIAN_POINT('Ctrl Pts',(-2.21585161566373E-15,-3.28713516706875,
-2.57988893141763));
#52587=CARTESIAN_POINT('Ctrl Pts',(-1.73369067459434E-14,-3.27054786797816,
-2.60518633230089));
#52588=CARTESIAN_POINT('Ctrl Pts',(-1.69309011255336E-14,-3.25368678771015,
-2.63029154815235));
#52589=CARTESIAN_POINT('Ctrl Pts',(-1.52366107287811E-14,-3.18332429778173,
-2.73505740356734));
#52590=CARTESIAN_POINT('Ctrl Pts',(-7.85431309872848E-15,-3.10815120519487,
-2.83655470454748));
#52591=CARTESIAN_POINT('Ctrl Pts',(-5.77315972805081E-15,-3.02856012624411,
-2.93460023723518));
#52592=CARTESIAN_POINT('Ctrl Pts',(-3.65120770442108E-15,-2.94740875440291,
-3.03456784146166));
#52593=CARTESIAN_POINT('Ctrl Pts',(-1.10974998716751E-14,-2.86166412082263,
-3.13094761193651));
#52594=CARTESIAN_POINT('Ctrl Pts',(-1.03805852802452E-14,-2.77169173795742,
-3.2235279094873));
#52595=CARTESIAN_POINT('Ctrl Pts',(-1.00669351464947E-14,-2.73232882045389,
-3.26403178966576));
#52596=CARTESIAN_POINT('Ctrl Pts',(1.1368289068979E-15,-2.69215607320333,
-3.30380815052698));
#52597=CARTESIAN_POINT('Ctrl Pts',(1.60982338570648E-15,-2.65120142765904,
-3.34283779060884));
#52598=CARTESIAN_POINT('Ctrl Pts',(1.85310027956541E-15,-2.63013708250599,
-3.36291204101334));
#52599=CARTESIAN_POINT('Ctrl Pts',(-2.39183766274509E-15,-2.60886587002882,
-3.38278873840918));
#52600=CARTESIAN_POINT('Ctrl Pts',(-1.77635683940025E-15,-2.58739143950339,
-3.40246515988401));
#52601=CARTESIAN_POINT('Ctrl Pts',(-1.21194577917492E-15,-2.56769885828742,
-3.42050892255673));
#52602=CARTESIAN_POINT('Ctrl Pts',(3.20395462986166E-15,-2.54783172387995,
-3.43838737529476));
#52603=CARTESIAN_POINT('Ctrl Pts',(2.72004641033163E-15,-2.52781546097606,
-3.45607868380752));
#52604=CARTESIAN_POINT('Ctrl Pts',(3.24874263539825E-16,-2.42874213786364,
-3.54364431646243));
#52605=CARTESIAN_POINT('Ctrl Pts',(-1.42112367967504E-14,-2.32592759453929,
-3.6267135247425));
#52606=CARTESIAN_POINT('Ctrl Pts',(-1.0991207943789E-14,-2.21978207787836,
-3.70509096548934));
#52607=CARTESIAN_POINT('Ctrl Pts',(-7.72550104896222E-15,-2.11213082335754,
-3.78458023727349));
#52608=CARTESIAN_POINT('Ctrl Pts',(3.10559049872635E-15,-2.00105292688667,
-3.85924433374753));
#52609=CARTESIAN_POINT('Ctrl Pts',(2.60902410786912E-15,-1.88692876195011,
-3.9288546438315));
#52610=CARTESIAN_POINT('Ctrl Pts',(2.11296027189519E-15,-1.77292009749333,
-3.99839450411882));
#52611=CARTESIAN_POINT('Ctrl Pts',(-1.19023239270618E-14,-1.65587069894074,
-4.06289140983169));
#52612=CARTESIAN_POINT('Ctrl Pts',(-1.44884104713583E-14,-1.53612127914559,
-4.12208347067618));
#52613=CARTESIAN_POINT('Ctrl Pts',(-1.63872008747819E-14,-1.44819728850264,
-4.16554424245053));
#52614=CARTESIAN_POINT('Ctrl Pts',(1.48322560200536E-15,-1.358816881025,
-4.20614452293028));
#52615=CARTESIAN_POINT('Ctrl Pts',(1.77635683940025E-15,-1.26810467560363,
-4.24376604966189));
#52616=CARTESIAN_POINT('Ctrl Pts',(1.89986052924058E-15,-1.22988530266112,
-4.25961696139028));
#52617=CARTESIAN_POINT('Ctrl Pts',(-6.83825980710587E-15,-1.19142942418558,
-4.27493893402116));
#52618=CARTESIAN_POINT('Ctrl Pts',(-6.77236045021345E-15,-1.15274600094195,
-4.28972236344086));
#52619=CARTESIAN_POINT('Ctrl Pts',(-6.73168489219131E-15,-1.1288691393026,
-4.29884725129232));
#52620=CARTESIAN_POINT('Ctrl Pts',(-6.80830697204428E-15,-1.10490022885304,
-4.30776879683175));
#52621=CARTESIAN_POINT('Ctrl Pts',(-6.55031584528842E-15,-1.08087218884353,
-4.31647376695309));
#52622=CARTESIAN_POINT('Ctrl Pts',(-5.15864969987438E-15,-0.951259165936978,
-4.36343046801116));
#52623=CARTESIAN_POINT('Ctrl Pts',(-9.14651306628698E-15,-0.819788429412977,
-4.4041447952911));
#52624=CARTESIAN_POINT('Ctrl Pts',(-7.49400541621981E-15,-0.686853690194028,
-4.43838432887677));
#52625=CARTESIAN_POINT('Ctrl Pts',(-6.41519723636329E-15,-0.600069774821131,
-4.46073695696003));
#52626=CARTESIAN_POINT('Ctrl Pts',(3.08265417366316E-15,-0.512661063187981,
-4.48032944741841));
#52627=CARTESIAN_POINT('Ctrl Pts',(2.72004641033163E-15,-0.424729285070971,
-4.49708803736938));
#52628=CARTESIAN_POINT('Ctrl Pts',(2.21027954554588E-15,-0.294380989358742,
-4.52193063336172));
#52629=CARTESIAN_POINT('Ctrl Pts',(-6.11319286711368E-15,-0.162884046650897,
-4.54054853308582));
#52630=CARTESIAN_POINT('Ctrl Pts',(-6.85562717706034E-15,-0.0306517464005833,
-4.55312130983207));
#52631=CARTESIAN_POINT('Ctrl Pts',(-7.61000109133581E-15,0.103707073763108,
-4.5658962781765));
#52632=CARTESIAN_POINT('Ctrl Pts',(-1.63497112532693E-15,0.238825822812114,
-4.57243019189283));
#52633=CARTESIAN_POINT('Ctrl Pts',(-2.63677968348475E-15,0.374285930049112,
-4.57285970409636));
#52634=CARTESIAN_POINT('Ctrl Pts',(-3.1179292879162E-15,0.439344844232451,
-4.57306599064198));
#52635=CARTESIAN_POINT('Ctrl Pts',(-1.01815445406519E-14,0.504482649963796,
-4.57186341188294));
#52636=CARTESIAN_POINT('Ctrl Pts',(-1.13242748511766E-14,0.56965339169973,
-4.56926290729125));
#52637=CARTESIAN_POINT('Ctrl Pts',(-1.17607086462203E-14,0.594543528838534,
-4.56826971749176));
#52638=CARTESIAN_POINT('Ctrl Pts',(-1.64394877692331E-14,0.619443271976647,
-4.56707223758195));
#52639=CARTESIAN_POINT('Ctrl Pts',(-1.64868119156836E-14,0.644320150574942,
-4.56567290865878));
#52640=CARTESIAN_POINT('Ctrl Pts',(-1.6747057075368E-14,0.78112319360564,
-4.55797771273081));
#52641=CARTESIAN_POINT('Ctrl Pts',(-4.80959600169574E-15,0.917388398723616,
-4.5441785389719));
#52642=CARTESIAN_POINT('Ctrl Pts',(-3.30291349825984E-15,1.05267829205595,
-4.52449336420144));
#52643=CARTESIAN_POINT('Ctrl Pts',(-1.76031124497757E-15,1.19119353586137,
-4.50433888912928));
#52644=CARTESIAN_POINT('Ctrl Pts',(-9.24810924555582E-15,1.32868716814533,
-4.47801451299053));
#52645=CARTESIAN_POINT('Ctrl Pts',(-6.0507154842071E-15,1.46470504959221,
-4.44570106748648));
#52646=CARTESIAN_POINT('Ctrl Pts',(-2.89585376704057E-15,1.59891360789184,
-4.41381745859138));
#52647=CARTESIAN_POINT('Ctrl Pts',(-2.10645447082242E-15,1.73168624049081,
-4.37610283665406));
#52648=CARTESIAN_POINT('Ctrl Pts',(-1.09634523681734E-15,1.862589475375,
-4.33268125614708));
#52649=CARTESIAN_POINT('Ctrl Pts',(-3.74816430711647E-16,1.9581841340492,
-4.30097179402927));
#52650=CARTESIAN_POINT('Ctrl Pts',(3.02205267408009E-15,2.05278195326171,
-4.26621781290806));
#52651=CARTESIAN_POINT('Ctrl Pts',(4.16333634234434E-15,2.14626801492587,
-4.22848555519344));
#52652=CARTESIAN_POINT('Ctrl Pts',(4.68860356446466E-15,2.18929427148484,
-4.21111956745068));
#52653=CARTESIAN_POINT('Ctrl Pts',(1.11734467368341E-15,2.23208498079157,
-4.19312252578931));
#52654=CARTESIAN_POINT('Ctrl Pts',(1.17961196366423E-15,2.27462862144891,
-4.17449995562647));
#52655=CARTESIAN_POINT('Ctrl Pts',(1.21298692846241E-15,2.29743180607061,
-4.16451834852861));
#52656=CARTESIAN_POINT('Ctrl Pts',(2.69478357067603E-15,2.32016400623282,
-4.15435702299221));
#52657=CARTESIAN_POINT('Ctrl Pts',(2.692290834716E-15,2.34282341818224,
-4.14401676235655));
#52658=CARTESIAN_POINT('Ctrl Pts',(2.69032939972027E-15,2.36065321014296,
-4.13588042164457));
#52659=CARTESIAN_POINT('Ctrl Pts',(-1.13007804132127E-14,2.37843876952637,
-4.12763283650539));
#52660=CARTESIAN_POINT('Ctrl Pts',(-1.09495745803656E-14,2.39616405253862,
-4.11928169694977));
#52661=CARTESIAN_POINT('Ctrl Pts',(-8.39698482786046E-15,2.52499270954159,
-4.05858500214088));
#52662=CARTESIAN_POINT('Ctrl Pts',(1.60026416366889E-15,2.6508256133944,
-3.99233766103874));
#52663=CARTESIAN_POINT('Ctrl Pts',(1.87350135405495E-15,2.77336570632561,
-3.92081240446126));
#52664=CARTESIAN_POINT('Ctrl Pts',(2.15041244287694E-15,2.89755345144912,
-3.84832543206502));
#52665=CARTESIAN_POINT('Ctrl Pts',(-2.86602714926484E-15,3.01835993446049,
-3.77041749676129));
#52666=CARTESIAN_POINT('Ctrl Pts',(-2.33146835171283E-15,3.13546816361818,
-3.68731987875136));
#52667=CARTESIAN_POINT('Ctrl Pts',(-1.79739883395837E-15,3.25246920402336,
-3.60429831970052));
#52668=CARTESIAN_POINT('Ctrl Pts',(-1.49727946848197E-15,3.3657794534396,
-3.51609628762174));
#52669=CARTESIAN_POINT('Ctrl Pts',(-1.44675937896466E-15,3.47506462955744,
-3.42289583527326));
#52670=CARTESIAN_POINT('Ctrl Pts',(-1.39690296057887E-15,3.5829141507272,
-3.33091973644948));
#52671=CARTESIAN_POINT('Ctrl Pts',(7.97356274507999E-15,3.68684428184482,
-3.23407532274603));
#52672=CARTESIAN_POINT('Ctrl Pts',(8.63198401646059E-15,3.786506317757,
-3.13249514891036));
#52673=CARTESIAN_POINT('Ctrl Pts',(8.82826822414374E-15,3.81621690671488,
-3.10221273732326));
#52674=CARTESIAN_POINT('Ctrl Pts',(4.28211893531462E-15,3.84554796150488,
-3.07150918131398));
#52675=CARTESIAN_POINT('Ctrl Pts',(4.44089209850063E-15,3.87448963569911,
-3.0403873211912));
#52676=CARTESIAN_POINT('Ctrl Pts',(4.44089209850063E-15,3.87448963569911,
-3.0403873211912));
#52677=CARTESIAN_POINT('Ctrl Pts',(-0.039772944186534,3.3679595299544,-3.68587930545212));
#52678=CARTESIAN_POINT('Ctrl Pts',(-0.0795458883730713,2.69823621289534,
-4.19688248983334));
#52679=CARTESIAN_POINT('Ctrl Pts',(-0.11931883255961,1.94417218263051,-4.52245569180505));
#52680=CARTESIAN_POINT('Ctrl Pts',(-0.159091776746148,1.19010815236569,
-4.84802889377675));
#52681=CARTESIAN_POINT('Ctrl Pts',(-0.198864720932685,0.351703408895132,
-4.98817211333893));
#52682=CARTESIAN_POINT('Ctrl Pts',(-0.238637665119224,-0.463640495906287,
-4.90908491848449));
#52683=CARTESIAN_POINT('Ctrl Pts',(-0.318183553492298,-2.09432830550906,
-4.75091052877563));
#52684=CARTESIAN_POINT('Ctrl Pts',(-0.397729441865374,-3.63277276043523,
-3.71581448140035));
#52685=CARTESIAN_POINT('Ctrl Pts',(-0.477275330238448,-4.38170539133441,
-2.26639967267857));
#52686=CARTESIAN_POINT('Ctrl Pts',(-0.515236378191096,-4.7391125194254,
-1.57470703862169));
#52687=CARTESIAN_POINT('Ctrl Pts',(-0.553197426143743,-4.91671556355819,
-0.788657102896253));
#52688=CARTESIAN_POINT('Ctrl Pts',(-0.591158474096391,-4.91617236260859,
-0.00191614214703012));
#52689=CARTESIAN_POINT('Origin',(0.5,7.95374963839832,-1.25014666726696));
#52690=CARTESIAN_POINT('',(9.,7.8971245663519,-1.27883680879202));
#52691=CARTESIAN_POINT('',(0.499999999999999,7.8971245663519,-1.27883680879202));
#52692=CARTESIAN_POINT('',(4.75,7.8971245663519,-1.27883680879202));
#52693=CARTESIAN_POINT('',(9.,7.73074086114583,-1.3631381946854));
#52694=CARTESIAN_POINT('',(9.,7.95374963839832,-1.25014666726696));
#52695=CARTESIAN_POINT('',(0.5,7.73074086114583,-1.3631381946854));
#52696=CARTESIAN_POINT('',(0.5,7.73074086114583,-1.3631381946854));
#52697=CARTESIAN_POINT('',(0.5,7.95374963839832,-1.25014666726696));
#52698=CARTESIAN_POINT('Origin',(0.5,7.82922163644705,-1.3805030124521));
#52699=CARTESIAN_POINT('',(0.499999999999999,7.85825762906118,-1.49926216363308));
#52700=CARTESIAN_POINT('Origin',(0.5,0.,0.));
#52701=CARTESIAN_POINT('',(0.5,7.73074086114583,-1.3631381946854));
#52702=CARTESIAN_POINT('Origin',(0.5,7.73074086114583,-1.3631381946854));
#52703=CARTESIAN_POINT('',(9.,7.85825762906118,-1.49926216363308));
#52704=CARTESIAN_POINT('',(4.75,7.85825762906118,-1.49926216363308));
#52705=CARTESIAN_POINT('',(9.,7.73074086114583,-1.3631381946854));
#52706=CARTESIAN_POINT('Origin',(9.,7.82922163644705,-1.3805030124521));
#52707=CARTESIAN_POINT('Origin',(9.,0.,0.));
#52708=CARTESIAN_POINT('Origin',(0.5,7.61582861882541,-2.61230826065375));
#52709=CARTESIAN_POINT('',(9.,7.55508181806639,-2.63072969389153));
#52710=CARTESIAN_POINT('',(0.499999999999999,7.55508181806639,-2.63072969389153));
#52711=CARTESIAN_POINT('',(4.75,7.55508181806639,-2.63072969389153));
#52712=CARTESIAN_POINT('',(9.,7.37658707316938,-2.6848581251065));
#52713=CARTESIAN_POINT('',(9.,7.61582861882541,-2.61230826065375));
#52714=CARTESIAN_POINT('',(0.5,7.37658707316938,-2.6848581251065));
#52715=CARTESIAN_POINT('',(0.5,7.37658707316938,-2.6848581251065));
#52716=CARTESIAN_POINT('',(0.5,7.61582861882541,-2.61230826065375));
#52717=CARTESIAN_POINT('Origin',(0.5,7.47055633524797,-2.71906013943907));
#52718=CARTESIAN_POINT('',(0.499999999999999,7.47852889570692,-2.84105711946744));
#52719=CARTESIAN_POINT('Origin',(0.5,0.,0.));
#52720=CARTESIAN_POINT('',(0.5,7.37658707316938,-2.6848581251065));
#52721=CARTESIAN_POINT('Origin',(0.5,7.37658707316938,-2.6848581251065));
#52722=CARTESIAN_POINT('',(9.,7.47852889570692,-2.84105711946744));
#52723=CARTESIAN_POINT('',(4.75,7.47852889570692,-2.84105711946744));
#52724=CARTESIAN_POINT('',(9.,7.37658707316938,-2.6848581251065));
#52725=CARTESIAN_POINT('Origin',(9.,7.47055633524797,-2.71906013943907));
#52726=CARTESIAN_POINT('Origin',(9.,0.,0.));
#52727=CARTESIAN_POINT('Origin',(0.5,7.04650450046473,-3.89509618943234));
#52728=CARTESIAN_POINT('',(9.,6.98348173179481,-3.9026891884556));
#52729=CARTESIAN_POINT('',(0.499999999999999,6.98348173179481,-3.9026891884556));
#52730=CARTESIAN_POINT('',(4.75,6.98348173179481,-3.9026891884556));
#52731=CARTESIAN_POINT('',(9.,6.79829941970784,-3.925));
#52732=CARTESIAN_POINT('',(9.,7.04650450046473,-3.89509618943234));
#52733=CARTESIAN_POINT('',(0.5,6.79829941970784,-3.925));
#52734=CARTESIAN_POINT('',(0.5,6.79829941970784,-3.925));
#52735=CARTESIAN_POINT('',(0.5,7.04650450046473,-3.89509618943234));
#52736=CARTESIAN_POINT('Origin',(0.5,6.88490196008629,-3.975));
#52737=CARTESIAN_POINT('',(0.499999999999999,6.87156884617482,-4.09652799237106));
#52738=CARTESIAN_POINT('Origin',(0.5,0.,0.));
#52739=CARTESIAN_POINT('',(0.5,6.79829941970784,-3.925));
#52740=CARTESIAN_POINT('Origin',(0.5,6.79829941970784,-3.925));
#52741=CARTESIAN_POINT('',(9.,6.87156884617482,-4.09652799237106));
#52742=CARTESIAN_POINT('',(4.75,6.87156884617482,-4.09652799237106));
#52743=CARTESIAN_POINT('',(9.,6.79829941970784,-3.925));
#52744=CARTESIAN_POINT('Origin',(9.,6.88490196008629,-3.975));
#52745=CARTESIAN_POINT('Origin',(9.,0.,0.));
#52746=CARTESIAN_POINT('Origin',(0.5,6.26307590856075,-5.0595335915088));
#52747=CARTESIAN_POINT('',(9.,6.1996920869149,-5.05606744688446));
#52748=CARTESIAN_POINT('',(0.499999999999999,6.1996920869149,-5.05606744688446));
#52749=CARTESIAN_POINT('',(4.75,6.1996920869149,-5.05606744688446));
#52750=CARTESIAN_POINT('',(9.,6.01344887848397,-5.04588273603934));
#52751=CARTESIAN_POINT('',(9.,6.26307590856075,-5.0595335915088));
#52752=CARTESIAN_POINT('',(0.5,6.01344887848397,-5.04588273603934));
#52753=CARTESIAN_POINT('',(0.5,6.01344887848397,-5.04588273603934));
#52754=CARTESIAN_POINT('',(0.5,6.26307590856075,-5.0595335915088));
#52755=CARTESIAN_POINT('Origin',(0.5,6.09005332279587,-5.11016149700799));
#52756=CARTESIAN_POINT('',(0.499999999999999,6.05581965443331,-5.22752793516966));
#52757=CARTESIAN_POINT('Origin',(0.5,0.,0.));
#52758=CARTESIAN_POINT('',(0.5,6.01344887848397,-5.04588273603934));
#52759=CARTESIAN_POINT('Origin',(0.5,6.01344887848397,-5.04588273603934));
#52760=CARTESIAN_POINT('',(9.,6.05581965443331,-5.22752793516966));
#52761=CARTESIAN_POINT('',(4.75,6.05581965443331,-5.22752793516966));
#52762=CARTESIAN_POINT('',(9.,6.01344887848397,-5.04588273603934));
#52763=CARTESIAN_POINT('Origin',(9.,6.09005332279587,-5.11016149700799));
#52764=CARTESIAN_POINT('Origin',(9.,0.,0.));
#52765=CARTESIAN_POINT('Origin',(0.5,5.28934692444449,-6.07023962565479));
#52766=CARTESIAN_POINT('',(9.,5.22752793516966,-6.05581965443332));
#52767=CARTESIAN_POINT('',(0.499999999999999,5.22752793516966,-6.05581965443332));
#52768=CARTESIAN_POINT('',(4.75,5.22752793516966,-6.05581965443332));
#52769=CARTESIAN_POINT('',(9.,5.04588273603933,-6.01344887848398));
#52770=CARTESIAN_POINT('',(9.,5.28934692444449,-6.07023962565479));
#52771=CARTESIAN_POINT('',(0.5,5.04588273603933,-6.01344887848398));
#52772=CARTESIAN_POINT('',(0.5,5.04588273603933,-6.01344887848398));
#52773=CARTESIAN_POINT('',(0.5,5.28934692444449,-6.07023962565479));
#52774=CARTESIAN_POINT('Origin',(0.5,5.11016149700799,-6.09005332279588));
#52775=CARTESIAN_POINT('',(0.499999999999999,5.05606744688446,-6.19969208691491));
#52776=CARTESIAN_POINT('Origin',(0.5,0.,0.));
#52777=CARTESIAN_POINT('',(0.5,5.04588273603933,-6.01344887848398));
#52778=CARTESIAN_POINT('Origin',(0.5,5.04588273603933,-6.01344887848398));
#52779=CARTESIAN_POINT('',(9.,5.05606744688446,-6.19969208691491));
#52780=CARTESIAN_POINT('',(4.75,5.05606744688446,-6.19969208691491));
#52781=CARTESIAN_POINT('',(9.,5.04588273603933,-6.01344887848398));
#52782=CARTESIAN_POINT('Origin',(9.,5.11016149700799,-6.09005332279588));
#52783=CARTESIAN_POINT('Origin',(9.,0.,0.));
#52784=CARTESIAN_POINT('Origin',(0.5,4.15490381056767,-6.89650450046473));
#52785=CARTESIAN_POINT('',(9.,4.09652799237105,-6.87156884617482));
#52786=CARTESIAN_POINT('',(0.499999999999999,4.09652799237105,-6.87156884617482));
#52787=CARTESIAN_POINT('',(4.75,4.09652799237105,-6.87156884617482));
#52788=CARTESIAN_POINT('',(9.,3.925,-6.79829941970784));
#52789=CARTESIAN_POINT('',(9.,4.15490381056767,-6.89650450046473));
#52790=CARTESIAN_POINT('',(0.5,3.925,-6.79829941970784));
#52791=CARTESIAN_POINT('',(0.5,3.925,-6.79829941970784));
#52792=CARTESIAN_POINT('',(0.5,4.15490381056767,-6.89650450046473));
#52793=CARTESIAN_POINT('Origin',(0.5,3.975,-6.88490196008629));
#52794=CARTESIAN_POINT('',(0.499999999999999,3.9026891884556,-6.98348173179481));
#52795=CARTESIAN_POINT('Origin',(0.5,0.,0.));
#52796=CARTESIAN_POINT('',(0.5,3.925,-6.79829941970784));
#52797=CARTESIAN_POINT('Origin',(0.5,3.925,-6.79829941970784));
#52798=CARTESIAN_POINT('',(9.,3.9026891884556,-6.98348173179481));
#52799=CARTESIAN_POINT('',(4.75,3.9026891884556,-6.98348173179481));
#52800=CARTESIAN_POINT('',(9.,3.925,-6.79829941970784));
#52801=CARTESIAN_POINT('Origin',(9.,3.975,-6.88490196008629));
#52802=CARTESIAN_POINT('Origin',(9.,0.,0.));
#52803=CARTESIAN_POINT('Origin',(0.5,2.89421604688952,-7.51322257582772));
#52804=CARTESIAN_POINT('',(9.,2.84105711946744,-7.47852889570692));
#52805=CARTESIAN_POINT('',(0.499999999999999,2.84105711946744,-7.47852889570692));
#52806=CARTESIAN_POINT('',(4.75,2.84105711946744,-7.47852889570692));
#52807=CARTESIAN_POINT('',(9.,2.6848581251065,-7.37658707316938));
#52808=CARTESIAN_POINT('',(9.,2.89421604688952,-7.51322257582772));
#52809=CARTESIAN_POINT('',(0.5,2.6848581251065,-7.37658707316938));
#52810=CARTESIAN_POINT('',(0.5,2.6848581251065,-7.37658707316938));
#52811=CARTESIAN_POINT('',(0.5,2.89421604688952,-7.51322257582772));
#52812=CARTESIAN_POINT('Origin',(0.5,2.71906013943906,-7.47055633524797));
#52813=CARTESIAN_POINT('',(0.499999999999999,2.63072969389152,-7.5550818180664));
#52814=CARTESIAN_POINT('Origin',(0.5,0.,0.));
#52815=CARTESIAN_POINT('',(0.5,2.6848581251065,-7.37658707316938));
#52816=CARTESIAN_POINT('Origin',(0.5,2.6848581251065,-7.37658707316938));
#52817=CARTESIAN_POINT('',(9.,2.63072969389152,-7.5550818180664));
#52818=CARTESIAN_POINT('',(4.75,2.63072969389152,-7.5550818180664));
#52819=CARTESIAN_POINT('',(9.,2.6848581251065,-7.37658707316938));
#52820=CARTESIAN_POINT('Origin',(9.,2.71906013943906,-7.47055633524797));
#52821=CARTESIAN_POINT('Origin',(9.,0.,0.));
#52822=CARTESIAN_POINT('Origin',(0.5,1.54558899317062,-7.90165518509824));
#52823=CARTESIAN_POINT('',(9.,1.49926216363307,-7.85825762906118));
#52824=CARTESIAN_POINT('',(0.499999999999999,1.49926216363307,-7.85825762906118));
#52825=CARTESIAN_POINT('',(4.75,1.49926216363307,-7.85825762906118));
#52826=CARTESIAN_POINT('',(9.,1.3631381946854,-7.73074086114583));
#52827=CARTESIAN_POINT('',(9.,1.54558899317062,-7.90165518509824));
#52828=CARTESIAN_POINT('',(0.5,1.3631381946854,-7.73074086114583));
#52829=CARTESIAN_POINT('',(0.5,1.3631381946854,-7.73074086114583));
#52830=CARTESIAN_POINT('',(0.5,1.54558899317062,-7.90165518509824));
#52831=CARTESIAN_POINT('Origin',(0.5,1.38050301245209,-7.82922163644705));
#52832=CARTESIAN_POINT('',(0.499999999999999,1.27883680879201,-7.8971245663519));
#52833=CARTESIAN_POINT('Origin',(0.5,0.,0.));
#52834=CARTESIAN_POINT('',(0.5,1.3631381946854,-7.73074086114583));
#52835=CARTESIAN_POINT('Origin',(0.5,1.3631381946854,-7.73074086114583));
#52836=CARTESIAN_POINT('',(9.,1.27883680879201,-7.8971245663519));
#52837=CARTESIAN_POINT('',(4.75,1.27883680879201,-7.8971245663519));
#52838=CARTESIAN_POINT('',(9.,1.3631381946854,-7.73074086114583));
#52839=CARTESIAN_POINT('Origin',(9.,1.38050301245209,-7.82922163644705));
#52840=CARTESIAN_POINT('Origin',(9.,0.,0.));
#52841=CARTESIAN_POINT('Origin',(0.5,0.149999999999999,-8.05));
#52842=CARTESIAN_POINT('',(9.,0.111912885619984,-7.99921718082665));
#52843=CARTESIAN_POINT('',(0.499999999999999,0.111912885619984,-7.99921718082665));
#52844=CARTESIAN_POINT('',(4.75,0.111912885619984,-7.99921718082665));
#52845=CARTESIAN_POINT('',(9.,-1.44202160599601E-15,-7.85));
#52846=CARTESIAN_POINT('',(9.,0.149999999999999,-8.05));
#52847=CARTESIAN_POINT('',(0.5,-1.44202160599601E-15,-7.85));
#52848=CARTESIAN_POINT('',(0.5,-1.44202160599601E-15,-7.85));
#52849=CARTESIAN_POINT('',(0.5,0.149999999999999,-8.05));
#52850=CARTESIAN_POINT('Origin',(0.5,-1.46039130798322E-15,-7.95));
#52851=CARTESIAN_POINT('',(0.499999999999999,-0.111912885619986,-7.99921718082665));
#52852=CARTESIAN_POINT('Origin',(0.5,0.,0.));
#52853=CARTESIAN_POINT('',(0.5,-1.44202160599601E-15,-7.85));
#52854=CARTESIAN_POINT('Origin',(0.5,-1.44202160599601E-15,-7.85));
#52855=CARTESIAN_POINT('',(9.,-0.111912885619986,-7.99921718082665));
#52856=CARTESIAN_POINT('',(4.75,-0.111912885619986,-7.99921718082665));
#52857=CARTESIAN_POINT('',(9.,-1.44202160599601E-15,-7.85));
#52858=CARTESIAN_POINT('Origin',(9.,-1.46039130798322E-15,-7.95));
#52859=CARTESIAN_POINT('Origin',(9.,0.,0.));
#52860=CARTESIAN_POINT('Origin',(0.5,-1.25014666726696,-7.95374963839832));
#52861=CARTESIAN_POINT('',(9.,-1.27883680879202,-7.8971245663519));
#52862=CARTESIAN_POINT('',(0.499999999999999,-1.27883680879202,-7.8971245663519));
#52863=CARTESIAN_POINT('',(4.75,-1.27883680879202,-7.8971245663519));
#52864=CARTESIAN_POINT('',(9.,-1.3631381946854,-7.73074086114583));
#52865=CARTESIAN_POINT('',(9.,-1.25014666726696,-7.95374963839832));
#52866=CARTESIAN_POINT('',(0.5,-1.3631381946854,-7.73074086114583));
#52867=CARTESIAN_POINT('',(0.5,-1.3631381946854,-7.73074086114583));
#52868=CARTESIAN_POINT('',(0.5,-1.25014666726696,-7.95374963839832));
#52869=CARTESIAN_POINT('Origin',(0.5,-1.3805030124521,-7.82922163644705));
#52870=CARTESIAN_POINT('',(0.499999999999999,-1.49926216363308,-7.85825762906118));
#52871=CARTESIAN_POINT('Origin',(0.5,0.,0.));
#52872=CARTESIAN_POINT('',(0.5,-1.3631381946854,-7.73074086114583));
#52873=CARTESIAN_POINT('Origin',(0.5,-1.3631381946854,-7.73074086114583));
#52874=CARTESIAN_POINT('',(9.,-1.49926216363308,-7.85825762906118));
#52875=CARTESIAN_POINT('',(4.75,-1.49926216363308,-7.85825762906118));
#52876=CARTESIAN_POINT('',(9.,-1.3631381946854,-7.73074086114583));
#52877=CARTESIAN_POINT('Origin',(9.,-1.3805030124521,-7.82922163644705));
#52878=CARTESIAN_POINT('Origin',(9.,0.,0.));
#52879=CARTESIAN_POINT('Origin',(0.5,-2.61230826065375,-7.61582861882541));
#52880=CARTESIAN_POINT('',(9.,-2.63072969389153,-7.55508181806639));
#52881=CARTESIAN_POINT('',(0.499999999999999,-2.63072969389153,-7.55508181806639));
#52882=CARTESIAN_POINT('',(4.75,-2.63072969389153,-7.55508181806639));
#52883=CARTESIAN_POINT('',(9.,-2.6848581251065,-7.37658707316938));
#52884=CARTESIAN_POINT('',(9.,-2.61230826065375,-7.61582861882541));
#52885=CARTESIAN_POINT('',(0.5,-2.6848581251065,-7.37658707316938));
#52886=CARTESIAN_POINT('',(0.5,-2.6848581251065,-7.37658707316938));
#52887=CARTESIAN_POINT('',(0.5,-2.61230826065375,-7.61582861882541));
#52888=CARTESIAN_POINT('Origin',(0.5,-2.71906013943907,-7.47055633524797));
#52889=CARTESIAN_POINT('',(0.499999999999999,-2.84105711946745,-7.47852889570692));
#52890=CARTESIAN_POINT('Origin',(0.5,0.,0.));
#52891=CARTESIAN_POINT('',(0.5,-2.6848581251065,-7.37658707316938));
#52892=CARTESIAN_POINT('Origin',(0.5,-2.6848581251065,-7.37658707316938));
#52893=CARTESIAN_POINT('',(9.,-2.84105711946745,-7.47852889570692));
#52894=CARTESIAN_POINT('',(4.75,-2.84105711946744,-7.47852889570692));
#52895=CARTESIAN_POINT('',(9.,-2.6848581251065,-7.37658707316938));
#52896=CARTESIAN_POINT('Origin',(9.,-2.71906013943907,-7.47055633524797));
#52897=CARTESIAN_POINT('Origin',(9.,0.,0.));
#52898=CARTESIAN_POINT('Origin',(0.5,-3.89509618943234,-7.04650450046473));
#52899=CARTESIAN_POINT('',(9.,-3.9026891884556,-6.98348173179481));
#52900=CARTESIAN_POINT('',(0.499999999999999,-3.9026891884556,-6.98348173179481));
#52901=CARTESIAN_POINT('',(4.75,-3.9026891884556,-6.98348173179481));
#52902=CARTESIAN_POINT('',(9.,-3.925,-6.79829941970784));
#52903=CARTESIAN_POINT('',(9.,-3.89509618943234,-7.04650450046473));
#52904=CARTESIAN_POINT('',(0.5,-3.925,-6.79829941970784));
#52905=CARTESIAN_POINT('',(0.5,-3.925,-6.79829941970784));
#52906=CARTESIAN_POINT('',(0.5,-3.89509618943234,-7.04650450046473));
#52907=CARTESIAN_POINT('Origin',(0.5,-3.975,-6.88490196008629));
#52908=CARTESIAN_POINT('',(0.499999999999999,-4.09652799237106,-6.87156884617482));
#52909=CARTESIAN_POINT('Origin',(0.5,0.,0.));
#52910=CARTESIAN_POINT('',(0.5,-3.925,-6.79829941970784));
#52911=CARTESIAN_POINT('Origin',(0.5,-3.925,-6.79829941970784));
#52912=CARTESIAN_POINT('',(9.,-4.09652799237106,-6.87156884617482));
#52913=CARTESIAN_POINT('',(4.75,-4.09652799237106,-6.87156884617482));
#52914=CARTESIAN_POINT('',(9.,-3.925,-6.79829941970784));
#52915=CARTESIAN_POINT('Origin',(9.,-3.975,-6.88490196008629));
#52916=CARTESIAN_POINT('Origin',(9.,0.,0.));
#52917=CARTESIAN_POINT('Origin',(0.5,-5.0595335915088,-6.26307590856075));
#52918=CARTESIAN_POINT('',(9.,-5.05606744688446,-6.1996920869149));
#52919=CARTESIAN_POINT('',(0.499999999999999,-5.05606744688446,-6.1996920869149));
#52920=CARTESIAN_POINT('',(4.75,-5.05606744688446,-6.1996920869149));
#52921=CARTESIAN_POINT('',(9.,-5.04588273603933,-6.01344887848398));
#52922=CARTESIAN_POINT('',(9.,-5.0595335915088,-6.26307590856075));
#52923=CARTESIAN_POINT('',(0.5,-5.04588273603933,-6.01344887848398));
#52924=CARTESIAN_POINT('',(0.5,-5.04588273603933,-6.01344887848398));
#52925=CARTESIAN_POINT('',(0.5,-5.0595335915088,-6.26307590856075));
#52926=CARTESIAN_POINT('Origin',(0.5,-5.11016149700799,-6.09005332279587));
#52927=CARTESIAN_POINT('',(0.499999999999999,-5.22752793516966,-6.05581965443332));
#52928=CARTESIAN_POINT('Origin',(0.5,0.,0.));
#52929=CARTESIAN_POINT('',(0.5,-5.04588273603933,-6.01344887848398));
#52930=CARTESIAN_POINT('Origin',(0.5,-5.04588273603933,-6.01344887848398));
#52931=CARTESIAN_POINT('',(9.,-5.22752793516966,-6.05581965443332));
#52932=CARTESIAN_POINT('',(4.75,-5.22752793516966,-6.05581965443332));
#52933=CARTESIAN_POINT('',(9.,-5.04588273603933,-6.01344887848398));
#52934=CARTESIAN_POINT('Origin',(9.,-5.11016149700799,-6.09005332279587));
#52935=CARTESIAN_POINT('Origin',(9.,0.,0.));
#52936=CARTESIAN_POINT('Origin',(0.5,-6.07023962565479,-5.28934692444449));
#52937=CARTESIAN_POINT('',(9.,-6.05581965443332,-5.22752793516966));
#52938=CARTESIAN_POINT('',(0.499999999999999,-6.05581965443332,-5.22752793516966));
#52939=CARTESIAN_POINT('',(4.75,-6.05581965443332,-5.22752793516966));
#52940=CARTESIAN_POINT('',(9.,-6.01344887848398,-5.04588273603933));
#52941=CARTESIAN_POINT('',(9.,-6.07023962565479,-5.28934692444449));
#52942=CARTESIAN_POINT('',(0.5,-6.01344887848398,-5.04588273603933));
#52943=CARTESIAN_POINT('',(0.5,-6.01344887848398,-5.04588273603933));
#52944=CARTESIAN_POINT('',(0.5,-6.07023962565479,-5.28934692444449));
#52945=CARTESIAN_POINT('Origin',(0.5,-6.09005332279588,-5.11016149700799));
#52946=CARTESIAN_POINT('',(0.499999999999999,-6.1996920869149,-5.05606744688446));
#52947=CARTESIAN_POINT('Origin',(0.5,0.,0.));
#52948=CARTESIAN_POINT('',(0.5,-6.01344887848398,-5.04588273603933));
#52949=CARTESIAN_POINT('Origin',(0.5,-6.01344887848398,-5.04588273603933));
#52950=CARTESIAN_POINT('',(9.,-6.1996920869149,-5.05606744688446));
#52951=CARTESIAN_POINT('',(4.75,-6.1996920869149,-5.05606744688446));
#52952=CARTESIAN_POINT('',(9.,-6.01344887848398,-5.04588273603933));
#52953=CARTESIAN_POINT('Origin',(9.,-6.09005332279588,-5.11016149700799));
#52954=CARTESIAN_POINT('Origin',(9.,0.,0.));
#52955=CARTESIAN_POINT('Origin',(0.5,-6.89650450046473,-4.15490381056766));
#52956=CARTESIAN_POINT('',(9.,-6.87156884617482,-4.09652799237105));
#52957=CARTESIAN_POINT('',(0.499999999999999,-6.87156884617482,-4.09652799237105));
#52958=CARTESIAN_POINT('',(4.75,-6.87156884617482,-4.09652799237105));
#52959=CARTESIAN_POINT('',(9.,-6.79829941970784,-3.925));
#52960=CARTESIAN_POINT('',(9.,-6.89650450046473,-4.15490381056766));
#52961=CARTESIAN_POINT('',(0.5,-6.79829941970784,-3.925));
#52962=CARTESIAN_POINT('',(0.5,-6.79829941970784,-3.925));
#52963=CARTESIAN_POINT('',(0.5,-6.89650450046473,-4.15490381056766));
#52964=CARTESIAN_POINT('Origin',(0.5,-6.88490196008629,-3.975));
#52965=CARTESIAN_POINT('',(0.499999999999999,-6.98348173179481,-3.90268918845559));
#52966=CARTESIAN_POINT('Origin',(0.5,0.,0.));
#52967=CARTESIAN_POINT('',(0.5,-6.79829941970784,-3.925));
#52968=CARTESIAN_POINT('Origin',(0.5,-6.79829941970784,-3.925));
#52969=CARTESIAN_POINT('',(9.,-6.98348173179481,-3.90268918845559));
#52970=CARTESIAN_POINT('',(4.75,-6.98348173179481,-3.90268918845559));
#52971=CARTESIAN_POINT('',(9.,-6.79829941970784,-3.925));
#52972=CARTESIAN_POINT('Origin',(9.,-6.88490196008629,-3.975));
#52973=CARTESIAN_POINT('Origin',(9.,0.,0.));
#52974=CARTESIAN_POINT('Origin',(0.5,-7.51322257582771,-2.89421604688952));
#52975=CARTESIAN_POINT('',(9.,-7.47852889570692,-2.84105711946744));
#52976=CARTESIAN_POINT('',(0.499999999999999,-7.47852889570692,-2.84105711946744));
#52977=CARTESIAN_POINT('',(4.75,-7.47852889570692,-2.84105711946744));
#52978=CARTESIAN_POINT('',(9.,-7.37658707316938,-2.6848581251065));
#52979=CARTESIAN_POINT('',(9.,-7.51322257582771,-2.89421604688952));
#52980=CARTESIAN_POINT('',(0.5,-7.37658707316938,-2.6848581251065));
#52981=CARTESIAN_POINT('',(0.5,-7.37658707316938,-2.6848581251065));
#52982=CARTESIAN_POINT('',(0.5,-7.51322257582771,-2.89421604688952));
#52983=CARTESIAN_POINT('Origin',(0.5,-7.47055633524797,-2.71906013943907));
#52984=CARTESIAN_POINT('',(0.499999999999999,-7.55508181806639,-2.63072969389152));
#52985=CARTESIAN_POINT('Origin',(0.5,0.,0.));
#52986=CARTESIAN_POINT('',(0.5,-7.37658707316938,-2.6848581251065));
#52987=CARTESIAN_POINT('Origin',(0.5,-7.37658707316938,-2.6848581251065));
#52988=CARTESIAN_POINT('',(9.,-7.55508181806639,-2.63072969389152));
#52989=CARTESIAN_POINT('',(4.75,-7.55508181806639,-2.63072969389152));
#52990=CARTESIAN_POINT('',(9.,-7.37658707316938,-2.6848581251065));
#52991=CARTESIAN_POINT('Origin',(9.,-7.47055633524797,-2.71906013943907));
#52992=CARTESIAN_POINT('Origin',(9.,0.,0.));
#52993=CARTESIAN_POINT('Origin',(0.5,-7.90165518509824,-1.54558899317062));
#52994=CARTESIAN_POINT('',(9.,-7.85825762906118,-1.49926216363307));
#52995=CARTESIAN_POINT('',(0.499999999999999,-7.85825762906118,-1.49926216363307));
#52996=CARTESIAN_POINT('',(4.75,-7.85825762906118,-1.49926216363307));
#52997=CARTESIAN_POINT('',(9.,-7.73074086114583,-1.3631381946854));
#52998=CARTESIAN_POINT('',(9.,-7.90165518509824,-1.54558899317062));
#52999=CARTESIAN_POINT('',(0.5,-7.73074086114583,-1.3631381946854));
#53000=CARTESIAN_POINT('',(0.5,-7.73074086114583,-1.3631381946854));
#53001=CARTESIAN_POINT('',(0.5,-7.90165518509824,-1.54558899317062));
#53002=CARTESIAN_POINT('Origin',(0.5,-7.82922163644705,-1.38050301245209));
#53003=CARTESIAN_POINT('',(0.499999999999999,-7.8971245663519,-1.27883680879201));
#53004=CARTESIAN_POINT('Origin',(0.5,0.,0.));
#53005=CARTESIAN_POINT('',(0.5,-7.73074086114583,-1.3631381946854));
#53006=CARTESIAN_POINT('Origin',(0.5,-7.73074086114583,-1.3631381946854));
#53007=CARTESIAN_POINT('',(9.,-7.8971245663519,-1.27883680879201));
#53008=CARTESIAN_POINT('',(4.75,-7.8971245663519,-1.27883680879201));
#53009=CARTESIAN_POINT('',(9.,-7.73074086114583,-1.3631381946854));
#53010=CARTESIAN_POINT('Origin',(9.,-7.82922163644705,-1.38050301245209));
#53011=CARTESIAN_POINT('Origin',(9.,0.,0.));
#53012=CARTESIAN_POINT('Origin',(0.5,-8.05,-0.149999999999999));
#53013=CARTESIAN_POINT('',(9.,-7.99921718082665,-0.111912885619986));
#53014=CARTESIAN_POINT('',(0.499999999999999,-7.99921718082665,-0.111912885619986));
#53015=CARTESIAN_POINT('',(4.75,-7.99921718082665,-0.111912885619986));
#53016=CARTESIAN_POINT('',(9.,-7.85,9.61347737330672E-16));
#53017=CARTESIAN_POINT('',(9.,-8.05,-0.149999999999999));
#53018=CARTESIAN_POINT('',(0.5,-7.85,9.61347737330672E-16));
#53019=CARTESIAN_POINT('',(0.5,-7.85,9.61347737330672E-16));
#53020=CARTESIAN_POINT('',(0.5,-8.05,-0.149999999999999));
#53021=CARTESIAN_POINT('Origin',(0.5,-7.95,9.73594205322146E-16));
#53022=CARTESIAN_POINT('',(0.5,-8.,-9.79717439317883E-16));
#53023=CARTESIAN_POINT('Origin',(0.5,0.,0.));
#53024=CARTESIAN_POINT('',(0.499999999999999,-7.99921718082665,0.111912885619986));
#53025=CARTESIAN_POINT('',(0.5,-7.85,9.61347737330672E-16));
#53026=CARTESIAN_POINT('Origin',(0.5,0.,0.));
#53027=CARTESIAN_POINT('Origin',(0.5,-7.85,9.61347737330672E-16));
#53028=CARTESIAN_POINT('',(9.,-7.99921718082665,0.111912885619986));
#53029=CARTESIAN_POINT('',(4.75,-7.99921718082665,0.111912885619986));
#53030=CARTESIAN_POINT('',(9.,-7.85,9.61347737330672E-16));
#53031=CARTESIAN_POINT('Origin',(9.,-7.95,9.73594205322146E-16));
#53032=CARTESIAN_POINT('',(9.,-8.,-9.79717439317883E-16));
#53033=CARTESIAN_POINT('Origin',(9.,0.,0.));
#53034=CARTESIAN_POINT('Origin',(9.,0.,0.));
#53035=CARTESIAN_POINT('Origin',(0.5,-7.95374963839832,1.25014666726696));
#53036=CARTESIAN_POINT('',(9.,-7.8971245663519,1.27883680879202));
#53037=CARTESIAN_POINT('',(0.499999999999999,-7.8971245663519,1.27883680879202));
#53038=CARTESIAN_POINT('',(4.75,-7.8971245663519,1.27883680879202));
#53039=CARTESIAN_POINT('',(9.,-7.73074086114583,1.36313819468541));
#53040=CARTESIAN_POINT('',(9.,-7.95374963839832,1.25014666726696));
#53041=CARTESIAN_POINT('',(0.5,-7.73074086114583,1.36313819468541));
#53042=CARTESIAN_POINT('',(0.5,-7.73074086114583,1.36313819468541));
#53043=CARTESIAN_POINT('',(0.5,-7.95374963839832,1.25014666726696));
#53044=CARTESIAN_POINT('Origin',(0.5,-7.82922163644705,1.3805030124521));
#53045=CARTESIAN_POINT('',(0.499999999999999,-7.85825762906118,1.49926216363308));
#53046=CARTESIAN_POINT('Origin',(0.5,0.,0.));
#53047=CARTESIAN_POINT('',(0.5,-7.73074086114583,1.36313819468541));
#53048=CARTESIAN_POINT('Origin',(0.5,-7.73074086114583,1.36313819468541));
#53049=CARTESIAN_POINT('',(9.,-7.85825762906118,1.49926216363308));
#53050=CARTESIAN_POINT('',(4.75,-7.85825762906118,1.49926216363308));
#53051=CARTESIAN_POINT('',(9.,-7.73074086114583,1.36313819468541));
#53052=CARTESIAN_POINT('Origin',(9.,-7.82922163644705,1.3805030124521));
#53053=CARTESIAN_POINT('Origin',(9.,0.,0.));
#53054=CARTESIAN_POINT('Origin',(0.5,-7.61582861882541,2.61230826065375));
#53055=CARTESIAN_POINT('',(9.,-7.55508181806639,2.63072969389153));
#53056=CARTESIAN_POINT('',(0.499999999999999,-7.55508181806639,2.63072969389153));
#53057=CARTESIAN_POINT('',(4.75,-7.55508181806639,2.63072969389153));
#53058=CARTESIAN_POINT('',(9.,-7.37658707316938,2.6848581251065));
#53059=CARTESIAN_POINT('',(9.,-7.61582861882541,2.61230826065375));
#53060=CARTESIAN_POINT('',(0.5,-7.37658707316938,2.6848581251065));
#53061=CARTESIAN_POINT('',(0.5,-7.37658707316938,2.6848581251065));
#53062=CARTESIAN_POINT('',(0.5,-7.61582861882541,2.61230826065375));
#53063=CARTESIAN_POINT('Origin',(0.5,-7.47055633524797,2.71906013943907));
#53064=CARTESIAN_POINT('',(0.499999999999999,-7.47852889570692,2.84105711946744));
#53065=CARTESIAN_POINT('Origin',(0.5,0.,0.));
#53066=CARTESIAN_POINT('',(0.5,-7.37658707316938,2.6848581251065));
#53067=CARTESIAN_POINT('Origin',(0.5,-7.37658707316938,2.6848581251065));
#53068=CARTESIAN_POINT('',(9.,-7.47852889570692,2.84105711946744));
#53069=CARTESIAN_POINT('',(4.75,-7.47852889570692,2.84105711946744));
#53070=CARTESIAN_POINT('',(9.,-7.37658707316938,2.6848581251065));
#53071=CARTESIAN_POINT('Origin',(9.,-7.47055633524797,2.71906013943907));
#53072=CARTESIAN_POINT('Origin',(9.,0.,0.));
#53073=CARTESIAN_POINT('Origin',(0.5,-7.04650450046473,3.89509618943233));
#53074=CARTESIAN_POINT('',(9.,-6.98348173179481,3.90268918845559));
#53075=CARTESIAN_POINT('',(0.499999999999999,-6.98348173179481,3.90268918845559));
#53076=CARTESIAN_POINT('',(4.75,-6.98348173179481,3.90268918845559));
#53077=CARTESIAN_POINT('',(9.,-6.79829941970784,3.925));
#53078=CARTESIAN_POINT('',(9.,-7.04650450046473,3.89509618943233));
#53079=CARTESIAN_POINT('',(0.5,-6.79829941970784,3.925));
#53080=CARTESIAN_POINT('',(0.5,-6.79829941970784,3.925));
#53081=CARTESIAN_POINT('',(0.5,-7.04650450046473,3.89509618943233));
#53082=CARTESIAN_POINT('Origin',(0.5,-6.88490196008629,3.975));
#53083=CARTESIAN_POINT('',(0.499999999999999,-6.87156884617482,4.09652799237105));
#53084=CARTESIAN_POINT('Origin',(0.5,0.,0.));
#53085=CARTESIAN_POINT('',(0.5,-6.79829941970784,3.925));
#53086=CARTESIAN_POINT('Origin',(0.5,-6.79829941970784,3.925));
#53087=CARTESIAN_POINT('',(9.,-6.87156884617482,4.09652799237105));
#53088=CARTESIAN_POINT('',(4.75,-6.87156884617482,4.09652799237105));
#53089=CARTESIAN_POINT('',(9.,-6.79829941970784,3.925));
#53090=CARTESIAN_POINT('Origin',(9.,-6.88490196008629,3.975));
#53091=CARTESIAN_POINT('Origin',(9.,0.,0.));
#53092=CARTESIAN_POINT('Origin',(0.5,-6.26307590856075,5.0595335915088));
#53093=CARTESIAN_POINT('',(9.,-6.1996920869149,5.05606744688446));
#53094=CARTESIAN_POINT('',(0.499999999999999,-6.1996920869149,5.05606744688446));
#53095=CARTESIAN_POINT('',(4.75,-6.1996920869149,5.05606744688446));
#53096=CARTESIAN_POINT('',(9.,-6.01344887848398,5.04588273603933));
#53097=CARTESIAN_POINT('',(9.,-6.26307590856075,5.0595335915088));
#53098=CARTESIAN_POINT('',(0.5,-6.01344887848398,5.04588273603933));
#53099=CARTESIAN_POINT('',(0.5,-6.01344887848398,5.04588273603933));
#53100=CARTESIAN_POINT('',(0.5,-6.26307590856075,5.0595335915088));
#53101=CARTESIAN_POINT('Origin',(0.5,-6.09005332279587,5.11016149700799));
#53102=CARTESIAN_POINT('',(0.499999999999999,-6.05581965443332,5.22752793516966));
#53103=CARTESIAN_POINT('Origin',(0.5,0.,0.));
#53104=CARTESIAN_POINT('',(0.5,-6.01344887848398,5.04588273603933));
#53105=CARTESIAN_POINT('Origin',(0.5,-6.01344887848398,5.04588273603933));
#53106=CARTESIAN_POINT('',(9.,-6.05581965443332,5.22752793516966));
#53107=CARTESIAN_POINT('',(4.75,-6.05581965443332,5.22752793516966));
#53108=CARTESIAN_POINT('',(9.,-6.01344887848398,5.04588273603933));
#53109=CARTESIAN_POINT('Origin',(9.,-6.09005332279587,5.11016149700799));
#53110=CARTESIAN_POINT('Origin',(9.,0.,0.));
#53111=CARTESIAN_POINT('Origin',(0.5,-5.28934692444449,6.07023962565479));
#53112=CARTESIAN_POINT('',(9.,-5.22752793516966,6.05581965443332));
#53113=CARTESIAN_POINT('',(0.499999999999999,-5.22752793516966,6.05581965443332));
#53114=CARTESIAN_POINT('',(4.75,-5.22752793516966,6.05581965443332));
#53115=CARTESIAN_POINT('',(9.,-5.04588273603933,6.01344887848398));
#53116=CARTESIAN_POINT('',(9.,-5.28934692444449,6.07023962565479));
#53117=CARTESIAN_POINT('',(0.5,-5.04588273603933,6.01344887848398));
#53118=CARTESIAN_POINT('',(0.5,-5.04588273603933,6.01344887848398));
#53119=CARTESIAN_POINT('',(0.5,-5.28934692444449,6.07023962565479));
#53120=CARTESIAN_POINT('Origin',(0.5,-5.11016149700799,6.09005332279587));
#53121=CARTESIAN_POINT('',(0.499999999999999,-5.05606744688446,6.1996920869149));
#53122=CARTESIAN_POINT('Origin',(0.5,0.,0.));
#53123=CARTESIAN_POINT('',(0.5,-5.04588273603933,6.01344887848398));
#53124=CARTESIAN_POINT('Origin',(0.5,-5.04588273603933,6.01344887848398));
#53125=CARTESIAN_POINT('',(9.,-5.05606744688446,6.1996920869149));
#53126=CARTESIAN_POINT('',(4.75,-5.05606744688446,6.1996920869149));
#53127=CARTESIAN_POINT('',(9.,-5.04588273603933,6.01344887848398));
#53128=CARTESIAN_POINT('Origin',(9.,-5.11016149700799,6.09005332279587));
#53129=CARTESIAN_POINT('Origin',(9.,0.,0.));
#53130=CARTESIAN_POINT('Origin',(0.5,-4.15490381056767,6.89650450046473));
#53131=CARTESIAN_POINT('',(9.,-4.09652799237105,6.87156884617482));
#53132=CARTESIAN_POINT('',(0.499999999999999,-4.09652799237105,6.87156884617482));
#53133=CARTESIAN_POINT('',(4.75,-4.09652799237105,6.87156884617482));
#53134=CARTESIAN_POINT('',(9.,-3.925,6.79829941970784));
#53135=CARTESIAN_POINT('',(9.,-4.15490381056767,6.89650450046473));
#53136=CARTESIAN_POINT('',(0.5,-3.925,6.79829941970784));
#53137=CARTESIAN_POINT('',(0.5,-3.925,6.79829941970784));
#53138=CARTESIAN_POINT('',(0.5,-4.15490381056767,6.89650450046473));
#53139=CARTESIAN_POINT('Origin',(0.5,-3.975,6.88490196008629));
#53140=CARTESIAN_POINT('',(0.499999999999999,-3.90268918845559,6.98348173179481));
#53141=CARTESIAN_POINT('Origin',(0.5,0.,0.));
#53142=CARTESIAN_POINT('',(0.5,-3.925,6.79829941970784));
#53143=CARTESIAN_POINT('Origin',(0.5,-3.925,6.79829941970784));
#53144=CARTESIAN_POINT('',(9.,-3.90268918845559,6.98348173179481));
#53145=CARTESIAN_POINT('',(4.75,-3.90268918845559,6.98348173179481));
#53146=CARTESIAN_POINT('',(9.,-3.925,6.79829941970784));
#53147=CARTESIAN_POINT('Origin',(9.,-3.975,6.88490196008629));
#53148=CARTESIAN_POINT('Origin',(9.,0.,0.));
#53149=CARTESIAN_POINT('Origin',(0.5,-2.89421604688952,7.51322257582771));
#53150=CARTESIAN_POINT('',(9.,-2.84105711946744,7.47852889570692));
#53151=CARTESIAN_POINT('',(0.499999999999999,-2.84105711946744,7.47852889570692));
#53152=CARTESIAN_POINT('',(4.75,-2.84105711946744,7.47852889570692));
#53153=CARTESIAN_POINT('',(9.,-2.6848581251065,7.37658707316938));
#53154=CARTESIAN_POINT('',(9.,-2.89421604688952,7.51322257582771));
#53155=CARTESIAN_POINT('',(0.5,-2.6848581251065,7.37658707316938));
#53156=CARTESIAN_POINT('',(0.5,-2.6848581251065,7.37658707316938));
#53157=CARTESIAN_POINT('',(0.5,-2.89421604688952,7.51322257582771));
#53158=CARTESIAN_POINT('Origin',(0.5,-2.71906013943907,7.47055633524797));
#53159=CARTESIAN_POINT('',(0.499999999999999,-2.63072969389152,7.55508181806639));
#53160=CARTESIAN_POINT('Origin',(0.5,0.,0.));
#53161=CARTESIAN_POINT('',(0.5,-2.6848581251065,7.37658707316938));
#53162=CARTESIAN_POINT('Origin',(0.5,-2.6848581251065,7.37658707316938));
#53163=CARTESIAN_POINT('',(9.,-2.63072969389152,7.55508181806639));
#53164=CARTESIAN_POINT('',(4.75,-2.63072969389152,7.55508181806639));
#53165=CARTESIAN_POINT('',(9.,-2.6848581251065,7.37658707316938));
#53166=CARTESIAN_POINT('Origin',(9.,-2.71906013943907,7.47055633524797));
#53167=CARTESIAN_POINT('Origin',(9.,0.,0.));
#53168=CARTESIAN_POINT('Origin',(0.5,-1.54558899317062,7.90165518509824));
#53169=CARTESIAN_POINT('',(9.,-1.49926216363308,7.85825762906118));
#53170=CARTESIAN_POINT('',(0.499999999999999,-1.49926216363308,7.85825762906118));
#53171=CARTESIAN_POINT('',(4.75,-1.49926216363308,7.85825762906118));
#53172=CARTESIAN_POINT('',(9.,-1.3631381946854,7.73074086114583));
#53173=CARTESIAN_POINT('',(9.,-1.54558899317062,7.90165518509824));
#53174=CARTESIAN_POINT('',(0.5,-1.3631381946854,7.73074086114583));
#53175=CARTESIAN_POINT('',(0.5,-1.3631381946854,7.73074086114583));
#53176=CARTESIAN_POINT('',(0.5,-1.54558899317062,7.90165518509824));
#53177=CARTESIAN_POINT('Origin',(0.5,-1.3805030124521,7.82922163644705));
#53178=CARTESIAN_POINT('',(0.499999999999999,-1.27883680879202,7.8971245663519));
#53179=CARTESIAN_POINT('Origin',(0.5,0.,0.));
#53180=CARTESIAN_POINT('',(0.5,-1.3631381946854,7.73074086114583));
#53181=CARTESIAN_POINT('Origin',(0.5,-1.3631381946854,7.73074086114583));
#53182=CARTESIAN_POINT('',(9.,-1.27883680879202,7.8971245663519));
#53183=CARTESIAN_POINT('',(4.75,-1.27883680879202,7.8971245663519));
#53184=CARTESIAN_POINT('',(9.,-1.3631381946854,7.73074086114583));
#53185=CARTESIAN_POINT('Origin',(9.,-1.3805030124521,7.82922163644705));
#53186=CARTESIAN_POINT('Origin',(9.,0.,0.));
#53187=CARTESIAN_POINT('Origin',(0.5,-0.15,8.05));
#53188=CARTESIAN_POINT('',(9.,-0.111912885619985,7.99921718082665));
#53189=CARTESIAN_POINT('',(0.499999999999999,-0.111912885619985,7.99921718082665));
#53190=CARTESIAN_POINT('',(4.75,-0.111912885619985,7.99921718082665));
#53191=CARTESIAN_POINT('',(9.,4.80673868665336E-16,7.85));
#53192=CARTESIAN_POINT('',(9.,-0.15,8.05));
#53193=CARTESIAN_POINT('',(0.5,4.80673868665336E-16,7.85));
#53194=CARTESIAN_POINT('',(0.5,4.80673868665336E-16,7.85));
#53195=CARTESIAN_POINT('',(0.5,-0.15,8.05));
#53196=CARTESIAN_POINT('Origin',(0.5,4.86797102661073E-16,7.95));
#53197=CARTESIAN_POINT('',(0.499999999999999,0.111912885619987,7.99921718082665));
#53198=CARTESIAN_POINT('Origin',(0.5,0.,0.));
#53199=CARTESIAN_POINT('',(0.5,4.80673868665336E-16,7.85));
#53200=CARTESIAN_POINT('Origin',(0.5,4.80673868665336E-16,7.85));
#53201=CARTESIAN_POINT('',(9.,0.111912885619987,7.99921718082665));
#53202=CARTESIAN_POINT('',(4.75,0.111912885619987,7.99921718082665));
#53203=CARTESIAN_POINT('',(9.,4.80673868665336E-16,7.85));
#53204=CARTESIAN_POINT('Origin',(9.,4.86797102661073E-16,7.95));
#53205=CARTESIAN_POINT('Origin',(9.,0.,0.));
#53206=CARTESIAN_POINT('Origin',(0.5,1.25014666726696,7.95374963839832));
#53207=CARTESIAN_POINT('',(9.,1.27883680879202,7.8971245663519));
#53208=CARTESIAN_POINT('',(0.499999999999999,1.27883680879202,7.8971245663519));
#53209=CARTESIAN_POINT('',(4.75,1.27883680879202,7.8971245663519));
#53210=CARTESIAN_POINT('',(9.,1.3631381946854,7.73074086114583));
#53211=CARTESIAN_POINT('',(9.,1.25014666726696,7.95374963839832));
#53212=CARTESIAN_POINT('',(0.5,1.3631381946854,7.73074086114583));
#53213=CARTESIAN_POINT('',(0.5,1.3631381946854,7.73074086114583));
#53214=CARTESIAN_POINT('',(0.5,1.25014666726696,7.95374963839832));
#53215=CARTESIAN_POINT('Origin',(0.5,1.3805030124521,7.82922163644705));
#53216=CARTESIAN_POINT('',(0.499999999999999,1.49926216363308,7.85825762906118));
#53217=CARTESIAN_POINT('Origin',(0.5,0.,0.));
#53218=CARTESIAN_POINT('',(0.5,1.3631381946854,7.73074086114583));
#53219=CARTESIAN_POINT('Origin',(0.5,1.3631381946854,7.73074086114583));
#53220=CARTESIAN_POINT('',(9.,1.49926216363308,7.85825762906118));
#53221=CARTESIAN_POINT('',(4.75,1.49926216363308,7.85825762906118));
#53222=CARTESIAN_POINT('',(9.,1.3631381946854,7.73074086114583));
#53223=CARTESIAN_POINT('Origin',(9.,1.3805030124521,7.82922163644705));
#53224=CARTESIAN_POINT('Origin',(9.,0.,0.));
#53225=CARTESIAN_POINT('Origin',(0.5,2.61230826065375,7.61582861882541));
#53226=CARTESIAN_POINT('',(9.,2.63072969389153,7.55508181806639));
#53227=CARTESIAN_POINT('',(0.499999999999999,2.63072969389153,7.55508181806639));
#53228=CARTESIAN_POINT('',(4.75,2.63072969389153,7.55508181806639));
#53229=CARTESIAN_POINT('',(9.,2.6848581251065,7.37658707316938));
#53230=CARTESIAN_POINT('',(9.,2.61230826065375,7.61582861882541));
#53231=CARTESIAN_POINT('',(0.5,2.6848581251065,7.37658707316938));
#53232=CARTESIAN_POINT('',(0.5,2.6848581251065,7.37658707316938));
#53233=CARTESIAN_POINT('',(0.5,2.61230826065375,7.61582861882541));
#53234=CARTESIAN_POINT('Origin',(0.5,2.71906013943907,7.47055633524797));
#53235=CARTESIAN_POINT('',(0.499999999999999,2.84105711946744,7.47852889570692));
#53236=CARTESIAN_POINT('Origin',(0.5,0.,0.));
#53237=CARTESIAN_POINT('',(0.5,2.6848581251065,7.37658707316938));
#53238=CARTESIAN_POINT('Origin',(0.5,2.6848581251065,7.37658707316938));
#53239=CARTESIAN_POINT('',(9.,2.84105711946744,7.47852889570692));
#53240=CARTESIAN_POINT('',(4.75,2.84105711946744,7.47852889570692));
#53241=CARTESIAN_POINT('',(9.,2.6848581251065,7.37658707316938));
#53242=CARTESIAN_POINT('Origin',(9.,2.71906013943907,7.47055633524797));
#53243=CARTESIAN_POINT('Origin',(9.,0.,0.));
#53244=CARTESIAN_POINT('Origin',(0.5,3.89509618943234,7.04650450046473));
#53245=CARTESIAN_POINT('',(9.,3.9026891884556,6.98348173179481));
#53246=CARTESIAN_POINT('',(0.499999999999999,3.9026891884556,6.98348173179481));
#53247=CARTESIAN_POINT('',(4.75,3.9026891884556,6.98348173179481));
#53248=CARTESIAN_POINT('',(9.,3.925,6.79829941970784));
#53249=CARTESIAN_POINT('',(9.,3.89509618943234,7.04650450046473));
#53250=CARTESIAN_POINT('',(0.5,3.925,6.79829941970784));
#53251=CARTESIAN_POINT('',(0.5,3.925,6.79829941970784));
#53252=CARTESIAN_POINT('',(0.5,3.89509618943234,7.04650450046473));
#53253=CARTESIAN_POINT('Origin',(0.5,3.975,6.88490196008629));
#53254=CARTESIAN_POINT('',(0.499999999999999,4.09652799237105,6.87156884617482));
#53255=CARTESIAN_POINT('Origin',(0.5,0.,0.));
#53256=CARTESIAN_POINT('',(0.5,3.925,6.79829941970784));
#53257=CARTESIAN_POINT('Origin',(0.5,3.925,6.79829941970784));
#53258=CARTESIAN_POINT('',(9.,4.09652799237105,6.87156884617482));
#53259=CARTESIAN_POINT('',(4.75,4.09652799237105,6.87156884617482));
#53260=CARTESIAN_POINT('',(9.,3.925,6.79829941970784));
#53261=CARTESIAN_POINT('Origin',(9.,3.975,6.88490196008629));
#53262=CARTESIAN_POINT('Origin',(9.,0.,0.));
#53263=CARTESIAN_POINT('Origin',(0.5,5.0595335915088,6.26307590856075));
#53264=CARTESIAN_POINT('',(9.,5.05606744688446,6.1996920869149));
#53265=CARTESIAN_POINT('',(0.499999999999999,5.05606744688446,6.1996920869149));
#53266=CARTESIAN_POINT('',(4.75,5.05606744688446,6.1996920869149));
#53267=CARTESIAN_POINT('',(9.,5.04588273603933,6.01344887848398));
#53268=CARTESIAN_POINT('',(9.,5.0595335915088,6.26307590856075));
#53269=CARTESIAN_POINT('',(0.5,5.04588273603933,6.01344887848398));
#53270=CARTESIAN_POINT('',(0.5,5.04588273603933,6.01344887848398));
#53271=CARTESIAN_POINT('',(0.5,5.0595335915088,6.26307590856075));
#53272=CARTESIAN_POINT('Origin',(0.5,5.11016149700799,6.09005332279587));
#53273=CARTESIAN_POINT('',(0.499999999999999,5.22752793516966,6.05581965443332));
#53274=CARTESIAN_POINT('Origin',(0.5,0.,0.));
#53275=CARTESIAN_POINT('',(0.5,5.04588273603933,6.01344887848398));
#53276=CARTESIAN_POINT('Origin',(0.5,5.04588273603933,6.01344887848398));
#53277=CARTESIAN_POINT('',(9.,5.22752793516966,6.05581965443332));
#53278=CARTESIAN_POINT('',(4.75,5.22752793516966,6.05581965443332));
#53279=CARTESIAN_POINT('',(9.,5.04588273603933,6.01344887848398));
#53280=CARTESIAN_POINT('Origin',(9.,5.11016149700799,6.09005332279587));
#53281=CARTESIAN_POINT('Origin',(9.,0.,0.));
#53282=CARTESIAN_POINT('Origin',(0.5,6.07023962565479,5.28934692444449));
#53283=CARTESIAN_POINT('',(9.,6.05581965443332,5.22752793516966));
#53284=CARTESIAN_POINT('',(0.499999999999999,6.05581965443332,5.22752793516966));
#53285=CARTESIAN_POINT('',(4.75,6.05581965443332,5.22752793516966));
#53286=CARTESIAN_POINT('',(9.,6.01344887848398,5.04588273603933));
#53287=CARTESIAN_POINT('',(9.,6.07023962565479,5.28934692444449));
#53288=CARTESIAN_POINT('',(0.5,6.01344887848398,5.04588273603933));
#53289=CARTESIAN_POINT('',(0.5,6.01344887848398,5.04588273603933));
#53290=CARTESIAN_POINT('',(0.5,6.07023962565479,5.28934692444449));
#53291=CARTESIAN_POINT('Origin',(0.5,6.09005332279588,5.11016149700799));
#53292=CARTESIAN_POINT('',(0.499999999999999,6.1996920869149,5.05606744688446));
#53293=CARTESIAN_POINT('Origin',(0.5,0.,0.));
#53294=CARTESIAN_POINT('',(0.5,6.01344887848398,5.04588273603933));
#53295=CARTESIAN_POINT('Origin',(0.5,6.01344887848398,5.04588273603933));
#53296=CARTESIAN_POINT('',(9.,6.1996920869149,5.05606744688446));
#53297=CARTESIAN_POINT('',(4.75,6.1996920869149,5.05606744688446));
#53298=CARTESIAN_POINT('',(9.,6.01344887848398,5.04588273603933));
#53299=CARTESIAN_POINT('Origin',(9.,6.09005332279588,5.11016149700799));
#53300=CARTESIAN_POINT('Origin',(9.,0.,0.));
#53301=CARTESIAN_POINT('Origin',(0.5,6.89650450046473,4.15490381056767));
#53302=CARTESIAN_POINT('',(9.,6.87156884617482,4.09652799237105));
#53303=CARTESIAN_POINT('',(0.499999999999999,6.87156884617482,4.09652799237105));
#53304=CARTESIAN_POINT('',(4.75,6.87156884617482,4.09652799237105));
#53305=CARTESIAN_POINT('',(9.,6.79829941970784,3.925));
#53306=CARTESIAN_POINT('',(9.,6.89650450046473,4.15490381056767));
#53307=CARTESIAN_POINT('',(0.5,6.79829941970784,3.925));
#53308=CARTESIAN_POINT('',(0.5,6.79829941970784,3.925));
#53309=CARTESIAN_POINT('',(0.5,6.89650450046473,4.15490381056767));
#53310=CARTESIAN_POINT('Origin',(0.5,6.88490196008629,3.975));
#53311=CARTESIAN_POINT('',(0.499999999999999,6.98348173179481,3.90268918845559));
#53312=CARTESIAN_POINT('Origin',(0.5,0.,0.));
#53313=CARTESIAN_POINT('',(0.5,6.79829941970784,3.925));
#53314=CARTESIAN_POINT('Origin',(0.5,6.79829941970784,3.925));
#53315=CARTESIAN_POINT('',(9.,6.98348173179481,3.90268918845559));
#53316=CARTESIAN_POINT('',(4.75,6.98348173179481,3.90268918845559));
#53317=CARTESIAN_POINT('',(9.,6.79829941970784,3.925));
#53318=CARTESIAN_POINT('Origin',(9.,6.88490196008629,3.975));
#53319=CARTESIAN_POINT('Origin',(9.,0.,0.));
#53320=CARTESIAN_POINT('Origin',(0.5,7.51322257582771,2.89421604688952));
#53321=CARTESIAN_POINT('',(9.,7.47852889570692,2.84105711946744));
#53322=CARTESIAN_POINT('',(0.499999999999999,7.47852889570692,2.84105711946744));
#53323=CARTESIAN_POINT('',(4.75,7.47852889570692,2.84105711946744));
#53324=CARTESIAN_POINT('',(9.,7.37658707316938,2.6848581251065));
#53325=CARTESIAN_POINT('',(9.,7.51322257582771,2.89421604688952));
#53326=CARTESIAN_POINT('',(0.5,7.37658707316938,2.6848581251065));
#53327=CARTESIAN_POINT('',(0.5,7.37658707316938,2.6848581251065));
#53328=CARTESIAN_POINT('',(0.5,7.51322257582771,2.89421604688952));
#53329=CARTESIAN_POINT('Origin',(0.5,7.47055633524797,2.71906013943907));
#53330=CARTESIAN_POINT('',(0.499999999999999,7.55508181806639,2.63072969389152));
#53331=CARTESIAN_POINT('Origin',(0.5,0.,0.));
#53332=CARTESIAN_POINT('',(0.5,7.37658707316938,2.6848581251065));
#53333=CARTESIAN_POINT('Origin',(0.5,7.37658707316938,2.6848581251065));
#53334=CARTESIAN_POINT('',(9.,7.55508181806639,2.63072969389152));
#53335=CARTESIAN_POINT('',(4.75,7.55508181806639,2.63072969389152));
#53336=CARTESIAN_POINT('',(9.,7.37658707316938,2.6848581251065));
#53337=CARTESIAN_POINT('Origin',(9.,7.47055633524797,2.71906013943907));
#53338=CARTESIAN_POINT('Origin',(9.,0.,0.));
#53339=CARTESIAN_POINT('Origin',(0.5,7.90165518509824,1.54558899317062));
#53340=CARTESIAN_POINT('',(9.,7.85825762906118,1.49926216363308));
#53341=CARTESIAN_POINT('',(0.499999999999999,7.85825762906118,1.49926216363308));
#53342=CARTESIAN_POINT('',(4.75,7.85825762906118,1.49926216363308));
#53343=CARTESIAN_POINT('',(9.,7.73074086114583,1.3631381946854));
#53344=CARTESIAN_POINT('',(9.,7.90165518509824,1.54558899317062));
#53345=CARTESIAN_POINT('',(0.5,7.73074086114583,1.3631381946854));
#53346=CARTESIAN_POINT('',(0.5,7.73074086114583,1.3631381946854));
#53347=CARTESIAN_POINT('',(0.5,7.90165518509824,1.54558899317062));
#53348=CARTESIAN_POINT('Origin',(0.5,7.82922163644705,1.3805030124521));
#53349=CARTESIAN_POINT('',(0.499999999999999,7.8971245663519,1.27883680879202));
#53350=CARTESIAN_POINT('Origin',(0.5,0.,0.));
#53351=CARTESIAN_POINT('',(0.5,7.73074086114583,1.3631381946854));
#53352=CARTESIAN_POINT('Origin',(0.5,7.73074086114583,1.3631381946854));
#53353=CARTESIAN_POINT('',(9.,7.8971245663519,1.27883680879202));
#53354=CARTESIAN_POINT('',(4.75,7.8971245663519,1.27883680879202));
#53355=CARTESIAN_POINT('',(9.,7.73074086114583,1.3631381946854));
#53356=CARTESIAN_POINT('Origin',(9.,7.82922163644705,1.3805030124521));
#53357=CARTESIAN_POINT('Origin',(9.,0.,0.));
#53358=CARTESIAN_POINT('Origin',(0.5,8.05,0.15));
#53359=CARTESIAN_POINT('',(9.,7.99921718082665,0.111912885619985));
#53360=CARTESIAN_POINT('',(0.499999999999999,7.99921718082665,0.111912885619985));
#53361=CARTESIAN_POINT('',(4.75,7.99921718082665,0.111912885619985));
#53362=CARTESIAN_POINT('',(9.,7.85,0.));
#53363=CARTESIAN_POINT('',(9.,8.05,0.15));
#53364=CARTESIAN_POINT('',(0.5,7.85,0.));
#53365=CARTESIAN_POINT('',(0.5,7.85,0.));
#53366=CARTESIAN_POINT('',(0.5,8.05,0.15));
#53367=CARTESIAN_POINT('Origin',(0.5,7.95,0.));
#53368=CARTESIAN_POINT('',(0.499999999999999,7.99921718082665,-0.111912885619987));
#53369=CARTESIAN_POINT('Origin',(0.5,0.,0.));
#53370=CARTESIAN_POINT('',(0.5,7.85,0.));
#53371=CARTESIAN_POINT('Origin',(0.5,7.85,0.));
#53372=CARTESIAN_POINT('',(9.,7.99921718082665,-0.111912885619987));
#53373=CARTESIAN_POINT('',(4.75,7.99921718082665,-0.111912885619987));
#53374=CARTESIAN_POINT('',(9.,7.85,0.));
#53375=CARTESIAN_POINT('Origin',(9.,7.95,0.));
#53376=CARTESIAN_POINT('Origin',(9.,0.,0.));
#53377=CARTESIAN_POINT('Origin',(10.,5.55111512312578E-16,4.61880215351701));
#53378=CARTESIAN_POINT('',(10.,2.82820063659975E-16,4.61880215351701));
#53379=CARTESIAN_POINT('',(10.,4.,2.3094010767585));
#53380=CARTESIAN_POINT('',(10.,1.,4.04145188432738));
#53381=CARTESIAN_POINT('',(5.,5.55111512312578E-16,4.61880215351701));
#53382=CARTESIAN_POINT('',(10.,2.82820063659975E-16,4.61880215351701));
#53383=CARTESIAN_POINT('',(5.,4.,2.3094010767585));
#53384=CARTESIAN_POINT('',(5.,4.,2.3094010767585));
#53385=CARTESIAN_POINT('',(10.,4.,2.3094010767585));
#53386=CARTESIAN_POINT('Origin',(10.,-4.,2.3094010767585));
#53387=CARTESIAN_POINT('',(10.,-4.,2.3094010767585));
#53388=CARTESIAN_POINT('',(10.,-3.,2.88675134594813));
#53389=CARTESIAN_POINT('',(5.,-4.,2.3094010767585));
#53390=CARTESIAN_POINT('',(10.,-4.,2.3094010767585));
#53391=CARTESIAN_POINT('',(5.,2.82820063659975E-16,4.61880215351701));
#53392=CARTESIAN_POINT('Origin',(10.,-4.,-2.3094010767585));
#53393=CARTESIAN_POINT('',(10.,-4.,-2.3094010767585));
#53394=CARTESIAN_POINT('',(10.,-4.,-1.15470053837925));
#53395=CARTESIAN_POINT('',(5.,-4.,-2.3094010767585));
#53396=CARTESIAN_POINT('',(10.,-4.,-2.3094010767585));
#53397=CARTESIAN_POINT('',(5.,-4.,2.3094010767585));
#53398=CARTESIAN_POINT('Origin',(10.,-1.11022302462516E-15,-4.61880215351701));
#53399=CARTESIAN_POINT('',(10.,-8.48460190979926E-16,-4.61880215351701));
#53400=CARTESIAN_POINT('',(10.,-1.,-4.04145188432738));
#53401=CARTESIAN_POINT('',(5.,-1.11022302462516E-15,-4.61880215351701));
#53402=CARTESIAN_POINT('',(10.,-8.48460190979926E-16,-4.61880215351701));
#53403=CARTESIAN_POINT('',(5.,-4.,-2.3094010767585));
#53404=CARTESIAN_POINT('Origin',(10.,4.,-2.30940107675851));
#53405=CARTESIAN_POINT('',(10.,4.,-2.30940107675851));
#53406=CARTESIAN_POINT('',(10.,3.,-2.88675134594813));
#53407=CARTESIAN_POINT('',(5.,4.,-2.30940107675851));
#53408=CARTESIAN_POINT('',(10.,4.,-2.30940107675851));
#53409=CARTESIAN_POINT('',(5.,-8.48460190979926E-16,-4.61880215351701));
#53410=CARTESIAN_POINT('Origin',(10.,4.,2.3094010767585));
#53411=CARTESIAN_POINT('',(10.,4.,1.15470053837925));
#53412=CARTESIAN_POINT('',(5.,4.,-2.30940107675851));
#53413=CARTESIAN_POINT('Origin',(5.,0.,0.));
#53414=CARTESIAN_POINT('Origin',(-30.,4.5,0.));
#53415=CARTESIAN_POINT('',(-30.,-4.5,-5.51091059616309E-16));
#53416=CARTESIAN_POINT('Origin',(-30.,0.,0.));
#53417=CARTESIAN_POINT('Origin',(-29.75,0.,0.));
#53418=CARTESIAN_POINT('',(-29.75,-4.75,-5.81707229594993E-16));
#53419=CARTESIAN_POINT('Origin',(-14.75,0.,0.));
#53420=CARTESIAN_POINT('Origin',(0.,0.,0.));
#53421=CARTESIAN_POINT('Origin',(0.,8.,0.));
#53422=CARTESIAN_POINT('',(5.55111512312578E-16,-8.,-9.79717439317883E-16));
#53423=CARTESIAN_POINT('Origin',(0.,0.,0.));
#53424=CARTESIAN_POINT('Origin',(4.75,0.,0.));
#53425=CARTESIAN_POINT('',(9.5,-8.,-9.79717439317883E-16));
#53426=CARTESIAN_POINT('Origin',(9.5,0.,0.));
#53427=CARTESIAN_POINT('',(4.75,-8.,-9.79717439317883E-16));
#53428=CARTESIAN_POINT('',(4.75,-8.,-9.79717439317883E-16));
#53429=CARTESIAN_POINT('Origin',(9.75,0.,0.));
#53430=CARTESIAN_POINT('',(10.,-7.5,-9.18485099360515E-16));
#53431=CARTESIAN_POINT('Origin',(10.,0.,0.));
#53432=CARTESIAN_POINT('',(9.75,-7.75,-9.49101269339199E-16));
#53433=CARTESIAN_POINT('Origin',(10.,0.,0.));
#53434=CARTESIAN_POINT('',(0.,0.,0.));
#53435=CARTESIAN_POINT('Origin',(5.5,-7.,3.54145188432738));
#53436=CARTESIAN_POINT('',(5.5,-6.56698729810778,4.29145188432738));
#53437=CARTESIAN_POINT('',(6.,-6.5,3.75277674973257));
#53438=CARTESIAN_POINT('',(5.5,-6.56698729810778,4.29145188432738));
#53439=CARTESIAN_POINT('',(5.5,-7.,3.54145188432738));
#53440=CARTESIAN_POINT('',(5.5,-7.,3.54145188432738));
#53441=CARTESIAN_POINT('',(6.,-6.5,3.75277674973257));
#53442=CARTESIAN_POINT('Origin',(0.,-6.78349364905389,3.91645188432738));
#53443=CARTESIAN_POINT('',(0.,-6.56698729810778,4.29145188432738));
#53444=CARTESIAN_POINT('',(0.,-7.,3.54145188432738));
#53445=CARTESIAN_POINT('',(0.,-6.78349364905389,3.91645188432738));
#53446=CARTESIAN_POINT('',(0.,-7.,3.54145188432738));
#53447=CARTESIAN_POINT('',(0.,-6.56698729810778,4.29145188432738));
#53448=CARTESIAN_POINT('Origin',(5.5,-0.433012701892218,7.83290376865476));
#53449=CARTESIAN_POINT('',(5.5,0.43301270189222,7.83290376865476));
#53450=CARTESIAN_POINT('',(6.,5.55111512312578E-16,7.50555349946513));
#53451=CARTESIAN_POINT('',(5.5,0.43301270189222,7.83290376865476));
#53452=CARTESIAN_POINT('',(5.5,-0.433012701892219,7.83290376865476));
#53453=CARTESIAN_POINT('',(5.5,-0.433012701892218,7.83290376865476));
#53454=CARTESIAN_POINT('',(6.,0.,7.50555349946513));
#53455=CARTESIAN_POINT('Origin',(0.,9.0205620750794E-16,7.83290376865476));
#53456=CARTESIAN_POINT('',(0.,0.43301270189222,7.83290376865476));
#53457=CARTESIAN_POINT('',(0.,-0.433012701892219,7.83290376865476));
#53458=CARTESIAN_POINT('',(0.,4.5102810375397E-16,7.83290376865476));
#53459=CARTESIAN_POINT('',(0.,-0.433012701892218,7.83290376865476));
#53460=CARTESIAN_POINT('',(0.,0.43301270189222,7.83290376865476));
#53461=CARTESIAN_POINT('Origin',(5.75,-1.625,6.85603444662681));
#53462=CARTESIAN_POINT('',(6.,-1.5,6.6395280956807));
#53463=CARTESIAN_POINT('',(5.5,-1.75,7.07254079757292));
#53464=CARTESIAN_POINT('Origin',(5.5,-6.56698729810778,-4.29145188432738));
#53465=CARTESIAN_POINT('',(5.5,-7.,-3.54145188432738));
#53466=CARTESIAN_POINT('',(6.,-6.5,-3.75277674973257));
#53467=CARTESIAN_POINT('',(5.5,-7.,-3.54145188432738));
#53468=CARTESIAN_POINT('',(5.5,-6.56698729810778,-4.29145188432738));
#53469=CARTESIAN_POINT('',(5.5,-6.56698729810778,-4.29145188432738));
#53470=CARTESIAN_POINT('',(6.,-6.5,-3.75277674973257));
#53471=CARTESIAN_POINT('Origin',(0.,-6.78349364905389,-3.91645188432738));
#53472=CARTESIAN_POINT('',(0.,-7.,-3.54145188432738));
#53473=CARTESIAN_POINT('',(0.,-6.56698729810778,-4.29145188432738));
#53474=CARTESIAN_POINT('',(0.,-6.78349364905389,-3.91645188432738));
#53475=CARTESIAN_POINT('',(0.,-6.56698729810778,-4.29145188432738));
#53476=CARTESIAN_POINT('',(0.,-7.,-3.54145188432738));
#53477=CARTESIAN_POINT('Origin',(5.5,6.56698729810778,4.29145188432738));
#53478=CARTESIAN_POINT('',(5.5,7.,3.54145188432738));
#53479=CARTESIAN_POINT('',(6.,6.5,3.75277674973257));
#53480=CARTESIAN_POINT('',(5.5,7.,3.54145188432738));
#53481=CARTESIAN_POINT('',(5.5,6.56698729810778,4.29145188432738));
#53482=CARTESIAN_POINT('',(5.5,6.56698729810778,4.29145188432738));
#53483=CARTESIAN_POINT('',(6.,6.5,3.75277674973257));
#53484=CARTESIAN_POINT('Origin',(0.,6.78349364905389,3.91645188432738));
#53485=CARTESIAN_POINT('',(0.,7.,3.54145188432738));
#53486=CARTESIAN_POINT('',(0.,6.56698729810778,4.29145188432738));
#53487=CARTESIAN_POINT('',(0.,6.78349364905389,3.91645188432738));
#53488=CARTESIAN_POINT('',(0.,6.56698729810778,4.29145188432738));
#53489=CARTESIAN_POINT('',(0.,7.,3.54145188432738));
#53490=CARTESIAN_POINT('Origin',(5.75,5.125,4.83530850446312));
#53491=CARTESIAN_POINT('',(6.,5.,4.61880215351701));
#53492=CARTESIAN_POINT('',(5.5,5.25,5.05181485540922));
#53493=CARTESIAN_POINT('Origin',(5.5,0.433012701892218,-7.83290376865476));
#53494=CARTESIAN_POINT('',(5.5,-0.433012701892222,-7.83290376865476));
#53495=CARTESIAN_POINT('',(6.,0.,-7.50555349946514));
#53496=CARTESIAN_POINT('',(5.5,-0.433012701892221,-7.83290376865476));
#53497=CARTESIAN_POINT('',(5.5,0.433012701892217,-7.83290376865476));
#53498=CARTESIAN_POINT('',(5.5,0.433012701892218,-7.83290376865476));
#53499=CARTESIAN_POINT('',(6.,-1.11022302462516E-15,-7.50555349946514));
#53500=CARTESIAN_POINT('Origin',(0.,-2.22044604925031E-15,-7.83290376865476));
#53501=CARTESIAN_POINT('',(0.,-0.433012701892223,-7.83290376865476));
#53502=CARTESIAN_POINT('',(0.,0.433012701892217,-7.83290376865476));
#53503=CARTESIAN_POINT('',(0.,-6.13101691567725E-15,-7.83290376865476));
#53504=CARTESIAN_POINT('',(0.,0.433012701892218,-7.83290376865476));
#53505=CARTESIAN_POINT('',(0.,-0.433012701892222,-7.83290376865476));
#53506=CARTESIAN_POINT('Origin',(5.5,7.,-3.54145188432738));
#53507=CARTESIAN_POINT('',(5.5,6.56698729810778,-4.29145188432738));
#53508=CARTESIAN_POINT('',(6.,6.5,-3.75277674973257));
#53509=CARTESIAN_POINT('',(5.5,6.56698729810778,-4.29145188432739));
#53510=CARTESIAN_POINT('',(5.5,7.,-3.54145188432738));
#53511=CARTESIAN_POINT('',(5.5,7.,-3.54145188432738));
#53512=CARTESIAN_POINT('',(6.,6.5,-3.75277674973257));
#53513=CARTESIAN_POINT('Origin',(0.,6.78349364905389,-3.91645188432738));
#53514=CARTESIAN_POINT('',(0.,6.56698729810778,-4.29145188432739));
#53515=CARTESIAN_POINT('',(0.,7.,-3.54145188432738));
#53516=CARTESIAN_POINT('',(0.,6.78349364905389,-3.91645188432738));
#53517=CARTESIAN_POINT('',(0.,7.,-3.54145188432738));
#53518=CARTESIAN_POINT('',(0.,6.56698729810778,-4.29145188432738));
#53519=CARTESIAN_POINT('Origin',(5.75,6.75,-2.02072594216369));
#53520=CARTESIAN_POINT('',(6.,6.5,-2.02072594216369));
#53521=CARTESIAN_POINT('',(5.5,7.,-2.02072594216369));
#53522=CARTESIAN_POINT('Origin',(5.75,1.625,-6.85603444662681));
#53523=CARTESIAN_POINT('',(6.,1.5,-6.6395280956807));
#53524=CARTESIAN_POINT('',(5.5,1.75,-7.07254079757292));
#53525=CARTESIAN_POINT('Origin',(5.75,-5.125,-4.83530850446312));
#53526=CARTESIAN_POINT('',(6.,-5.,-4.61880215351701));
#53527=CARTESIAN_POINT('',(5.5,-5.25,-5.05181485540923));
#53528=CARTESIAN_POINT('Origin',(5.75,-6.75,2.02072594216369));
#53529=CARTESIAN_POINT('',(6.,-6.5,2.02072594216369));
#53530=CARTESIAN_POINT('',(5.5,-7.,2.02072594216369));
#53531=CARTESIAN_POINT('Origin',(0.,4.94935111404957E-16,8.08290376865476));
#53532=CARTESIAN_POINT('',(0.,4.94935111404957E-16,8.08290376865476));
#53533=CARTESIAN_POINT('Origin',(0.,7.,4.04145188432738));
#53534=CARTESIAN_POINT('',(0.,7.,4.04145188432738));
#53535=CARTESIAN_POINT('Origin',(0.,7.,-4.04145188432738));
#53536=CARTESIAN_POINT('',(0.,7.,-4.04145188432738));
#53537=CARTESIAN_POINT('Origin',(6.,0.,0.));
#53538=CARTESIAN_POINT('',(6.,3.5,2.02072594216369));
#53539=CARTESIAN_POINT('',(6.,-5.55111512312578E-16,4.04145188432738));
#53540=CARTESIAN_POINT('',(6.,1.,3.46410161513775));
#53541=CARTESIAN_POINT('',(6.,3.5,-2.02072594216369));
#53542=CARTESIAN_POINT('',(6.,3.5,0.866025403784438));
#53543=CARTESIAN_POINT('',(6.,-5.55111512312578E-16,-4.04145188432738));
#53544=CARTESIAN_POINT('',(6.,2.5,-2.59807621135332));
#53545=CARTESIAN_POINT('',(6.,-3.5,-2.02072594216369));
#53546=CARTESIAN_POINT('',(6.,-1.,-3.46410161513775));
#53547=CARTESIAN_POINT('',(6.,-3.5,2.02072594216369));
#53548=CARTESIAN_POINT('',(6.,-3.5,-0.866025403784439));
#53549=CARTESIAN_POINT('',(6.,-2.5,2.59807621135332));
#53550=CARTESIAN_POINT('Origin',(5.75,-0.875,-3.24759526419165));
#53551=CARTESIAN_POINT('',(5.5,-6.36345143234944E-16,-3.46410161513775));
#53552=CARTESIAN_POINT('',(6.,-2.77555756156289E-16,-4.04145188432738));
#53553=CARTESIAN_POINT('',(5.5,-3.,-1.73205080756888));
#53554=CARTESIAN_POINT('',(5.5,-0.75,-3.03108891324554));
#53555=CARTESIAN_POINT('',(6.,-3.5,-2.02072594216369));
#53556=CARTESIAN_POINT('Origin',(5.75,2.375,-2.38156986040721));
#53557=CARTESIAN_POINT('',(5.5,3.,-1.73205080756888));
#53558=CARTESIAN_POINT('',(6.,3.5,-2.02072594216369));
#53559=CARTESIAN_POINT('',(5.5,2.25,-2.1650635094611));
#53560=CARTESIAN_POINT('Origin',(5.75,0.875,3.24759526419165));
#53561=CARTESIAN_POINT('',(5.5,2.12115047744981E-16,3.46410161513775));
#53562=CARTESIAN_POINT('',(6.,-5.55111512312578E-16,4.04145188432738));
#53563=CARTESIAN_POINT('',(5.5,3.,1.73205080756888));
#53564=CARTESIAN_POINT('',(5.5,0.75,3.03108891324554));
#53565=CARTESIAN_POINT('',(5.5,3.,1.73205080756888));
#53566=CARTESIAN_POINT('Origin',(5.75,-2.375,2.38156986040721));
#53567=CARTESIAN_POINT('',(5.5,-3.,1.73205080756888));
#53568=CARTESIAN_POINT('',(5.5,-2.25,2.1650635094611));
#53569=CARTESIAN_POINT('',(6.,-3.5,2.02072594216369));
#53570=CARTESIAN_POINT('Origin',(5.75,3.25,0.866025403784438));
#53571=CARTESIAN_POINT('',(5.5,3.,0.866025403784438));
#53572=CARTESIAN_POINT('Origin',(5.75,-3.25,-0.866025403784439));
#53573=CARTESIAN_POINT('',(5.5,-3.,-0.866025403784439));
#53574=CARTESIAN_POINT('Origin',(6.,3.,-1.73205080756888));
#53575=CARTESIAN_POINT('',(2.5,3.,-1.73205080756888));
#53576=CARTESIAN_POINT('',(6.,3.,-1.73205080756888));
#53577=CARTESIAN_POINT('',(2.5,-5.55111512312578E-16,-3.46410161513775));
#53578=CARTESIAN_POINT('',(2.5,-6.36345143234944E-16,-3.46410161513775));
#53579=CARTESIAN_POINT('',(6.,-6.36345143234944E-16,-3.46410161513775));
#53580=CARTESIAN_POINT('Origin',(6.,3.,1.73205080756888));
#53581=CARTESIAN_POINT('',(2.5,3.,1.73205080756888));
#53582=CARTESIAN_POINT('',(6.,3.,1.73205080756888));
#53583=CARTESIAN_POINT('',(2.5,3.,-1.73205080756888));
#53584=CARTESIAN_POINT('Origin',(6.,0.,3.46410161513775));
#53585=CARTESIAN_POINT('',(2.5,0.,3.46410161513775));
#53586=CARTESIAN_POINT('',(6.,2.12115047744981E-16,3.46410161513775));
#53587=CARTESIAN_POINT('',(2.5,3.,1.73205080756888));
#53588=CARTESIAN_POINT('Origin',(6.,-3.,1.73205080756888));
#53589=CARTESIAN_POINT('',(2.5,-3.,1.73205080756888));
#53590=CARTESIAN_POINT('',(6.,-3.,1.73205080756888));
#53591=CARTESIAN_POINT('',(2.5,2.12115047744981E-16,3.46410161513775));
#53592=CARTESIAN_POINT('Origin',(6.,-3.,-1.73205080756888));
#53593=CARTESIAN_POINT('',(2.5,-3.,-1.73205080756888));
#53594=CARTESIAN_POINT('',(6.,-3.,-1.73205080756888));
#53595=CARTESIAN_POINT('',(2.5,-3.,1.73205080756888));
#53596=CARTESIAN_POINT('Origin',(6.,-5.55111512312578E-16,-3.46410161513775));
#53597=CARTESIAN_POINT('',(2.5,-3.,-1.73205080756888));
#53598=CARTESIAN_POINT('Origin',(2.5,0.,0.));
#53599=CARTESIAN_POINT('Origin',(0.,0.,0.));
#53600=CARTESIAN_POINT('',(0.,-1.48480533421487E-15,-8.08290376865476));
#53601=CARTESIAN_POINT('',(0.,-7.,-4.04145188432738));
#53602=CARTESIAN_POINT('',(0.,-7.,4.04145188432738));
#53603=CARTESIAN_POINT('',(0.,-6.85,-8.38883057415937E-16));
#53604=CARTESIAN_POINT('Origin',(0.,0.,0.));
#53605=CARTESIAN_POINT('Origin',(0.,-1.48480533421487E-15,-8.08290376865476));
#53606=CARTESIAN_POINT('Origin',(0.,-7.,-4.04145188432738));
#53607=CARTESIAN_POINT('Origin',(0.,-7.,4.04145188432738));
#53608=CARTESIAN_POINT('Origin',(-10.,6.35,0.));
#53609=CARTESIAN_POINT('',(-10.,-6.35,-7.77650717458569E-16));
#53610=CARTESIAN_POINT('Origin',(-10.,0.,0.));
#53611=CARTESIAN_POINT('Origin',(-9.75,0.,0.));
#53612=CARTESIAN_POINT('',(-9.5,-6.85,-8.38883057415937E-16));
#53613=CARTESIAN_POINT('Origin',(-9.5,0.,0.));
#53614=CARTESIAN_POINT('',(-9.75,-6.6,-8.08266887437253E-16));
#53615=CARTESIAN_POINT('Origin',(-4.75,0.,0.));
#53616=CARTESIAN_POINT('',(-4.75,-6.85,-8.38883057415937E-16));
#53617=CARTESIAN_POINT('',(0.,0.,0.));
#53618=CARTESIAN_POINT('Origin',(-4.85,0.,0.));
#53619=CARTESIAN_POINT('',(-9.49167250378795,-2.45327747456172,0.00165524322402417));
#53620=CARTESIAN_POINT('',(-9.60732749621206,-2.45271517060122,0.00261677541903093));
#53621=CARTESIAN_POINT('',(-4.85,-2.4505,-3.00099698131059E-16));
#53622=CARTESIAN_POINT('',(-9.7495,1.07637022042037,2.20364147798228));
#53623=CARTESIAN_POINT('Ctrl Pts',(-9.49167250378795,-2.45327747456172,
0.00165524322402417));
#53624=CARTESIAN_POINT('Ctrl Pts',(-9.49633463918664,-2.4539194957778,0.0910866010723908));
#53625=CARTESIAN_POINT('Ctrl Pts',(-9.50099677458534,-2.44945222484254,
0.180449214552893));
#53626=CARTESIAN_POINT('Ctrl Pts',(-9.50565890998403,-2.43966236895119,
0.269219861232167));
#53627=CARTESIAN_POINT('Ctrl Pts',(-9.54790628291729,-2.3509485806471,1.07364236188226));
#53628=CARTESIAN_POINT('Ctrl Pts',(-9.59015365585055,-1.825163527862,1.82945470779013));
#53629=CARTESIAN_POINT('Ctrl Pts',(-9.63240102878381,-1.10182743978963,
2.19303587121579));
#53630=CARTESIAN_POINT('Ctrl Pts',(-9.67143401918921,-0.433526226594529,
2.52895403791445));
#53631=CARTESIAN_POINT('Ctrl Pts',(-9.7104670095946,0.4034083658124,2.53005609171326));
#53632=CARTESIAN_POINT('Ctrl Pts',(-9.7495,1.07765198048948,2.20520778639847));
#53633=CARTESIAN_POINT('',(-9.7495,-1.07508846035133,2.20207516956606));
#53634=CARTESIAN_POINT('Origin',(-9.7495,0.,0.));
#53635=CARTESIAN_POINT('Ctrl Pts',(-9.7495,-1.07508846035133,2.20207516956606));
#53636=CARTESIAN_POINT('Ctrl Pts',(-9.70725262706674,-1.80575922297742,
1.8453499695947));
#53637=CARTESIAN_POINT('Ctrl Pts',(-9.66500525413347,-2.33873961907574,
1.09958288884865));
#53638=CARTESIAN_POINT('Ctrl Pts',(-9.62275788120021,-2.43620643494331,
0.297400442061077));
#53639=CARTESIAN_POINT('Ctrl Pts',(-9.61761441953749,-2.448072659894,0.199737691099642));
#53640=CARTESIAN_POINT('Ctrl Pts',(-9.61247095787478,-2.45348363138364,
0.101238742362921));
#53641=CARTESIAN_POINT('Ctrl Pts',(-9.60732749621206,-2.45271517060122,
0.00261677541903093));
#53642=CARTESIAN_POINT('Origin',(-4.85,0.,0.));
#53643=CARTESIAN_POINT('',(-8.69167250378794,-2.44691142445882,0.000997465547478843));
#53644=CARTESIAN_POINT('',(-8.80732749621206,-2.44679980543952,0.000874454649755137));
#53645=CARTESIAN_POINT('',(-4.85,-2.4505,-3.00099698131059E-16));
#53646=CARTESIAN_POINT('Ctrl Pts',(-8.69167250378794,-2.44691142445882,
0.000997465547478843));
#53647=CARTESIAN_POINT('Ctrl Pts',(-8.70951706825373,-2.4481762977678,0.345611269438561));
#53648=CARTESIAN_POINT('Ctrl Pts',(-8.72736163271951,-2.38025527099653,
0.689748316659788));
#53649=CARTESIAN_POINT('Ctrl Pts',(-8.7452061971853,-2.24070602085676,1.00185768813625));
#53650=CARTESIAN_POINT('Ctrl Pts',(-8.78745357011856,-1.91032030454994,
1.74078303641323));
#53651=CARTESIAN_POINT('Ctrl Pts',(-8.82970094305183,-1.17844740017566,
2.30018834537626));
#53652=CARTESIAN_POINT('Ctrl Pts',(-8.8719483159851,-0.378714078450958,
2.42508315806902));
#53653=CARTESIAN_POINT('Ctrl Pts',(-8.91419568891836,0.42101924327374,2.54997797076177));
#53654=CARTESIAN_POINT('Ctrl Pts',(-8.95644306185162,1.28861298234885,2.24036228718424));
#53655=CARTESIAN_POINT('Ctrl Pts',(-8.99869043478488,1.82856107840019,1.63734074473426));
#53656=CARTESIAN_POINT('Ctrl Pts',(-9.04093780771814,2.36850917445153,1.03431920228428));
#53657=CARTESIAN_POINT('Ctrl Pts',(-9.0831851806514,2.5808116274791,0.137891800961835));
#53658=CARTESIAN_POINT('Ctrl Pts',(-9.12543255358466,2.36870098520686,-0.643228817589892));
#53659=CARTESIAN_POINT('Ctrl Pts',(-9.16767992651792,2.15659034293461,-1.42434943614162));
#53660=CARTESIAN_POINT('Ctrl Pts',(-9.20992729945119,1.52006660536256,-2.09016327192263));
#53661=CARTESIAN_POINT('Ctrl Pts',(-9.25217467238445,0.749270724461215,
-2.33728533022963));
#53662=CARTESIAN_POINT('Ctrl Pts',(-9.29442204531772,-0.0215251564401345,
-2.58440738853662));
#53663=CARTESIAN_POINT('Ctrl Pts',(-9.33666941825097,-0.926593180670786,
-2.4128376693696));
#53664=CARTESIAN_POINT('Ctrl Pts',(-9.37891679118423,-1.55330593087457,
-1.90053648208992));
#53665=CARTESIAN_POINT('Ctrl Pts',(-9.4165020287188,-2.11085888498516,-1.44476940176601));
#53666=CARTESIAN_POINT('Ctrl Pts',(-9.45408726625338,-2.44810162318784,
-0.719323136921701));
#53667=CARTESIAN_POINT('Ctrl Pts',(-9.49167250378795,-2.45327747456172,
0.00165524322402417));
#53668=CARTESIAN_POINT('Ctrl Pts',(-9.60732749621206,-2.45271517060122,
0.00261677541903093));
#53669=CARTESIAN_POINT('Ctrl Pts',(-9.57022358494152,-2.44717164708428,
-0.708822514065269));
#53670=CARTESIAN_POINT('Ctrl Pts',(-9.53311967367097,-2.12005707050393,
-1.42666353961262));
#53671=CARTESIAN_POINT('Ctrl Pts',(-9.49601576240043,-1.57491430716428,
-1.88317974641052));
#53672=CARTESIAN_POINT('Ctrl Pts',(-9.45376838946716,-0.954202127880854,
-2.40297967526545));
#53673=CARTESIAN_POINT('Ctrl Pts',(-9.4115210165339,-0.0508245336771831,
-2.5839817201462));
#53674=CARTESIAN_POINT('Ctrl Pts',(-9.36927364360064,0.7227993233438,-2.34541864510377));
#53675=CARTESIAN_POINT('Ctrl Pts',(-9.32702627066737,1.49642318036478,-2.10685557006134));
#53676=CARTESIAN_POINT('Ctrl Pts',(-9.28477889773412,2.14029330020308,-1.44872737509573));
#53677=CARTESIAN_POINT('Ctrl Pts',(-9.24253152480085,2.36120984472134,-0.670163752243124));
#53678=CARTESIAN_POINT('Ctrl Pts',(-9.20028415186759,2.58212638923961,0.108399870609487));
#53679=CARTESIAN_POINT('Ctrl Pts',(-9.15803677893433,2.38008935843785,1.0073989213491));
#53680=CARTESIAN_POINT('Ctrl Pts',(-9.11578940600107,1.84703509648051,1.61655781423769));
#53681=CARTESIAN_POINT('Ctrl Pts',(-9.0735420330678,1.31398083452317,2.22571670712627));
#53682=CARTESIAN_POINT('Ctrl Pts',(-9.03129466013454,0.449909341410258,
2.54503544216384));
#53683=CARTESIAN_POINT('Ctrl Pts',(-8.98904728720128,-0.351199568854151,
2.42919060595784));
#53684=CARTESIAN_POINT('Ctrl Pts',(-8.94679991426801,-1.15230847911856,
2.31334576975184));
#53685=CARTESIAN_POINT('Ctrl Pts',(-8.90455254133475,-1.89045480653447,
1.76233736230228));
#53686=CARTESIAN_POINT('Ctrl Pts',(-8.86230516840149,-2.22919361727906,
1.02722088666372));
#53687=CARTESIAN_POINT('Ctrl Pts',(-8.84397927767168,-2.37613033785236,
0.708345101712173));
#53688=CARTESIAN_POINT('Ctrl Pts',(-8.82565338694187,-2.44791394062357,
0.354827266324934));
#53689=CARTESIAN_POINT('Ctrl Pts',(-8.80732749621206,-2.44679980543952,
0.000874454649755137));
#53690=CARTESIAN_POINT('Origin',(-4.85,0.,0.));
#53691=CARTESIAN_POINT('',(-7.89167250378795,-2.44971218776673,-0.00219053278463388));
#53692=CARTESIAN_POINT('',(-8.00732749621207,-2.44998306124988,-0.00220861612412772));
#53693=CARTESIAN_POINT('',(-4.85,-2.4505,-3.00099698131059E-16));
#53694=CARTESIAN_POINT('Ctrl Pts',(-7.89167250378795,-2.44971218776673,
-0.00219053278463388));
#53695=CARTESIAN_POINT('Ctrl Pts',(-7.92269949732083,-2.44447247776505,
0.595274393060675));
#53696=CARTESIAN_POINT('Ctrl Pts',(-7.95372649085371,-2.22417636360755,
1.19619884911934));
#53697=CARTESIAN_POINT('Ctrl Pts',(-7.98475348438658,-1.82728666671986,
1.63875025584126));
#53698=CARTESIAN_POINT('Ctrl Pts',(-8.02700085731984,-1.28686862653767,
2.24134277909389));
#53699=CARTESIAN_POINT('Ctrl Pts',(-8.0692482302531,-0.419038321458612,
2.55030470728015));
#53700=CARTESIAN_POINT('Ctrl Pts',(-8.11149560318637,0.380596882636705,
2.42479364987812));
#53701=CARTESIAN_POINT('Ctrl Pts',(-8.15374297611963,1.18023208673203,2.29928259247609));
#53702=CARTESIAN_POINT('Ctrl Pts',(-8.19599034905289,1.9116721898436,1.73929854948577));
#53703=CARTESIAN_POINT('Ctrl Pts',(-8.23823772198616,2.24148419393013,1.00011400763455));
#53704=CARTESIAN_POINT('Ctrl Pts',(-8.28048509491942,2.57129619801665,0.260929465783332));
#53705=CARTESIAN_POINT('Ctrl Pts',(-8.32273246785268,2.49948010307813,-0.657455574928778));
#53706=CARTESIAN_POINT('Ctrl Pts',(-8.36497984078594,2.05877411056465,-1.33638646263042));
#53707=CARTESIAN_POINT('Ctrl Pts',(-8.40722721371921,1.61806811805117,-2.01531735033206));
#53708=CARTESIAN_POINT('Ctrl Pts',(-8.44947458665247,0.808472227962739,
-2.45479408502322));
#53709=CARTESIAN_POINT('Ctrl Pts',(-8.49172195958573,-0.0009532390009169,
-2.4544803883035));
#53710=CARTESIAN_POINT('Ctrl Pts',(-8.53396933251899,-0.810378705964571,
-2.45416669158379));
#53711=CARTESIAN_POINT('Ctrl Pts',(-8.57621670545226,-1.61963374980345,
-2.01406256345319));
#53712=CARTESIAN_POINT('Ctrl Pts',(-8.61846407838552,-2.0598120076032,-1.33478780559243));
#53713=CARTESIAN_POINT('Ctrl Pts',(-8.64286688685299,-2.3140665321059,-0.942427034685969));
#53714=CARTESIAN_POINT('Ctrl Pts',(-8.66726969532047,-2.44518168422594,
-0.47026899028148));
#53715=CARTESIAN_POINT('Ctrl Pts',(-8.69167250378794,-2.44691142445882,
0.000997465547478843));
#53716=CARTESIAN_POINT('Ctrl Pts',(-8.80732749621206,-2.44679980543952,
0.000874454649755137));
#53717=CARTESIAN_POINT('Ctrl Pts',(-8.78340601400861,-2.44534548240713,
-0.461153613190768));
#53718=CARTESIAN_POINT('Ctrl Pts',(-8.75948453180516,-2.31968016518885,
-0.923922840341414));
#53719=CARTESIAN_POINT('Ctrl Pts',(-8.73556304960171,-2.07482021352832,
-1.311350703522));
#53720=CARTESIAN_POINT('Ctrl Pts',(-8.69331567666844,-1.64237670495972,
-1.99558127424157));
#53721=CARTESIAN_POINT('Ctrl Pts',(-8.65106830373517,-0.83815839374923,
-2.44481787185314));
#53722=CARTESIAN_POINT('Ctrl Pts',(-8.60882093080191,-0.0287870535078842,
-2.45430704848734));
#53723=CARTESIAN_POINT('Ctrl Pts',(-8.56657355786865,0.780584286733466,
-2.46379622512154));
#53724=CARTESIAN_POINT('Ctrl Pts',(-8.5243261849354,1.59510865600568,-2.03353798077836));
#53725=CARTESIAN_POINT('Ctrl Pts',(-8.48207881200214,2.04348504860573,-1.35965082042215));
#53726=CARTESIAN_POINT('Ctrl Pts',(-8.43983143906888,2.49186144120578,-0.685763660065949));
#53727=CARTESIAN_POINT('Ctrl Pts',(-8.39758406613561,2.57408985713368,0.23175241630329));
#53728=CARTESIAN_POINT('Ctrl Pts',(-8.35533669320234,2.25268240724564,0.974630779216524));
#53729=CARTESIAN_POINT('Ctrl Pts',(-8.31308932026908,1.93127495735761,1.71750914212977));
#53730=CARTESIAN_POINT('Ctrl Pts',(-8.27084194733582,1.20623164165363,2.285749791587));
#53731=CARTESIAN_POINT('Ctrl Pts',(-8.22859457440256,0.408071081466186,
2.42032064888589));
#53732=CARTESIAN_POINT('Ctrl Pts',(-8.1863472014693,-0.390089478721252,
2.55489150618479));
#53733=CARTESIAN_POINT('Ctrl Pts',(-8.14409982853603,-1.26136728339215,
2.25579257132536));
#53734=CARTESIAN_POINT('Ctrl Pts',(-8.10185245560277,-1.80858426161825,
1.65936788193681));
#53735=CARTESIAN_POINT('Ctrl Pts',(-8.07034413580586,-2.21670165096406,
1.21455111480413));
#53736=CARTESIAN_POINT('Ctrl Pts',(-8.03883581600897,-2.44456807139402,
0.604354113579378));
#53737=CARTESIAN_POINT('Ctrl Pts',(-8.00732749621207,-2.44998306124988,
-0.00220861612412772));
#53738=CARTESIAN_POINT('Origin',(-4.85,0.,0.));
#53739=CARTESIAN_POINT('',(-7.09167250378795,-2.45424633052781,0.000682524973613097));
#53740=CARTESIAN_POINT('',(-7.20732749621206,-2.45412426038782,0.000841066407299921));
#53741=CARTESIAN_POINT('',(-4.85,-2.4505,-3.00099698131059E-16));
#53742=CARTESIAN_POINT('Ctrl Pts',(-7.09167250378795,-2.45424633052781,
0.000682524973613097));
#53743=CARTESIAN_POINT('Ctrl Pts',(-7.09363455345465,-2.45438587279557,
0.0382834665408473));
#53744=CARTESIAN_POINT('Ctrl Pts',(-7.09559660312136,-2.4535962127551,0.0758784207214286));
#53745=CARTESIAN_POINT('Ctrl Pts',(-7.09755865278807,-2.45185899785181,
0.113429538489877));
#53746=CARTESIAN_POINT('Ctrl Pts',(-7.13980602572134,-2.41445282657598,
0.921990149030203));
#53747=CARTESIAN_POINT('Ctrl Pts',(-7.1820533986546,-1.93772380966174,1.71022651442513));
#53748=CARTESIAN_POINT('Ctrl Pts',(-7.22430077158786,-1.23899271099641,
2.11881473280963));
#53749=CARTESIAN_POINT('Ctrl Pts',(-7.26654814452113,-0.540261612331091,
2.52740295119414));
#53750=CARTESIAN_POINT('Ctrl Pts',(-7.30879551745439,0.3804715680853,2.55634302256822));
#53751=CARTESIAN_POINT('Ctrl Pts',(-7.35104289038765,1.10348319354511,2.19244239041122));
#53752=CARTESIAN_POINT('Ctrl Pts',(-7.39329026332091,1.82649481900493,1.82854175825421));
#53753=CARTESIAN_POINT('Ctrl Pts',(-7.43553763625417,2.35178488950816,1.07180042256612));
#53754=CARTESIAN_POINT('Ctrl Pts',(-7.47778500918743,2.4398956916372,0.267185002312099));
#53755=CARTESIAN_POINT('Ctrl Pts',(-7.5200323821207,2.52800649376624,-0.537430417941909));
#53756=CARTESIAN_POINT('Ctrl Pts',(-7.56227975505396,2.17893802752108,-1.38991992276184));
#53757=CARTESIAN_POINT('Ctrl Pts',(-7.60452712798722,1.55181597081934,-1.90166927357545));
#53758=CARTESIAN_POINT('Ctrl Pts',(-7.64677450092048,0.924693914117586,
-2.41341862438908));
#53759=CARTESIAN_POINT('Ctrl Pts',(-7.68902187385375,0.0195182669592417,
-2.58442782119639));
#53760=CARTESIAN_POINT('Ctrl Pts',(-7.73126924678701,-0.751079369498862,
-2.33674100060766));
#53761=CARTESIAN_POINT('Ctrl Pts',(-7.77351661972027,-1.52167700595696,
-2.08905418001893));
#53762=CARTESIAN_POINT('Ctrl Pts',(-7.81576399265353,-2.15769663171482,
-1.42267134203417));
#53763=CARTESIAN_POINT('Ctrl Pts',(-7.85801136558679,-2.36920355695109,
-0.641368363882281));
#53764=CARTESIAN_POINT('Ctrl Pts',(-7.86923174498718,-2.42537717869814,
-0.433863962239076));
#53765=CARTESIAN_POINT('Ctrl Pts',(-7.88045212438756,-2.45160703890997,
-0.218253463255248));
#53766=CARTESIAN_POINT('Ctrl Pts',(-7.89167250378795,-2.44971218776673,
-0.00219053278463388));
#53767=CARTESIAN_POINT('Ctrl Pts',(-8.00732749621207,-2.44998306124988,
-0.00220861612412772));
#53768=CARTESIAN_POINT('Ctrl Pts',(-7.99658844307571,-2.45182866470223,
-0.208944786977084));
#53769=CARTESIAN_POINT('Ctrl Pts',(-7.98584938993934,-2.42783282903302,
-0.415258776655366));
#53770=CARTESIAN_POINT('Ctrl Pts',(-7.97511033680298,-2.37632469663013,
-0.614458734829266));
#53771=CARTESIAN_POINT('Ctrl Pts',(-7.93286296386972,-2.17369200163464,
-1.3981102182891));
#53772=CARTESIAN_POINT('Ctrl Pts',(-7.89061559093646,-1.54527045986237,
-2.07166274129109));
#53773=CARTESIAN_POINT('Ctrl Pts',(-7.8483682180032,-0.777531351301464,
-2.32807268057354));
#53774=CARTESIAN_POINT('Ctrl Pts',(-7.80612084506993,-0.00979224274055196,
-2.58448261985599));
#53775=CARTESIAN_POINT('Ctrl Pts',(-7.76387347213667,0.897264432609006,
-2.42374997541889));
#53776=CARTESIAN_POINT('Ctrl Pts',(-7.72162609920341,1.53014971651881,-1.91914564019643));
#53777=CARTESIAN_POINT('Ctrl Pts',(-7.67937872627014,2.16303500042861,-1.41454130497397));
#53778=CARTESIAN_POINT('Ctrl Pts',(-7.63713135333688,2.52174889289865,-0.566065278966143));
#53779=CARTESIAN_POINT('Ctrl Pts',(-7.59488398040362,2.44276870532455,0.239497607437949));
#53780=CARTESIAN_POINT('Ctrl Pts',(-7.55263660747036,2.36378851775044,1.04506049384204));
#53781=CARTESIAN_POINT('Ctrl Pts',(-7.5103892345371,1.84711425013217,1.80771024064241));
#53782=CARTESIAN_POINT('Ctrl Pts',(-7.46814186160384,1.12827606704126,2.17978692041014));
#53783=CARTESIAN_POINT('Ctrl Pts',(-7.42589448867057,0.409437883950348,
2.55186360017788));
#53784=CARTESIAN_POINT('Ctrl Pts',(-7.38364711573731,-0.511564214613206,
2.533367212913));
#53785=CARTESIAN_POINT('Ctrl Pts',(-7.34139974280405,-1.21488402143036,
2.13272943126949));
#53786=CARTESIAN_POINT('Ctrl Pts',(-7.29915236987079,-1.91820382824751,
1.73209164962598));
#53787=CARTESIAN_POINT('Ctrl Pts',(-7.25690499693752,-2.40384134331826,
0.949312473603835));
#53788=CARTESIAN_POINT('Ctrl Pts',(-7.21465762400426,-2.45041478266452,
0.141228125619655));
#53789=CARTESIAN_POINT('Ctrl Pts',(-7.21221424807353,-2.45310835655585,
0.0944925842408962));
#53790=CARTESIAN_POINT('Ctrl Pts',(-7.20977087214279,-2.45433331169064,
0.0476723999768843));
#53791=CARTESIAN_POINT('Ctrl Pts',(-7.20732749621206,-2.45412426038782,
0.000841066407299921));
#53792=CARTESIAN_POINT('Origin',(-4.85,0.,0.));
#53793=CARTESIAN_POINT('',(-6.29167250378795,-2.44778349460883,0.00166651518545433));
#53794=CARTESIAN_POINT('',(-6.40732749621207,-2.44759559891841,0.00156187491458784));
#53795=CARTESIAN_POINT('',(-4.85,-2.4505,-3.00099698131059E-16));
#53796=CARTESIAN_POINT('Ctrl Pts',(-6.29167250378795,-2.44778349460883,
0.00166651518545433));
#53797=CARTESIAN_POINT('Ctrl Pts',(-6.30681698252175,-2.44962168320389,
0.293874483510101));
#53798=CARTESIAN_POINT('Ctrl Pts',(-6.32196146125555,-2.40122185351473,
0.585493705442811));
#53799=CARTESIAN_POINT('Ctrl Pts',(-6.33710593998935,-2.29986782320631,
0.857372031787032));
#53800=CARTESIAN_POINT('Ctrl Pts',(-6.37935331292261,-2.01712837789465,
1.61580982601093));
#53801=CARTESIAN_POINT('Ctrl Pts',(-6.42160068585587,-1.32229978843967,
2.22062413668589));
#53802=CARTESIAN_POINT('Ctrl Pts',(-6.46384805878913,-0.532125265238115,
2.39610548752291));
#53803=CARTESIAN_POINT('Ctrl Pts',(-6.5060954317224,0.258049257963456,2.57158683835993));
#53804=CARTESIAN_POINT('Ctrl Pts',(-6.54834280465566,1.14356971491161,2.31773522935899));
#53805=CARTESIAN_POINT('Ctrl Pts',(-6.59059017758893,1.72076447115239,1.75027096180509));
#53806=CARTESIAN_POINT('Ctrl Pts',(-6.63283755052219,2.29795922739315,1.1828066942512));
#53807=CARTESIAN_POINT('Ctrl Pts',(-6.67508492345545,2.56682828292656,0.301729768144353));
#53808=CARTESIAN_POINT('Ctrl Pts',(-6.71733229638871,2.40480551258969,-0.491313801687984));
#53809=CARTESIAN_POINT('Ctrl Pts',(-6.75957966932197,2.24278274225283,-1.28435737152033));
#53810=CARTESIAN_POINT('Ctrl Pts',(-6.80182704225524,1.64986814604569,-1.98936758507816));
#53811=CARTESIAN_POINT('Ctrl Pts',(-6.8440744151885,0.896346619568618,-2.28495985598806));
#53812=CARTESIAN_POINT('Ctrl Pts',(-6.88632178812176,0.142825093091551,
-2.58055212689795));
#53813=CARTESIAN_POINT('Ctrl Pts',(-6.92856916105502,-0.771303363655447,
-2.46672645515992));
#53814=CARTESIAN_POINT('Ctrl Pts',(-6.97081653398828,-1.42932592921024,
-1.99537119144805));
#53815=CARTESIAN_POINT('Ctrl Pts',(-7.01110185725484,-2.05678865480829,
-1.54590657735191));
#53816=CARTESIAN_POINT('Ctrl Pts',(-7.05138718052139,-2.45138121173831,
-0.771349963227231));
#53817=CARTESIAN_POINT('Ctrl Pts',(-7.09167250378795,-2.45424633052781,
0.000682524973613097));
#53818=CARTESIAN_POINT('Ctrl Pts',(-7.20732749621206,-2.45412426038782,
0.000841066407299921));
#53819=CARTESIAN_POINT('Ctrl Pts',(-7.16752349920953,-2.45071869461871,
-0.762068249994661));
#53820=CARTESIAN_POINT('Ctrl Pts',(-7.127719502207,-2.06675247208674,-1.52793640042953));
#53821=CARTESIAN_POINT('Ctrl Pts',(-7.08791550520447,-1.4518628975676,-1.97903312234382));
#53822=CARTESIAN_POINT('Ctrl Pts',(-7.04566813227121,-0.799228209502633,
-2.45782050237689));
#53823=CARTESIAN_POINT('Ctrl Pts',(-7.00342075933795,0.113550530249083,
-2.58200574249679));
#53824=CARTESIAN_POINT('Ctrl Pts',(-6.96117338640468,0.870375782186031,
-2.29497799264066));
#53825=CARTESIAN_POINT('Ctrl Pts',(-6.91892601347142,1.62720103412297,-2.00795024278453));
#53826=CARTESIAN_POINT('Ctrl Pts',(-6.87667864053816,2.22807279824515,-1.30970950295236));
#53827=CARTESIAN_POINT('Ctrl Pts',(-6.8344312676049,2.3990788384909,-0.518554443884578));
#53828=CARTESIAN_POINT('Ctrl Pts',(-6.79218389467164,2.57008487873666,0.272600615183211));
#53829=CARTESIAN_POINT('Ctrl Pts',(-6.74993652173838,2.31122519510601,1.15666999348662));
#53830=CARTESIAN_POINT('Ctrl Pts',(-6.70768914880512,1.74050306065297,1.73064354459267));
#53831=CARTESIAN_POINT('Ctrl Pts',(-6.66544177587185,1.16978092619992,2.30461709569873));
#53832=CARTESIAN_POINT('Ctrl Pts',(-6.62319440293859,0.287196340924479,
2.56849481960743));
#53833=CARTESIAN_POINT('Ctrl Pts',(-6.58094703000532,-0.504917401848296,
2.40198592881454));
#53834=CARTESIAN_POINT('Ctrl Pts',(-6.53869965707206,-1.29703114462107,
2.23547703802164));
#53835=CARTESIAN_POINT('Ctrl Pts',(-6.4964522841388,-1.99867404489118,1.63858153252716));
#53836=CARTESIAN_POINT('Ctrl Pts',(-6.45420491120554,-2.28999653358123,
0.883399037985938));
#53837=CARTESIAN_POINT('Ctrl Pts',(-6.43857910620771,-2.39774639076035,
0.604083814856844));
#53838=CARTESIAN_POINT('Ctrl Pts',(-6.42295330120989,-2.44936450788483,
0.30311496721273));
#53839=CARTESIAN_POINT('Ctrl Pts',(-6.40732749621207,-2.44759559891841,
0.00156187491458784));
#53840=CARTESIAN_POINT('Origin',(-4.85,0.,0.));
#53841=CARTESIAN_POINT('',(-5.49167250378794,-2.44831607326794,-0.00189653782627697));
#53842=CARTESIAN_POINT('',(-5.60732749621207,-2.44854493522231,-0.00197153692530977));
#53843=CARTESIAN_POINT('',(-4.85,-2.4505,-3.00099698131059E-16));
#53844=CARTESIAN_POINT('Ctrl Pts',(-5.49167250378794,-2.44831607326794,
-0.00189653782627697));
#53845=CARTESIAN_POINT('Ctrl Pts',(-5.51999941158884,-2.44434671486883,
0.544362953986012));
#53846=CARTESIAN_POINT('Ctrl Pts',(-5.54832631938974,-2.26370630972924,
1.0930041977374));
#53847=CARTESIAN_POINT('Ctrl Pts',(-5.57665322719063,-1.92777581339653,
1.51926272198234));
#53848=CARTESIAN_POINT('Ctrl Pts',(-5.61890060012389,-1.42676168725263,
2.15499405440788));
#53849=CARTESIAN_POINT('Ctrl Pts',(-5.66114797305715,-0.580329673604588,
2.5185046667982));
#53850=CARTESIAN_POINT('Ctrl Pts',(-5.70339534599041,0.225667374856916,
2.44408531787464));
#53851=CARTESIAN_POINT('Ctrl Pts',(-5.74564271892368,1.03166442331841,2.36966596895107));
#53852=CARTESIAN_POINT('Ctrl Pts',(-5.78789009185694,1.79722650659338,1.85731665871363));
#53853=CARTESIAN_POINT('Ctrl Pts',(-5.8301374647902,2.17336598128022,1.14059594797335));
#53854=CARTESIAN_POINT('Ctrl Pts',(-5.87238483772346,2.54950545596706,0.423875237233074));
#53855=CARTESIAN_POINT('Ctrl Pts',(-5.91463221065673,2.53622232206579,-0.497216874010042));
#53856=CARTESIAN_POINT('Ctrl Pts',(-5.95687958358999,2.13957180317949,-1.2027931260855));
#53857=CARTESIAN_POINT('Ctrl Pts',(-5.99912695652325,1.7429212842932,-1.90836937816096));
#53858=CARTESIAN_POINT('Ctrl Pts',(-6.04137432945651,0.96290338042188,-2.39842977106876));
#53859=CARTESIAN_POINT('Ctrl Pts',(-6.08362170238978,0.155095537252022,
-2.44957632652366));
#53860=CARTESIAN_POINT('Ctrl Pts',(-6.12586907532304,-0.65271230591783,
-2.50072288197856));
#53861=CARTESIAN_POINT('Ctrl Pts',(-6.1681164482563,-1.48831008838622,-2.11295559998057));
#53862=CARTESIAN_POINT('Ctrl Pts',(-6.21036382118956,-1.97078382903626,
-1.46304132009516));
#53863=CARTESIAN_POINT('Ctrl Pts',(-6.23746671538902,-2.28030448887734,
-1.04610278064375));
#53864=CARTESIAN_POINT('Ctrl Pts',(-6.26456960958849,-2.4444938316309,-0.521275329756746));
#53865=CARTESIAN_POINT('Ctrl Pts',(-6.29167250378795,-2.44778349460883,
0.00166651518545433));
#53866=CARTESIAN_POINT('Ctrl Pts',(-6.40732749621207,-2.44759559891841,
0.00156187491458784));
#53867=CARTESIAN_POINT('Ctrl Pts',(-6.38070592827663,-2.44458192184847,
-0.512191889059406));
#53868=CARTESIAN_POINT('Ctrl Pts',(-6.35408436034119,-2.2866087506118,-1.02764146309601));
#53869=CARTESIAN_POINT('Ctrl Pts',(-6.32746279240576,-1.98724892687709,
-1.44059698964044));
#53870=CARTESIAN_POINT('Ctrl Pts',(-6.28521541947249,-1.51217675437289,
-2.09594103913763));
#53871=CARTESIAN_POINT('Ctrl Pts',(-6.24296804653923,-0.681030332254514,
-2.49315965454405));
#53872=CARTESIAN_POINT('Ctrl Pts',(-6.20072067360596,0.127305546892975,
-2.45117752967657));
#53873=CARTESIAN_POINT('Ctrl Pts',(-6.1584733006727,0.935641426040468,-2.40919540480908));
#53874=CARTESIAN_POINT('Ctrl Pts',(-6.11622592773944,1.72116676221708,-1.92801253966767));
#53875=CARTESIAN_POINT('Ctrl Pts',(-6.07397855480618,2.1257935023211,-1.22698002005643));
#53876=CARTESIAN_POINT('Ctrl Pts',(-6.03173118187292,2.53042024242512,-0.525947500445177));
#53877=CARTESIAN_POINT('Ctrl Pts',(-5.98948380893965,2.55414838645656,0.394934673635915));
#53878=CARTESIAN_POINT('Ctrl Pts',(-5.94723643600639,2.18616126880922,1.11587494410122));
#53879=CARTESIAN_POINT('Ctrl Pts',(-5.90498906307313,1.81817415116189,1.83681521456651));
#53880=CARTESIAN_POINT('Ctrl Pts',(-5.86274169013987,1.05847177183578,2.35781358141602));
#53881=CARTESIAN_POINT('Ctrl Pts',(-5.8204943172066,0.253370580970988,2.44136874168104));
#53882=CARTESIAN_POINT('Ctrl Pts',(-5.77824694427334,-0.551730609893816,
2.52492390194606));
#53883=CARTESIAN_POINT('Ctrl Pts',(-5.73599957134008,-1.40223061229731,
2.17103585562659));
#53884=CARTESIAN_POINT('Ctrl Pts',(-5.69375219840682,-1.91042214809686,
1.5410273197443));
#53885=CARTESIAN_POINT('Ctrl Pts',(-5.6649439643419,-2.25695495467515,1.11142822033371));
#53886=CARTESIAN_POINT('Ctrl Pts',(-5.63613573027698,-2.44432132291076,
0.553438738665929));
#53887=CARTESIAN_POINT('Ctrl Pts',(-5.60732749621207,-2.44854493522231,
-0.00197153692530977));
#53888=CARTESIAN_POINT('Origin',(-4.85,0.,0.));
#53889=CARTESIAN_POINT('',(-4.69167250378794,-2.45444635238797,-0.00026109281808101));
#53890=CARTESIAN_POINT('',(-4.80732749621206,-2.45447688366933,-9.10453097679518E-5));
#53891=CARTESIAN_POINT('',(-4.85,-2.4505,-3.00099698131059E-16));
#53892=CARTESIAN_POINT('Ctrl Pts',(-4.69167250378794,-2.45444635238797,
-0.00026109281808101));
#53893=CARTESIAN_POINT('Ctrl Pts',(-4.73318184065593,-2.45323838965266,
0.795054750259954));
#53894=CARTESIAN_POINT('Ctrl Pts',(-4.77469117752392,-2.03080581207006,
1.59147263731996));
#53895=CARTESIAN_POINT('Ctrl Pts',(-4.81620051439191,-1.37119273741817,
2.03575766779202));
#53896=CARTESIAN_POINT('Ctrl Pts',(-4.85844788732517,-0.699851741412878,
2.48794208670272));
#53897=CARTESIAN_POINT('Ctrl Pts',(-4.90069526025843,0.217178870277101,
2.57536048448576));
#53898=CARTESIAN_POINT('Ctrl Pts',(-4.94294263319169,0.961863305267408,
2.25816248022647));
#53899=CARTESIAN_POINT('Ctrl Pts',(-4.98519000612495,1.70654774025772,1.94096447596719));
#53900=CARTESIAN_POINT('Ctrl Pts',(-5.02743737905822,2.27888599854835,1.21915006966559));
#53901=CARTESIAN_POINT('Ctrl Pts',(-5.06968475199148,2.41797307406147,0.421764173723033));
#53902=CARTESIAN_POINT('Ctrl Pts',(-5.11193212492474,2.55706014957458,-0.375621722219518));
#53903=CARTESIAN_POINT('Ctrl Pts',(-5.154179497858,2.26289604231019,-1.24857910780302));
#53904=CARTESIAN_POINT('Ctrl Pts',(-5.19642687079127,1.66957783049421,-1.79916332583916));
#53905=CARTESIAN_POINT('Ctrl Pts',(-5.23867424372453,1.07625961867823,-2.34974754387529));
#53906=CARTESIAN_POINT('Ctrl Pts',(-5.28092161665779,0.183787302310668,
-2.57795859436406));
#53907=CARTESIAN_POINT('Ctrl Pts',(-5.32316898959106,-0.600998423000285,
-2.37976463136043));
#53908=CARTESIAN_POINT('Ctrl Pts',(-5.36541636252432,-1.38578414831124,
-2.1815706683568));
#53909=CARTESIAN_POINT('Ctrl Pts',(-5.40766373545758,-2.06288328256559,
-1.55697169186076));
#53910=CARTESIAN_POINT('Ctrl Pts',(-5.44991110839084,-2.32363473037289,
-0.790696177382358));
#53911=CARTESIAN_POINT('Ctrl Pts',(-5.46383157352321,-2.40955205931899,
-0.538209197944985));
#53912=CARTESIAN_POINT('Ctrl Pts',(-5.47775203865557,-2.45026670323366,
-0.270340459148239));
#53913=CARTESIAN_POINT('Ctrl Pts',(-5.49167250378794,-2.44831607326794,
-0.00189653782627697));
#53914=CARTESIAN_POINT('Ctrl Pts',(-5.60732749621207,-2.44854493522231,
-0.00197153692530977));
#53915=CARTESIAN_POINT('Ctrl Pts',(-5.59388835734372,-2.45051526468621,
-0.261072313660039));
#53916=CARTESIAN_POINT('Ctrl Pts',(-5.58044921847538,-2.41262907617418,
-0.519611789606023));
#53917=CARTESIAN_POINT('Ctrl Pts',(-5.56701007960703,-2.33245222215829,
-0.764293540131167));
#53918=CARTESIAN_POINT('Ctrl Pts',(-5.52476270667377,-2.08040769122459,
-1.53347683867927));
#53919=CARTESIAN_POINT('Ctrl Pts',(-5.4825153337405,-1.41043556016157,-2.1657144103304));
#53920=CARTESIAN_POINT('Ctrl Pts',(-5.44026796080724,-0.627948022535169,
-2.37279566442992));
#53921=CARTESIAN_POINT('Ctrl Pts',(-5.39802058787398,0.154539515091236,
-2.57987691852945));
#53922=CARTESIAN_POINT('Ctrl Pts',(-5.35577321494072,1.04954245928102,-2.36180185507737));
#53923=CARTESIAN_POINT('Ctrl Pts',(-5.31352584200746,1.64906650734465,-1.81798174866911));
#53924=CARTESIAN_POINT('Ctrl Pts',(-5.2712784690742,2.24859055540828,-1.27416164226085));
#53925=CARTESIAN_POINT('Ctrl Pts',(-5.22903109614093,2.55263570734576,-0.404596492896413));
#53926=CARTESIAN_POINT('Ctrl Pts',(-5.18678372320767,2.42260053111077,0.394315420446647));
#53927=CARTESIAN_POINT('Ctrl Pts',(-5.1445363502744,2.29256535487578,1.19322733378971));
#53928=CARTESIAN_POINT('Ctrl Pts',(-5.10228897734114,1.72844985046831,1.9214860111114));
#53929=CARTESIAN_POINT('Ctrl Pts',(-5.06004160440788,0.987410615361824,
2.24710886714723));
#53930=CARTESIAN_POINT('Ctrl Pts',(-5.01779423147462,0.246371380255345,
2.57273172318307));
#53931=CARTESIAN_POINT('Ctrl Pts',(-4.97554685854136,-0.671591585550147,
2.49571875793305));
#53932=CARTESIAN_POINT('Ctrl Pts',(-4.9332994856081,-1.34801746853503,2.05117695206065));
#53933=CARTESIAN_POINT('Ctrl Pts',(-4.89130882247608,-2.02033315147846,
1.60933633754549));
#53934=CARTESIAN_POINT('Ctrl Pts',(-4.84931815934407,-2.45403816100393,
0.8044197798363));
#53935=CARTESIAN_POINT('Ctrl Pts',(-4.80732749621206,-2.45447688366933,
-9.10453097679518E-5));
#53936=CARTESIAN_POINT('Origin',(-4.85,0.,0.));
#53937=CARTESIAN_POINT('',(-3.89167250378794,-2.44904833524983,0.00209640718090015));
#53938=CARTESIAN_POINT('',(-4.00732749621206,-2.4487999781993,0.00204119660086303));
#53939=CARTESIAN_POINT('',(-4.85,-2.4505,-3.00099698131059E-16));
#53940=CARTESIAN_POINT('Ctrl Pts',(-3.89167250378794,-2.44904833524983,
0.00209640718090015));
#53941=CARTESIAN_POINT('Ctrl Pts',(-3.90411689678976,-2.45101740052764,
0.241894248235633));
#53942=CARTESIAN_POINT('Ctrl Pts',(-3.91656128979158,-2.41863571201545,
0.481171829065209));
#53943=CARTESIAN_POINT('Ctrl Pts',(-3.9290056827934,-2.34972373355784,0.709420313421929));
#53944=CARTESIAN_POINT('Ctrl Pts',(-3.97125305572666,-2.11577499431097,
1.48429931625169));
#53945=CARTESIAN_POINT('Ctrl Pts',(-4.01350042865992,-1.46080395431589,
2.13206474896982));
#53946=CARTESIAN_POINT('Ctrl Pts',(-4.05574780159318,-0.68338443893331,
2.35742752035839));
#53947=CARTESIAN_POINT('Ctrl Pts',(-4.09799517452644,0.0940350764492678,
2.58279029174695));
#53948=CARTESIAN_POINT('Ctrl Pts',(-4.14024254745971,0.993903067219349,
2.38575040180594));
#53949=CARTESIAN_POINT('Ctrl Pts',(-4.18248992039297,1.60600746001602,1.856130071814));
#53950=CARTESIAN_POINT('Ctrl Pts',(-4.22473729332624,2.21811185281269,1.32650974182207));
#53951=CARTESIAN_POINT('Ctrl Pts',(-4.26698466625949,2.54245264763596,0.464308971779215));
#53952=CARTESIAN_POINT('Ctrl Pts',(-4.30923203919276,2.43117648011452,-0.337431070980653));
#53953=CARTESIAN_POINT('Ctrl Pts',(-4.35147941212602,2.31990031259309,-1.13917111374053));
#53954=CARTESIAN_POINT('Ctrl Pts',(-4.39372678505928,1.77300718272696,-1.8804504292174));
#53955=CARTESIAN_POINT('Ctrl Pts',(-4.43597415799255,1.0398027298051,-2.22335086934377));
#53956=CARTESIAN_POINT('Ctrl Pts',(-4.47822153092581,0.306598276883252,
-2.56625130947013));
#53957=CARTESIAN_POINT('Ctrl Pts',(-4.52046890385907,-0.612917499094324,
-2.51077287424597));
#53958=CARTESIAN_POINT('Ctrl Pts',(-4.56271627679233,-1.29957592358191,
-2.08220585532948));
#53959=CARTESIAN_POINT('Ctrl Pts',(-4.60496364972559,-1.98623434806949,
-1.65363883641299));
#53960=CARTESIAN_POINT('Ctrl Pts',(-4.64721102265886,-2.44003542106709,
-0.851983233804166));
#53961=CARTESIAN_POINT('Ctrl Pts',(-4.68945839559212,-2.45411026740558,
-0.0426802124805824));
#53962=CARTESIAN_POINT('Ctrl Pts',(-4.69019643165739,-2.45435614646243,
-0.0285421779472637));
#53963=CARTESIAN_POINT('Ctrl Pts',(-4.69093446772267,-2.45446782996703,
-0.0144018095763991));
#53964=CARTESIAN_POINT('Ctrl Pts',(-4.69167250378794,-2.45444635238797,
-0.00026109281808101));
#53965=CARTESIAN_POINT('Ctrl Pts',(-4.80732749621206,-2.45447688366933,
-9.10453097679518E-5));
#53966=CARTESIAN_POINT('Ctrl Pts',(-4.80707078641081,-2.45447956579912,
-0.00500941998221655));
#53967=CARTESIAN_POINT('Ctrl Pts',(-4.80681407660956,-2.45446605466731,
-0.00992777949047233));
#53968=CARTESIAN_POINT('Ctrl Pts',(-4.80655736680831,-2.45443630579685,
-0.0148460407822334));
#53969=CARTESIAN_POINT('Ctrl Pts',(-4.76430999387504,-2.44954045990948,
-0.824256581257921));
#53970=CARTESIAN_POINT('Ctrl Pts',(-4.72206262094178,-2.00485996797048,
-1.63100701571451));
#53971=CARTESIAN_POINT('Ctrl Pts',(-4.67981524800852,-1.32310601479308,
-2.06733365903014));
#53972=CARTESIAN_POINT('Ctrl Pts',(-4.63756787507526,-0.641352061615665,
-2.50366030234578));
#53973=CARTESIAN_POINT('Ctrl Pts',(-4.59532050214199,0.277475352800151,
-2.56956315452044));
#53974=CARTESIAN_POINT('Ctrl Pts',(-4.55307312920873,1.01452134907151,-2.23499986944486));
#53975=CARTESIAN_POINT('Ctrl Pts',(-4.51082575627547,1.75156734534285,-1.9004365843693));
#53976=CARTESIAN_POINT('Ctrl Pts',(-4.46857838334221,2.30683192346974,-1.16540716204352));
#53977=CARTESIAN_POINT('Ctrl Pts',(-4.42633101040895,2.42719325203068,-0.364980686389968));
#53978=CARTESIAN_POINT('Ctrl Pts',(-4.38408363747569,2.54755458059162,0.435445789263594));
#53979=CARTESIAN_POINT('Ctrl Pts',(-4.34183626454242,2.23301265958659,1.30126931824493));
#53980=CARTESIAN_POINT('Ctrl Pts',(-4.29958889160916,1.62695395780928,1.83779726937138));
#53981=CARTESIAN_POINT('Ctrl Pts',(-4.2573415186759,1.02089525603198,2.37432522049783));
#53982=CARTESIAN_POINT('Ctrl Pts',(-4.21509414574264,0.123319773482412,
2.5815575937694));
#53983=CARTESIAN_POINT('Ctrl Pts',(-4.17284677280938,-0.656605474814574,
2.36502584226545));
#53984=CARTESIAN_POINT('Ctrl Pts',(-4.13059939987611,-1.43653072311158,
2.1484940907615));
#53985=CARTESIAN_POINT('Ctrl Pts',(-4.08835202694285,-2.09880573715599,
1.50819821448203));
#53986=CARTESIAN_POINT('Ctrl Pts',(-4.04610465400958,-2.34152711618347,
0.736022247164297));
#53987=CARTESIAN_POINT('Ctrl Pts',(-4.03317893474374,-2.41578850067437,
0.499772533054371));
#53988=CARTESIAN_POINT('Ctrl Pts',(-4.0202532154779,-2.45077657478841,0.251177871086556));
#53989=CARTESIAN_POINT('Ctrl Pts',(-4.00732749621206,-2.4487999781993,0.00204119660086303));
#53990=CARTESIAN_POINT('Origin',(-4.85,0.,0.));
#53991=CARTESIAN_POINT('',(-3.09167250378794,-2.44725071792797,-0.00132331670171071));
#53992=CARTESIAN_POINT('',(-3.20732749621206,-2.44741005262324,-0.00144229910683621));
#53993=CARTESIAN_POINT('',(-4.85,-2.4505,-3.00099698131059E-16));
#53994=CARTESIAN_POINT('Ctrl Pts',(-3.09167250378794,-2.44725071792797,
-0.00132331670171071));
#53995=CARTESIAN_POINT('Ctrl Pts',(-3.11729932585685,-2.44481399137148,
0.493408423386824));
#53996=CARTESIAN_POINT('Ctrl Pts',(-3.14292614792576,-2.29924344722054,
0.989458790886426));
#53997=CARTESIAN_POINT('Ctrl Pts',(-3.16855296999468,-2.02046507845012,
1.39362824047613));
#53998=CARTESIAN_POINT('Ctrl Pts',(-3.21080034292794,-1.5608820025814,2.05992613020793));
#53999=CARTESIAN_POINT('Ctrl Pts',(-3.2530477158612,-0.739273023463133,
2.47651442222843));
#54000=CARTESIAN_POINT('Ctrl Pts',(-3.29529508879446,0.0698247858651539,
2.45348798741501));
#54001=CARTESIAN_POINT('Ctrl Pts',(-3.33754246172772,0.878922595193441,
2.4304615526016));
#54002=CARTESIAN_POINT('Ctrl Pts',(-3.37978983466098,1.67550923473175,1.96782039095427));
#54003=CARTESIAN_POINT('Ctrl Pts',(-3.42203720759425,2.09645426748447,1.27646320325523));
#54004=CARTESIAN_POINT('Ctrl Pts',(-3.46428458052751,2.5173993002372,0.585106015556197));
#54005=CARTESIAN_POINT('Ctrl Pts',(-3.50653195346077,2.56270272620434,-0.334967198194552));
#54006=CARTESIAN_POINT('Ctrl Pts',(-3.54877932639404,2.21171261350024,-1.06433365094129));
#54007=CARTESIAN_POINT('Ctrl Pts',(-3.5910266993273,1.86072250079615,-1.79370010368804));
#54008=CARTESIAN_POINT('Ctrl Pts',(-3.63327407226056,1.11343884942081,-2.33235979543077));
#54009=CARTESIAN_POINT('Ctrl Pts',(-3.67552144519382,0.310516932425231,
-2.43476036598832));
#54010=CARTESIAN_POINT('Ctrl Pts',(-3.71776881812708,-0.492404984570358,
-2.53716093654587));
#54011=CARTESIAN_POINT('Ctrl Pts',(-3.76001619106035,-1.35096516718619,
-2.20330238591822));
#54012=CARTESIAN_POINT('Ctrl Pts',(-3.80226356399361,-1.87378203924477,
-1.58537682413371));
#54013=CARTESIAN_POINT('Ctrl Pts',(-3.83206654392505,-2.24259788894024,
-1.14946751573524));
#54014=CARTESIAN_POINT('Ctrl Pts',(-3.8618695238565,-2.44433263614344,-0.572193575746662));
#54015=CARTESIAN_POINT('Ctrl Pts',(-3.89167250378794,-2.44904833524983,
0.00209640718090015));
#54016=CARTESIAN_POINT('Ctrl Pts',(-4.00732749621206,-2.4487999781993,0.00204119660086303));
#54017=CARTESIAN_POINT('Ctrl Pts',(-3.97800584254464,-2.44431612090407,
-0.563118786753198));
#54018=CARTESIAN_POINT('Ctrl Pts',(-3.94868418887722,-2.24961307590875,
-1.1310679517478));
#54019=CARTESIAN_POINT('Ctrl Pts',(-3.9193625352098,-1.89164075675834,-1.56402469018496));
#54020=CARTESIAN_POINT('Ctrl Pts',(-3.87711516227654,-1.37586527429514,
-2.18783960186053));
#54021=CARTESIAN_POINT('Ctrl Pts',(-3.83486778934327,-0.521146565358179,
-2.5314133668557));
#54022=CARTESIAN_POINT('Ctrl Pts',(-3.79262041641001,0.282884960559793,
-2.43812511640121));
#54023=CARTESIAN_POINT('Ctrl Pts',(-3.75037304347675,1.08691648647776,-2.34483686594671));
#54024=CARTESIAN_POINT('Ctrl Pts',(-3.70812567054349,1.84026082937673,-1.81468660004255));
#54025=CARTESIAN_POINT('Ctrl Pts',(-3.66587829761023,2.19949990122418,-1.08934758854723));
#54026=CARTESIAN_POINT('Ctrl Pts',(-3.62363092467696,2.55873897307164,-0.364008577051898));
#54027=CARTESIAN_POINT('Ctrl Pts',(-3.5813835517437,2.52387277386756,0.55651918003457));
#54028=CARTESIAN_POINT('Ctrl Pts',(-3.53913617881044,2.11079534144264,1.25260568841855));
#54029=CARTESIAN_POINT('Ctrl Pts',(-3.49688880587718,1.69771790901772,1.94869219680253));
#54030=CARTESIAN_POINT('Ctrl Pts',(-3.45464143294391,0.906429243371915,
2.42033745648402));
#54031=CARTESIAN_POINT('Ctrl Pts',(-3.41239406001065,0.0976446577005888,
2.45253817604351));
#54032=CARTESIAN_POINT('Ctrl Pts',(-3.37014668707739,-0.71113992797075,
2.48473889560299));
#54033=CARTESIAN_POINT('Ctrl Pts',(-3.32789931414413,-1.53742043366764,
2.07749507504048));
#54034=CARTESIAN_POINT('Ctrl Pts',(-3.28565194121086,-2.00453023386089,
1.41645209089424));
#54035=CARTESIAN_POINT('Ctrl Pts',(-3.25954379287793,-2.29319603967271,
1.00793891986703));
#54036=CARTESIAN_POINT('Ctrl Pts',(-3.23343564454499,-2.44469358413537,
0.502499163605551));
#54037=CARTESIAN_POINT('Ctrl Pts',(-3.20732749621206,-2.44741005262324,
-0.00144229910683621));
#54038=CARTESIAN_POINT('Origin',(-4.85,0.,0.));
#54039=CARTESIAN_POINT('',(-2.29167250378794,-2.45380537632986,-0.00115034636150174));
#54040=CARTESIAN_POINT('',(-2.40732749621206,-2.45397025608505,-0.00100410518415028));
#54041=CARTESIAN_POINT('',(-4.85,-2.4505,-3.00099698131059E-16));
#54042=CARTESIAN_POINT('Ctrl Pts',(-2.29167250378794,-2.45380537632986,
-0.00115034636150174));
#54043=CARTESIAN_POINT('Ctrl Pts',(-2.33048175492395,-2.44946767235673,
0.742949817427895));
#54044=CARTESIAN_POINT('Ctrl Pts',(-2.36929100605995,-2.08689533417843,
1.4907108692332));
#54045=CARTESIAN_POINT('Ctrl Pts',(-2.40810025719595,-1.49784486253987,
1.94446383384055));
#54046=CARTESIAN_POINT('Ctrl Pts',(-2.45034763012922,-0.856610254208518,
2.43841489329699));
#54047=CARTESIAN_POINT('Ctrl Pts',(-2.49259500306248,0.0530074563527559,
2.58395791301339));
#54048=CARTESIAN_POINT('Ctrl Pts',(-2.53484237599574,0.816351677303214,
2.31474593648947));
#54049=CARTESIAN_POINT('Ctrl Pts',(-2.577089748929,1.57969589825366,2.04553395996556));
#54050=CARTESIAN_POINT('Ctrl Pts',(-2.61933712186227,2.1967666295933,1.36156698720134));
#54051=CARTESIAN_POINT('Ctrl Pts',(-2.66158449479553,2.38626722282838,0.574636872262373));
#54052=CARTESIAN_POINT('Ctrl Pts',(-2.70383186772879,2.57576781606347,-0.212293242676599));
#54053=CARTESIAN_POINT('Ctrl Pts',(-2.74607924066205,2.337698271194,-1.10218649979031));
#54054=CARTESIAN_POINT('Ctrl Pts',(-2.78832661359532,1.78058449996468,-1.68937788796909));
#54055=CARTESIAN_POINT('Ctrl Pts',(-2.83057398652858,1.22347072873538,-2.27656927614787));
#54056=CARTESIAN_POINT('Ctrl Pts',(-2.87282135946184,0.347312731146226,
-2.56105879539171));
#54057=CARTESIAN_POINT('Ctrl Pts',(-2.9150687323951,-0.44848580650072,-2.41315960659802));
#54058=CARTESIAN_POINT('Ctrl Pts',(-2.95731610532836,-1.24428434414768,
-2.26526041780433));
#54059=CARTESIAN_POINT('Ctrl Pts',(-2.99956347826163,-1.95972342185244,
-1.6849725209731));
#54060=CARTESIAN_POINT('Ctrl Pts',(-3.04181085119489,-2.26866437439522,
-0.936824828835923));
#54061=CARTESIAN_POINT('Ctrl Pts',(-3.05843140205924,-2.39020492139988,
-0.642495834915862));
#54062=CARTESIAN_POINT('Ctrl Pts',(-3.07505195292359,-2.4488310831237,-0.322186903620115));
#54063=CARTESIAN_POINT('Ctrl Pts',(-3.09167250378794,-2.44725071792797,
-0.00132331670171071));
#54064=CARTESIAN_POINT('Ctrl Pts',(-3.20732749621206,-2.44741005262324,
-0.00144229910683621));
#54065=CARTESIAN_POINT('Ctrl Pts',(-3.19118827161173,-2.44908928680278,
-0.312962838534463));
#54066=CARTESIAN_POINT('Ctrl Pts',(-3.1750490470114,-2.3939145395726,-0.62391083234076));
#54067=CARTESIAN_POINT('Ctrl Pts',(-3.15890982241108,-2.27914261217474,
-0.911036188800726));
#54068=CARTESIAN_POINT('Ctrl Pts',(-3.11666244947782,-1.97870609560573,
-1.66263933661953));
#54069=CARTESIAN_POINT('Ctrl Pts',(-3.07441507654455,-1.26989396777807,
-2.25100348452715));
#54070=CARTESIAN_POINT('Ctrl Pts',(-3.03216770361129,-0.475823947375298,
-2.40791809562384));
#54071=CARTESIAN_POINT('Ctrl Pts',(-2.98992033067803,0.318246073027468,
-2.56483270672052));
#54072=CARTESIAN_POINT('Ctrl Pts',(-2.94767295774476,1.19757398600535,-2.29029778100629));
#54073=CARTESIAN_POINT('Ctrl Pts',(-2.9054255848115,1.76131107751761,-1.70946227601724));
#54074=CARTESIAN_POINT('Ctrl Pts',(-2.86317821187824,2.32504816902986,-1.1286267710282));
#54075=CARTESIAN_POINT('Ctrl Pts',(-2.82093083894498,2.57319443907647,-0.241490686764353));
#54076=CARTESIAN_POINT('Ctrl Pts',(-2.77868346601172,2.39263041244319,0.547537845298911));
#54077=CARTESIAN_POINT('Ctrl Pts',(-2.73643609307845,2.21206638580991,1.33656637736216));
#54078=CARTESIAN_POINT('Ctrl Pts',(-2.69418872014519,1.60279206249672,2.02748735722485));
#54079=CARTESIAN_POINT('Ctrl Pts',(-2.65194134721193,0.842550049158391,
2.30533889032187));
#54080=CARTESIAN_POINT('Ctrl Pts',(-2.60969397427867,0.0823080358200451,
2.58319042341891));
#54081=CARTESIAN_POINT('Ctrl Pts',(-2.5674466013454,-0.828901667543443,
2.44797250975027));
#54082=CARTESIAN_POINT('Ctrl Pts',(-2.52519922841214,-1.47569677223535,
1.96132532368679));
#54083=CARTESIAN_POINT('Ctrl Pts',(-2.48590865101211,-2.07722418940753,
1.50873744418155));
#54084=CARTESIAN_POINT('Ctrl Pts',(-2.44661807361209,-2.4500533600519,0.752190332549819));
#54085=CARTESIAN_POINT('Ctrl Pts',(-2.40732749621206,-2.45397025608505,
-0.00100410518415028));
#54086=CARTESIAN_POINT('Origin',(-4.85,0.,0.));
#54087=CARTESIAN_POINT('',(-1.49167250378794,-2.45055445589341,0.00221101876065513));
#54088=CARTESIAN_POINT('',(-1.60732749621206,-2.45027648577636,0.0022158123731987));
#54089=CARTESIAN_POINT('',(-4.85,-2.4505,-3.00099698131059E-16));
#54090=CARTESIAN_POINT('Ctrl Pts',(-1.49167250378794,-2.45055445589341,
0.00221101876065513));
#54091=CARTESIAN_POINT('Ctrl Pts',(-1.50141681105777,-2.45226598486262,
0.189685678637849));
#54092=CARTESIAN_POINT('Ctrl Pts',(-1.51116111832761,-2.43256006628774,
0.376804259058285));
#54093=CARTESIAN_POINT('Ctrl Pts',(-1.52090542559744,-2.39007174190195,
0.558598204251411));
#54094=CARTESIAN_POINT('Ctrl Pts',(-1.5631527985307,-2.20585956181267,1.34678318106949));
#54095=CARTESIAN_POINT('Ctrl Pts',(-1.60540017146397,-1.59339768921037,
2.03487893035977));
#54096=CARTESIAN_POINT('Ctrl Pts',(-1.64764754439723,-0.831879031878564,
2.30921131388054));
#54097=CARTESIAN_POINT('Ctrl Pts',(-1.68989491733049,-0.0703603745467456,
2.58354369740131));
#54098=CARTESIAN_POINT('Ctrl Pts',(-1.73214229026376,0.840215067514576,
2.44411271515255));
#54099=CARTESIAN_POINT('Ctrl Pts',(-1.77438966319702,1.48475269024887,1.95447918093393));
#54100=CARTESIAN_POINT('Ctrl Pts',(-1.81663703613028,2.12929031298315,1.46484564671533));
#54101=CARTESIAN_POINT('Ctrl Pts',(-1.85888440906354,2.5077901163904,0.625009560526885));
#54102=CARTESIAN_POINT('Ctrl Pts',(-1.9011317819968,2.44771067730732,-0.182183072094467));
#54103=CARTESIAN_POINT('Ctrl Pts',(-1.94337915493007,2.38763123822424,-0.989375704715836));
#54104=CARTESIAN_POINT('Ctrl Pts',(-1.98562652786333,1.8889725566508,-1.76392488377011));
#54105=CARTESIAN_POINT('Ctrl Pts',(-2.02787390079659,1.17905181075523,-2.15274610461772));
#54106=CARTESIAN_POINT('Ctrl Pts',(-2.07012127372986,0.469131064859669,
-2.54156732546532));
#54107=CARTESIAN_POINT('Ctrl Pts',(-2.11236864666312,-0.452051745358034,
-2.54466058810626));
#54108=CARTESIAN_POINT('Ctrl Pts',(-2.15461601959638,-1.16456780504994,
-2.16061581497033));
#54109=CARTESIAN_POINT('Ctrl Pts',(-2.19686339252964,-1.87708386474185,
-1.77657104183441));
#54110=CARTESIAN_POINT('Ctrl Pts',(-2.2391107654629,-2.38093317390796,-1.00538823292162));
#54111=CARTESIAN_POINT('Ctrl Pts',(-2.28135813839617,-2.4464320754403,-0.198617278866989));
#54112=CARTESIAN_POINT('Ctrl Pts',(-2.28479626019343,-2.45176242346953,
-0.13296167450759));
#54113=CARTESIAN_POINT('Ctrl Pts',(-2.28823438199068,-2.45418965466927,
-0.0670703761889925));
#54114=CARTESIAN_POINT('Ctrl Pts',(-2.29167250378794,-2.45380537632986,
-0.00115034636150174));
#54115=CARTESIAN_POINT('Ctrl Pts',(-2.40732749621206,-2.45397025608505,
-0.00100410518415028));
#54116=CARTESIAN_POINT('Ctrl Pts',(-2.40437070067883,-2.45426502041435,
-0.0576854292195473));
#54117=CARTESIAN_POINT('Ctrl Pts',(-2.40141390514559,-2.45247054215495,
-0.114347766223135));
#54118=CARTESIAN_POINT('Ctrl Pts',(-2.39845710961236,-2.44852706412429,
-0.170860144323412));
#54119=CARTESIAN_POINT('Ctrl Pts',(-2.35620973667909,-2.39218174530106,
-0.978321967811869));
#54120=CARTESIAN_POINT('Ctrl Pts',(-2.31396236374583,-1.89711060163426,
-1.75516915633047));
#54121=CARTESIAN_POINT('Ctrl Pts',(-2.27171499081257,-1.18899578697325,
-2.14726966381187));
#54122=CARTESIAN_POINT('Ctrl Pts',(-2.22946761787931,-0.480880972312235,
-2.53937017129327));
#54123=CARTESIAN_POINT('Ctrl Pts',(-2.18722024494604,0.440277513342999,
-2.54672399773748));
#54124=CARTESIAN_POINT('Ctrl Pts',(-2.14497287201278,1.15456212339647,-2.16597883548019));
#54125=CARTESIAN_POINT('Ctrl Pts',(-2.10272549907952,1.86884673344991,-1.78523367322291));
#54126=CARTESIAN_POINT('Ctrl Pts',(-2.06047812614626,2.37625746790161,-1.01638952226416));
#54127=CARTESIAN_POINT('Ctrl Pts',(-2.018230753213,2.44548711196819,-0.209930195652571));
#54128=CARTESIAN_POINT('Ctrl Pts',(-1.97598338027973,2.51471675603477,0.596529130959046));
#54129=CARTESIAN_POINT('Ctrl Pts',(-1.93373600734647,2.1457653097162,1.44060363322349));
#54130=CARTESIAN_POINT('Ctrl Pts',(-1.89148863441321,1.50682215458819,1.93751517313379));
#54131=CARTESIAN_POINT('Ctrl Pts',(-1.84924126147994,0.867878999460197,
2.43442671304407));
#54132=CARTESIAN_POINT('Ctrl Pts',(-1.80699388854668,-0.0410558644772366,
2.5841752906002));
#54133=CARTESIAN_POINT('Ctrl Pts',(-1.76474651561342,-0.805636951321461,
2.31849676426623));
#54134=CARTESIAN_POINT('Ctrl Pts',(-1.72249914268016,-1.57021803816568,
2.05281823793226));
#54135=CARTESIAN_POINT('Ctrl Pts',(-1.6802517697469,-2.1904453479167,1.37171260770819));
#54136=CARTESIAN_POINT('Ctrl Pts',(-1.63800439681363,-2.38358365619368,
0.585667450193285));
#54137=CARTESIAN_POINT('Ctrl Pts',(-1.62777876327978,-2.43033121526461,
0.395411603172733));
#54138=CARTESIAN_POINT('Ctrl Pts',(-1.61755312974592,-2.45205807642027,
0.199007950419292));
#54139=CARTESIAN_POINT('Ctrl Pts',(-1.60732749621206,-2.45027648577636,
0.0022158123731987));
#54140=CARTESIAN_POINT('Origin',(-4.85,0.,0.));
#54141=CARTESIAN_POINT('',(-0.691672503787938,-2.44670246171365,-0.000557269204686795));
#54142=CARTESIAN_POINT('',(-0.80732749621206,-2.44672029168306,-0.000703677119379069));
#54143=CARTESIAN_POINT('',(-4.85,-2.4505,-3.00099698131059E-16));
#54144=CARTESIAN_POINT('Ctrl Pts',(-0.691672503787938,-2.44670246171365,
-0.000557269204686795));
#54145=CARTESIAN_POINT('Ctrl Pts',(-0.714599240124866,-2.44575994471511,
0.442323777543362));
#54146=CARTESIAN_POINT('Ctrl Pts',(-0.737525976461795,-2.33087207722529,
0.88564371083638));
#54147=CARTESIAN_POINT('Ctrl Pts',(-0.760452712798723,-2.10494043458978,
1.26235300145016));
#54148=CARTESIAN_POINT('Ctrl Pts',(-0.802700085731985,-1.68861347799314,
1.956519744335));
#54149=CARTESIAN_POINT('Ctrl Pts',(-0.844947458665247,-0.895227651255518,
2.42450421239133));
#54150=CARTESIAN_POINT('Ctrl Pts',(-0.887194831598509,-0.0863207720182636,
2.45296481699518));
#54151=CARTESIAN_POINT('Ctrl Pts',(-0.929442204531771,0.722586107218991,
2.48142542159903));
#54152=CARTESIAN_POINT('Ctrl Pts',(-0.971689577465033,1.54701403895588,
2.07036216275039));
#54153=CARTESIAN_POINT('Ctrl Pts',(-1.0139369503983,2.01107092521102,1.4071652588015));
#54154=CARTESIAN_POINT('Ctrl Pts',(-1.05618432333156,2.47512781146617,0.743968354852607));
#54155=CARTESIAN_POINT('Ctrl Pts',(-1.09843169626482,2.57881365223958,-0.171362194196542));
#54156=CARTESIAN_POINT('Ctrl Pts',(-1.14067906919808,2.27489910948537,-0.921567533298358));
#54157=CARTESIAN_POINT('Ctrl Pts',(-1.18292644213135,1.97098456673116,-1.67177287240018));
#54158=CARTESIAN_POINT('Ctrl Pts',(-1.22517381506461,1.25946964044931,-2.25685300155467));
#54159=CARTESIAN_POINT('Ctrl Pts',(-1.26742118799787,0.46468490875651,-2.41009340789012));
#54160=CARTESIAN_POINT('Ctrl Pts',(-1.30966856093113,-0.330099822936278,
-2.56333381422556));
#54161=CARTESIAN_POINT('Ctrl Pts',(-1.3519159338644,-1.20815436004001,-2.28473449774198));
#54162=CARTESIAN_POINT('Ctrl Pts',(-1.39416330679766,-1.76920038480375,
-1.70129773732726));
#54163=CARTESIAN_POINT('Ctrl Pts',(-1.42666637246109,-2.20084179862391,
-1.25242998490692));
#54164=CARTESIAN_POINT('Ctrl Pts',(-1.45916943812451,-2.44484548788464,
-0.623128578142306));
#54165=CARTESIAN_POINT('Ctrl Pts',(-1.49167250378794,-2.45055445589341,
0.00221101876065513));
#54166=CARTESIAN_POINT('Ctrl Pts',(-1.60732749621206,-2.45027648577636,
0.0022158123731987));
#54167=CARTESIAN_POINT('Ctrl Pts',(-1.57530575681265,-2.44469740540674,
-0.614042000846752));
#54168=CARTESIAN_POINT('Ctrl Pts',(-1.54328401741325,-2.20858515756784,
-1.2341094543524));
#54169=CARTESIAN_POINT('Ctrl Pts',(-1.51126227801385,-1.78837913807019,
-1.68112422477864));
#54170=CARTESIAN_POINT('Ctrl Pts',(-1.46901490508058,-1.23398700486683,
-2.27088605742987));
#54171=CARTESIAN_POINT('Ctrl Pts',(-1.42676753214732,-0.359153431657199,
-2.55942503792661));
#54172=CARTESIAN_POINT('Ctrl Pts',(-1.38452015921406,0.437320224845424,
-2.41520802829028));
#54173=CARTESIAN_POINT('Ctrl Pts',(-1.3422727862808,1.23379388134807,-2.27099101865394));
#54174=CARTESIAN_POINT('Ctrl Pts',(-1.30002541334753,1.9519076211437,-1.69401801888449));
#54175=CARTESIAN_POINT('Ctrl Pts',(-1.25777804041427,2.2643062266558,-0.947307427860767));
#54176=CARTESIAN_POINT('Ctrl Pts',(-1.21553066748101,2.57670483216789,-0.200596836837063));
#54177=CARTESIAN_POINT('Ctrl Pts',(-1.17328329454775,2.48338830339646,0.715851345440913));
#54178=CARTESIAN_POINT('Ctrl Pts',(-1.13103592161449,2.02689055186718,1.38426799228393));
#54179=CARTESIAN_POINT('Ctrl Pts',(-1.08878854868123,1.57039280033789,2.05268463912697));
#54180=CARTESIAN_POINT('Ctrl Pts',(-1.04654117574796,0.75071382605072,2.47306975053505));
#54181=CARTESIAN_POINT('Ctrl Pts',(-1.0042938028147,-0.0584792284292852,
2.45378517339887));
#54182=CARTESIAN_POINT('Ctrl Pts',(-0.962046429881436,-0.867672282909301,
2.43450059626269));
#54183=CARTESIAN_POINT('Ctrl Pts',(-0.919799056948171,-1.66637941758216,
1.97554633058223));
#54184=CARTESIAN_POINT('Ctrl Pts',(-0.877551684014908,-2.09052238902825,
1.2861445967215));
#54185=CARTESIAN_POINT('Ctrl Pts',(-0.854143621413959,-2.32552789441308,
0.904166787854964));
#54186=CARTESIAN_POINT('Ctrl Pts',(-0.830735558813009,-2.44554401588084,
0.451442722424482));
#54187=CARTESIAN_POINT('Ctrl Pts',(-0.80732749621206,-2.44672029168306,
-0.000703677119379069));
#54188=CARTESIAN_POINT('Origin',(-4.85,0.,0.));
#54189=CARTESIAN_POINT('',(1.11022302462516E-15,-2.4505,-3.00099698131059E-16));
#54190=CARTESIAN_POINT('',(-0.00732749621205394,-2.45343455551405,-0.00158943503992818));
#54191=CARTESIAN_POINT('',(-4.85,-2.4505,-3.00099698131059E-16));
#54192=CARTESIAN_POINT('',(0.,-1.6158113816168,1.84230937386683));
#54193=CARTESIAN_POINT('Origin',(0.,0.,0.));
#54194=CARTESIAN_POINT('Ctrl Pts',(-1.73472347597681E-17,-1.6158113816168,
1.84230937386684));
#54195=CARTESIAN_POINT('Ctrl Pts',(-0.0422473729332622,-1.00451454043688,
2.37845189560396));
#54196=CARTESIAN_POINT('Ctrl Pts',(-0.0844947458665235,-0.110745570517432,
2.58195950654786));
#54197=CARTESIAN_POINT('Ctrl Pts',(-0.126742118799786,0.666815391991473,
2.36197006147115));
#54198=CARTESIAN_POINT('Ctrl Pts',(-0.168989491733048,1.44437635450039,
2.14198061639443));
#54199=CARTESIAN_POINT('Ctrl Pts',(-0.211236864666312,2.10572930959876,
1.49849411529711));
#54200=CARTESIAN_POINT('Ctrl Pts',(-0.253484237599575,2.34539034598602,
0.72516513771482));
#54201=CARTESIAN_POINT('Ctrl Pts',(-0.295731610532837,2.58505138237327,
-0.0481638398674565));
#54202=CARTESIAN_POINT('Ctrl Pts',(-0.337978983466098,2.40302050004942,
-0.951335293934691));
#54203=CARTESIAN_POINT('Ctrl Pts',(-0.38022635639936,1.88411977415752,-1.57274369054247));
#54204=CARTESIAN_POINT('Ctrl Pts',(-0.422473729332622,1.36521904826563,
-2.19415208715025));
#54205=CARTESIAN_POINT('Ctrl Pts',(-0.464721102265886,0.509448478805686,
-2.53379742629858));
#54206=CARTESIAN_POINT('Ctrl Pts',(-0.506968475199148,-0.294017051498195,
-2.43679826444183));
#54207=CARTESIAN_POINT('Ctrl Pts',(-0.54921584813241,-1.09748258180206,
-2.33979910258508));
#54208=CARTESIAN_POINT('Ctrl Pts',(-0.591463221065671,-1.84864307294988,
-1.80615543972326));
#54209=CARTESIAN_POINT('Ctrl Pts',(-0.633710593998932,-2.20458927529597,
-1.07915909943569));
#54210=CARTESIAN_POINT('Ctrl Pts',(-0.653031230595267,-2.36737116552707,
-0.746687962833883));
#54211=CARTESIAN_POINT('Ctrl Pts',(-0.672351867191602,-2.44749673212994,
-0.373778456637334));
#54212=CARTESIAN_POINT('Ctrl Pts',(-0.691672503787938,-2.44670246171365,
-0.000557269204686795));
#54213=CARTESIAN_POINT('Ctrl Pts',(-0.80732749621206,-2.44672029168306,
-0.000703677119379069));
#54214=CARTESIAN_POINT('Ctrl Pts',(-0.788488185879749,-2.44766698365207,
-0.364600787352598));
#54215=CARTESIAN_POINT('Ctrl Pts',(-0.769648875547439,-2.3716366477106,
-0.728123721712155));
#54216=CARTESIAN_POINT('Ctrl Pts',(-0.750809565215128,-2.21662198793308,
-1.05409038924796));
#54217=CARTESIAN_POINT('Ctrl Pts',(-0.708562192281865,-1.86899980717248,
-1.78507443931583));
#54218=CARTESIAN_POINT('Ctrl Pts',(-0.6663148193486,-1.12417663743191,-2.32719333741056));
#54219=CARTESIAN_POINT('Ctrl Pts',(-0.624067446415337,-0.321754636452474,
-2.43330246521825));
#54220=CARTESIAN_POINT('Ctrl Pts',(-0.581820073482074,0.48066736452695,
-2.53941159302594));
#54221=CARTESIAN_POINT('Ctrl Pts',(-0.539572700548812,1.34068819674525,
-2.20951095054658));
#54222=CARTESIAN_POINT('Ctrl Pts',(-0.49732532761555,1.86639110685498,-1.59401768292883));
#54223=CARTESIAN_POINT('Ctrl Pts',(-0.455077954682288,2.39209401696471,
-0.978524415311086));
#54224=CARTESIAN_POINT('Ctrl Pts',(-0.412830581749026,2.58347900496592,
-0.0774385225549623));
#54225=CARTESIAN_POINT('Ctrl Pts',(-0.370583208815764,2.35305240108692,
0.698528605099877));
#54226=CARTESIAN_POINT('Ctrl Pts',(-0.328335835882501,2.1226257972079,1.47449573275474));
#54227=CARTESIAN_POINT('Ctrl Pts',(-0.286088462949239,1.47038760144866,
2.12534409530829));
#54228=CARTESIAN_POINT('Ctrl Pts',(-0.243841090015977,0.694141965819649,
2.35427235402313));
#54229=CARTESIAN_POINT('Ctrl Pts',(-0.201593717082716,-0.0821036698093253,
2.58320061273796));
#54230=CARTESIAN_POINT('Ctrl Pts',(-0.159346344149453,-0.98235674530807,
2.39020876761409));
#54231=CARTESIAN_POINT('Ctrl Pts',(-0.117098971216192,-1.59714394385247,
1.86348026693122));
#54232=CARTESIAN_POINT('Ctrl Pts',(-0.0805084795481457,-2.12961174727059,
1.40728018921266));
#54233=CARTESIAN_POINT('Ctrl Pts',(-0.0439179878800999,-2.44794276668283,
0.700733923400609));
#54234=CARTESIAN_POINT('Ctrl Pts',(-0.00732749621205394,-2.45343455551405,
-0.00158943503992818));
#54235=CARTESIAN_POINT('Origin',(-11.2285451186048,0.,0.));
#54236=CARTESIAN_POINT('',(-0.428545118604763,-1.99165873719784,-0.000453626911316259));
#54237=CARTESIAN_POINT('',(-0.270454881395215,-1.99713877968237,-0.00129382801318301));
#54238=CARTESIAN_POINT('',(-11.2285451186048,-1.99475,-1.35786321299982E-13));
#54239=CARTESIAN_POINT('',(0.,1.94482913246214,0.443471766887781));
#54240=CARTESIAN_POINT('Ctrl Pts',(-0.428545118604763,-1.99165873719784,
-0.00045362691131607));
#54241=CARTESIAN_POINT('Ctrl Pts',(-0.409224482008429,-1.99230528725411,
-0.304262222557603));
#54242=CARTESIAN_POINT('Ctrl Pts',(-0.347656472478832,-1.78446077518961,
-1.27158386090278));
#54243=CARTESIAN_POINT('Ctrl Pts',(-0.243841090015977,-0.281912258858396,
-2.33903283263629));
#54244=CARTESIAN_POINT('Ctrl Pts',(-0.120313353744052,1.75492292348853,
-1.53063674963699));
#54245=CARTESIAN_POINT('Ctrl Pts',(-0.039032990405396,2.08014183670335,
-0.149753151782914));
#54246=CARTESIAN_POINT('Ctrl Pts',(-3.31223763694322E-16,1.94778769460277,
0.44492227130092));
#54247=CARTESIAN_POINT('',(0.,1.04832369103675,-1.69706953343435));
#54248=CARTESIAN_POINT('Origin',(0.,0.,0.));
#54249=CARTESIAN_POINT('Ctrl Pts',(-0.270454881395215,-1.99713877968237,
-0.00129382801318285));
#54250=CARTESIAN_POINT('Ctrl Pts',(-0.264798000130001,-1.99782990438245,
-0.0896790582877039));
#54251=CARTESIAN_POINT('Ctrl Pts',(-0.216893745931524,-1.95213957343271,
-0.837457295748683));
#54252=CARTESIAN_POINT('Ctrl Pts',(-0.126742118799788,-1.00466619559831,
-2.13028476617671));
#54253=CARTESIAN_POINT('Ctrl Pts',(-0.04224737293326,0.485218894542327,
-2.04491391286112));
#54254=CARTESIAN_POINT('Ctrl Pts',(2.22044604925031E-15,1.04832369103677,
-1.69706953343434));
#54255=CARTESIAN_POINT('Origin',(-11.2285451186048,0.,0.));
#54256=CARTESIAN_POINT('',(-1.22854511860476,-1.99479432805279,0.00179980806883705));
#54257=CARTESIAN_POINT('',(-1.07045488139522,-1.99167325110581,-0.000572805523073594));
#54258=CARTESIAN_POINT('',(-11.2285451186048,-1.99475,-1.35786321299982E-13));
#54259=CARTESIAN_POINT('Ctrl Pts',(-1.22854511860476,-1.99479432805279,
0.00179980806883711));
#54260=CARTESIAN_POINT('Ctrl Pts',(-1.19604205294134,-1.99014712791588,
-0.507237596918782));
#54261=CARTESIAN_POINT('Ctrl Pts',(-1.12129161434465,-1.53335398106482,
-1.68533687396134));
#54262=CARTESIAN_POINT('Ctrl Pts',(-1.0042938028147,0.446044752534434,-2.31338343704634));
#54263=CARTESIAN_POINT('Ctrl Pts',(-0.87755168401491,2.18360165830961,-0.884586961676926));
#54264=CARTESIAN_POINT('Ctrl Pts',(-0.750809565215123,1.93039537687792,
1.35069842422285));
#54265=CARTESIAN_POINT('Ctrl Pts',(-0.624067446415335,-0.0829010322208286,
2.35453654165394));
#54266=CARTESIAN_POINT('Ctrl Pts',(-0.516645964211884,-1.72503897850329,
1.38590939031426));
#54267=CARTESIAN_POINT('Ctrl Pts',(-0.451471854941692,-1.99089151182228,
0.360059316569889));
#54268=CARTESIAN_POINT('Ctrl Pts',(-0.428545118604763,-1.99165873719784,
-0.00045362691131607));
#54269=CARTESIAN_POINT('Ctrl Pts',(-1.07045488139522,-1.99167325110581,
-0.000572805523073629));
#54270=CARTESIAN_POINT('Ctrl Pts',(-1.05161557106291,-1.99244387498058,
-0.296791438715318));
#54271=CARTESIAN_POINT('Ctrl Pts',(-0.990528887797343,-1.79176473937272,
-1.25629618557132));
#54272=CARTESIAN_POINT('Ctrl Pts',(-0.887194831598507,-0.308800379382655,
-2.3356705087836));
#54273=CARTESIAN_POINT('Ctrl Pts',(-0.760452712798722,1.7914157663844,-1.5300357731145));
#54274=CARTESIAN_POINT('Ctrl Pts',(-0.633710593998933,2.25878798203272,
0.670463412246034));
#54275=CARTESIAN_POINT('Ctrl Pts',(-0.506968475199148,0.665987972658192,
2.25986937576817));
#54276=CARTESIAN_POINT('Ctrl Pts',(-0.385883237664576,-1.43435331803907,
1.80960849678481));
#54277=CARTESIAN_POINT('Ctrl Pts',(-0.307045373063264,-1.99266836720697,
0.570409709733958));
#54278=CARTESIAN_POINT('Ctrl Pts',(-0.270454881395215,-1.99713877968237,
-0.00129382801318285));
#54279=CARTESIAN_POINT('Origin',(-11.2285451186048,0.,0.));
#54280=CARTESIAN_POINT('',(-2.02854511860477,-1.9974406343334,-0.000936402123948542));
#54281=CARTESIAN_POINT('',(-1.87045488139522,-1.99456805549986,0.00180371015347854));
#54282=CARTESIAN_POINT('',(-11.2285451186048,-1.99475,-1.35786321299982E-13));
#54283=CARTESIAN_POINT('Ctrl Pts',(-2.02854511860477,-1.9974406343334,-0.000936402123948733));
#54284=CARTESIAN_POINT('Ctrl Pts',(-2.02510699680751,-1.99775344364478,
-0.0545964631312387));
#54285=CARTESIAN_POINT('Ctrl Pts',(-1.97942150207699,-1.97149905031364,
-0.767316398232434));
#54286=CARTESIAN_POINT('Ctrl Pts',(-1.89148863441321,-1.11783702498862,
-2.07391634106428));
#54287=CARTESIAN_POINT('Ctrl Pts',(-1.76474651561342,1.13173989076134,-2.06636243085856));
#54288=CARTESIAN_POINT('Ctrl Pts',(-1.63800439681363,2.34949064171247,-0.174872561543903));
#54289=CARTESIAN_POINT('Ctrl Pts',(-1.51126227801384,1.42517419668494,1.87605137184651));
#54290=CARTESIAN_POINT('Ctrl Pts',(-1.38452015921406,-0.798498967630685,
2.21654917046805));
#54291=CARTESIAN_POINT('Ctrl Pts',(-1.2902811060777,-1.91059945294607,0.967113652992006));
#54292=CARTESIAN_POINT('Ctrl Pts',(-1.2382894258746,-1.99618754266669,0.154407470909096));
#54293=CARTESIAN_POINT('Ctrl Pts',(-1.22854511860476,-1.99479432805279,
0.00179980806883711));
#54294=CARTESIAN_POINT('Ctrl Pts',(-1.87045488139522,-1.99456805549986,
0.0018037101534785));
#54295=CARTESIAN_POINT('Ctrl Pts',(-1.83843314199582,-1.99002658618038,
-0.49984096355409));
#54296=CARTESIAN_POINT('Ctrl Pts',(-1.76416402966316,-1.54425170067928,
-1.67051508410203));
#54297=CARTESIAN_POINT('Ctrl Pts',(-1.64764754439723,0.419772684089712,
-2.31829268547235));
#54298=CARTESIAN_POINT('Ctrl Pts',(-1.52090542559744,2.17344423984237,-0.909294246839299));
#54299=CARTESIAN_POINT('Ctrl Pts',(-1.39416330679766,1.94556036418415,1.3287204582401));
#54300=CARTESIAN_POINT('Ctrl Pts',(-1.26742118799787,-0.0561388408262527,
2.35532303034526));
#54301=CARTESIAN_POINT('Ctrl Pts',(-1.15951837953039,-1.71669807082336,
1.4011300490413));
#54302=CARTESIAN_POINT('Ctrl Pts',(-1.09386294399617,-1.9907157419622,0.367482297717186));
#54303=CARTESIAN_POINT('Ctrl Pts',(-1.07045488139522,-1.99167325110581,
-0.000572805523073629));
#54304=CARTESIAN_POINT('Origin',(-11.2285451186048,0.,0.));
#54305=CARTESIAN_POINT('',(-2.82854511860477,-1.99210502737679,-0.00107720301609401));
#54306=CARTESIAN_POINT('',(-2.67045488139522,-1.99757484934734,-0.000817359239539128));
#54307=CARTESIAN_POINT('',(-11.2285451186048,-1.99475,-1.35786321299982E-13));
#54308=CARTESIAN_POINT('Ctrl Pts',(-2.82854511860477,-1.99210502737679,
-0.00107720301609413));
#54309=CARTESIAN_POINT('Ctrl Pts',(-2.81192456774042,-1.99339147237746,
-0.262265793101971));
#54310=CARTESIAN_POINT('Ctrl Pts',(-2.7530566439428,-1.82436351865471,-1.18576413623229));
#54311=CARTESIAN_POINT('Ctrl Pts',(-2.65194134721193,-0.43048932676473,
-2.31632626019967));
#54312=CARTESIAN_POINT('Ctrl Pts',(-2.52519922841214,1.7091346263358,-1.62158787801847));
#54313=CARTESIAN_POINT('Ctrl Pts',(-2.39845710961236,2.29051298743969,0.551578301896968));
#54314=CARTESIAN_POINT('Ctrl Pts',(-2.27171499081256,0.783593777474662,
2.22186165499399));
#54315=CARTESIAN_POINT('Ctrl Pts',(-2.14841099381004,-1.37748262398157,
1.8760794855684));
#54316=CARTESIAN_POINT('Ctrl Pts',(-2.06735436974077,-1.99390966718369,
0.604774188253086));
#54317=CARTESIAN_POINT('Ctrl Pts',(-2.02854511860477,-1.9974406343334,-0.000936402123948733));
#54318=CARTESIAN_POINT('Ctrl Pts',(-2.67045488139522,-1.99757484934734,
-0.000817359239538885));
#54319=CARTESIAN_POINT('Ctrl Pts',(-2.66749808586199,-1.99781479268375,
-0.0469569516163979));
#54320=CARTESIAN_POINT('Ctrl Pts',(-2.62229391739549,-1.97548271348753,
-0.752113333853607));
#54321=CARTESIAN_POINT('Ctrl Pts',(-2.53484237599575,-1.14128472098778,
-2.06110573511026));
#54322=CARTESIAN_POINT('Ctrl Pts',(-2.40810025719595,1.1082327929001,-2.07906416640946));
#54323=CARTESIAN_POINT('Ctrl Pts',(-2.28135813839617,2.34735651770835,-0.201506276029945));
#54324=CARTESIAN_POINT('Ctrl Pts',(-2.15461601959638,1.44635766333907,1.8597680925381));
#54325=CARTESIAN_POINT('Ctrl Pts',(-2.02787390079659,-0.773309122834207,
2.22546200204237));
#54326=CARTESIAN_POINT('Ctrl Pts',(-1.93315352139621,-1.90526206476071,
0.982402385392531));
#54327=CARTESIAN_POINT('Ctrl Pts',(-1.88068051492908,-1.99601830154637,
0.161995963721133));
#54328=CARTESIAN_POINT('Ctrl Pts',(-1.87045488139522,-1.99456805549986,
0.0018037101534785));
#54329=CARTESIAN_POINT('Origin',(-11.2285451186048,0.,0.));
#54330=CARTESIAN_POINT('',(-3.62854511860477,-1.99356831942036,0.00170651223176268));
#54331=CARTESIAN_POINT('',(-3.47045488139522,-1.99223472861465,-0.00117405678175919));
#54332=CARTESIAN_POINT('',(-11.2285451186048,-1.99475,-1.35786321299982E-13));
#54333=CARTESIAN_POINT('Ctrl Pts',(-3.62854511860477,-1.99356831942036,
0.00170651223176254));
#54334=CARTESIAN_POINT('Ctrl Pts',(-3.59874213867332,-1.9897296575993,-0.465775611189874));
#54335=CARTESIAN_POINT('Ctrl Pts',(-3.52669178580862,-1.59272930081482,
-1.60181173444131));
#54336=CARTESIAN_POINT('Ctrl Pts',(-3.41239406001065,0.298056756295131,
-2.33706024159941));
#54337=CARTESIAN_POINT('Ctrl Pts',(-3.28565194121087,2.12296277169725,-1.02162491806891));
#54338=CARTESIAN_POINT('Ctrl Pts',(-3.15890982241107,2.0123294206081,1.22524230469704));
#54339=CARTESIAN_POINT('Ctrl Pts',(-3.03216770361129,0.067022912688436,
2.35503637594289));
#54340=CARTESIAN_POINT('Ctrl Pts',(-2.92204613567585,-1.67627504640892,
1.47111526782332));
#54341=CARTESIAN_POINT('Ctrl Pts',(-2.85417194067368,-1.99012148920151,
0.40164311469117));
#54342=CARTESIAN_POINT('Ctrl Pts',(-2.82854511860477,-1.99210502737679,
-0.00107720301609413));
#54343=CARTESIAN_POINT('Ctrl Pts',(-3.47045488139522,-1.99223472861465,
-0.00117405678175954));
#54344=CARTESIAN_POINT('Ctrl Pts',(-3.4543156567949,-1.99360165470304,-0.254757242263571));
#54345=CARTESIAN_POINT('Ctrl Pts',(-3.39592905926131,-1.83111989225785,
-1.17045474154989));
#54346=CARTESIAN_POINT('Ctrl Pts',(-3.29529508879446,-0.456730463269167,
-2.31129507643307));
#54347=CARTESIAN_POINT('Ctrl Pts',(-3.16855296999467,1.69063459008238,-1.64086633568406));
#54348=CARTESIAN_POINT('Ctrl Pts',(-3.04181085119489,2.29662084453102,0.525566682988035));
#54349=CARTESIAN_POINT('Ctrl Pts',(-2.9150687323951,0.808740873387587,2.21283208749455));
#54350=CARTESIAN_POINT('Ctrl Pts',(-2.79128340912855,-1.36456848198966,
1.8903263506637));
#54351=CARTESIAN_POINT('Ctrl Pts',(-2.70974545879525,-1.99438642724492,
0.612296129709636));
#54352=CARTESIAN_POINT('Ctrl Pts',(-2.67045488139522,-1.99757484934734,
-0.000817359239538885));
#54353=CARTESIAN_POINT('Origin',(-11.2285451186048,0.,0.));
#54354=CARTESIAN_POINT('',(-4.42854511860477,-1.99796240009219,-0.000212534135467141));
#54355=CARTESIAN_POINT('',(-4.27045488139522,-1.9933661524232,0.00166156985075161));
#54356=CARTESIAN_POINT('',(-11.2285451186048,-1.99475,-1.35786321299982E-13));
#54357=CARTESIAN_POINT('Ctrl Pts',(-4.42854511860477,-1.99796240009219,
-0.000212534135467313));
#54358=CARTESIAN_POINT('Ctrl Pts',(-4.42780708253949,-1.99797988321841,
-0.0117233257101024));
#54359=CARTESIAN_POINT('Ctrl Pts',(-4.38482167354096,-1.99268487938393,
-0.682129443554957));
#54360=CARTESIAN_POINT('Ctrl Pts',(-4.29958889160916,-1.24742757618837,
-1.9986527574939));
#54361=CARTESIAN_POINT('Ctrl Pts',(-4.17284677280937,0.998078354190639,
-2.13413401682469));
#54362=CARTESIAN_POINT('Ctrl Pts',(-4.04610465400959,2.33362016704573,-0.323890905768756));
#54363=CARTESIAN_POINT('Ctrl Pts',(-3.9193625352098,1.54156287203605,1.78164876292292));
#54364=CARTESIAN_POINT('Ctrl Pts',(-3.79262041641001,-0.655962132561314,
2.26283054679536));
#54365=CARTESIAN_POINT('Ctrl Pts',(-3.69568127754167,-1.87932505480736,
1.05292634598367));
#54366=CARTESIAN_POINT('Ctrl Pts',(-3.64098951160659,-1.99517117310856,
0.196906162688389));
#54367=CARTESIAN_POINT('Ctrl Pts',(-3.62854511860477,-1.99356831942036,
0.00170651223176254));
#54368=CARTESIAN_POINT('Ctrl Pts',(-4.27045488139522,-1.9933661524232,0.00166156985075149));
#54369=CARTESIAN_POINT('Ctrl Pts',(-4.24113322772781,-1.98971621390464,
-0.458388573709922));
#54370=CARTESIAN_POINT('Ctrl Pts',(-4.16956420112713,-1.60286571508947,
-1.58683223921642));
#54371=CARTESIAN_POINT('Ctrl Pts',(-4.05574780159318,0.271533578210096,
-2.34028997398879));
#54372=CARTESIAN_POINT('Ctrl Pts',(-3.9290056827934,2.11124012136177,-1.04563511631196));
#54373=CARTESIAN_POINT('Ctrl Pts',(-3.80226356399361,2.02609502746784,1.20234212520804));
#54374=CARTESIAN_POINT('Ctrl Pts',(-3.67552144519382,0.0937264506913446,
2.35412467784988));
#54375=CARTESIAN_POINT('Ctrl Pts',(-3.56491855099436,-1.66714663971742,
1.48625392461337));
#54376=CARTESIAN_POINT('Ctrl Pts',(-3.49656302972816,-1.99002347559849,
0.409043136748388));
#54377=CARTESIAN_POINT('Ctrl Pts',(-3.47045488139522,-1.99223472861465,
-0.00117405678175954));
#54378=CARTESIAN_POINT('Origin',(-11.2285451186048,0.,0.));
#54379=CARTESIAN_POINT('',(-5.22854511860477,-1.99297224531778,-0.00154381507001048));
#54380=CARTESIAN_POINT('',(-5.07045488139522,-1.99798725309096,-7.41124799008563E-5));
#54381=CARTESIAN_POINT('',(-11.2285451186048,-1.99475,-1.35786321299982E-13));
#54382=CARTESIAN_POINT('Ctrl Pts',(-5.22854511860477,-1.99297224531778,
-0.00154381507001065));
#54383=CARTESIAN_POINT('Ctrl Pts',(-5.2146246534724,-1.99456009233844,-0.220061877529497));
#54384=CARTESIAN_POINT('Ctrl Pts',(-5.15845681540677,-1.86083331804391,
-1.09987363392612));
#54385=CARTESIAN_POINT('Ctrl Pts',(-5.06004160440788,-0.576882037049555,
-2.28427133200172));
#54386=CARTESIAN_POINT('Ctrl Pts',(-4.93329948560809,1.60258234133143,-1.72696793314944));
#54387=CARTESIAN_POINT('Ctrl Pts',(-4.80655736680831,2.32094657675149,0.404839956945686));
#54388=CARTESIAN_POINT('Ctrl Pts',(-4.67981524800852,0.923266420793207,
2.16754873511761));
#54389=CARTESIAN_POINT('Ctrl Pts',(-4.55381116527401,-1.30313007054563,
1.95531152992337));
#54390=CARTESIAN_POINT('Ctrl Pts',(-4.47005445547276,-1.99697909722901,
0.647188517886537));
#54391=CARTESIAN_POINT('Ctrl Pts',(-4.42854511860477,-1.99796240009219,
-0.000212534135467313));
#54392=CARTESIAN_POINT('Ctrl Pts',(-5.07045488139522,-1.99798725309096,
-7.4112479900871E-5));
#54393=CARTESIAN_POINT('Ctrl Pts',(-5.07019817159397,-1.99798943639167,
-0.00407775576811743));
#54394=CARTESIAN_POINT('Ctrl Pts',(-5.02769408885946,-1.99616842066926,
-0.666968927304851));
#54395=CARTESIAN_POINT('Ctrl Pts',(-4.9429426331917,-1.27001347064424,-1.98437734084019));
#54396=CARTESIAN_POINT('Ctrl Pts',(-4.8162005143919,0.973811444563989,-2.14531557512957));
#54397=CARTESIAN_POINT('Ctrl Pts',(-4.68945839559212,2.3297967747643,-0.350335032157474));
#54398=CARTESIAN_POINT('Ctrl Pts',(-4.56271627679233,1.5616688454542,1.76405160457239));
#54399=CARTESIAN_POINT('Ctrl Pts',(-4.43597415799255,-0.630257733385777,
2.270123969294));
#54400=CARTESIAN_POINT('Ctrl Pts',(-4.33855369286017,-1.87340513851435,
1.06823330419032));
#54401=CARTESIAN_POINT('Ctrl Pts',(-4.28338060066107,-1.99497513673096,
0.204463194592811));
#54402=CARTESIAN_POINT('Ctrl Pts',(-4.27045488139522,-1.9933661524232,0.00166156985075149));
#54403=CARTESIAN_POINT('Origin',(-11.2285451186048,0.,0.));
#54404=CARTESIAN_POINT('',(-6.02854511860477,-1.99253871694387,0.00135657260398031));
#54405=CARTESIAN_POINT('',(-5.87045488139522,-1.99315854296458,-0.00160486565277951));
#54406=CARTESIAN_POINT('',(-11.2285451186048,-1.99475,-1.35786321299982E-13));
#54407=CARTESIAN_POINT('Ctrl Pts',(-6.02854511860477,-1.99253871694387,
0.00135657260398022));
#54408=CARTESIAN_POINT('Ctrl Pts',(-6.00144222440531,-1.98986087355467,
-0.424327265469242));
#54409=CARTESIAN_POINT('Ctrl Pts',(-5.93209195727259,-1.64787261177768,
-1.51748486420009));
#54410=CARTESIAN_POINT('Ctrl Pts',(-5.82049431720661,0.148871987083987,
-2.35128167908273));
#54411=CARTESIAN_POINT('Ctrl Pts',(-5.69375219840681,2.05371677028819,-1.15452840168687));
#54412=CARTESIAN_POINT('Ctrl Pts',(-5.56701007960703,2.08615488253003,1.09482702239254));
#54413=CARTESIAN_POINT('Ctrl Pts',(-5.44026796080724,0.216611974209998,
2.34601100924763));
#54414=CARTESIAN_POINT('Ctrl Pts',(-5.32744630713982,-1.62339131927296,
1.55579902148089));
#54415=CARTESIAN_POINT('Ctrl Pts',(-5.25687202640566,-1.98974111792884,
0.443120996720471));
#54416=CARTESIAN_POINT('Ctrl Pts',(-5.22854511860477,-1.99297224531778,
-0.00154381507001065));
#54417=CARTESIAN_POINT('Ctrl Pts',(-5.87045488139522,-1.99315854296458,
-0.00160486565277954));
#54418=CARTESIAN_POINT('Ctrl Pts',(-5.85701574252688,-1.99476242572242,
-0.212517444469958));
#54419=CARTESIAN_POINT('Ctrl Pts',(-5.80132923072528,-1.86697348923956,
-1.08456306234651));
#54420=CARTESIAN_POINT('Ctrl Pts',(-5.70339534599041,-0.60275022452326,
-2.27758201022554));
#54421=CARTESIAN_POINT('Ctrl Pts',(-5.57665322719063,1.58289408021768,-1.74503122529871));
#54422=CARTESIAN_POINT('Ctrl Pts',(-5.44991110839084,2.32538834689053,0.378492645374279));
#54423=CARTESIAN_POINT('Ctrl Pts',(-5.32316898959105,0.947788588779759,
2.15693867261862));
#54424=CARTESIAN_POINT('Ctrl Pts',(-5.19668358059252,-1.28938481843638,
1.96924988310733));
#54425=CARTESIAN_POINT('Ctrl Pts',(-5.11244554452723,-1.99763012514291,
0.654811816293906));
#54426=CARTESIAN_POINT('Ctrl Pts',(-5.07045488139522,-1.99798725309096,
-7.4112479900871E-5));
#54427=CARTESIAN_POINT('Origin',(-11.2285451186048,0.,0.));
#54428=CARTESIAN_POINT('',(-6.82854511860477,-1.99779957878814,0.000555587305033103));
#54429=CARTESIAN_POINT('',(-6.67045488139523,-1.99238576655478,0.0012713935872409));
#54430=CARTESIAN_POINT('',(-11.2285451186048,-1.99475,-1.35786321299982E-13));
#54431=CARTESIAN_POINT('Ctrl Pts',(-6.82854511860477,-1.99779957878814,
0.000555587305033239));
#54432=CARTESIAN_POINT('Ctrl Pts',(-6.78825979533822,-1.99546732181797,
-0.627892405283668));
#54433=CARTESIAN_POINT('Ctrl Pts',(-6.7057270991384,-1.33741286327219,-1.91960565321309));
#54434=CARTESIAN_POINT('Ctrl Pts',(-6.58094703000533,0.860378736396868,
-2.19327080752055));
#54435=CARTESIAN_POINT('Ctrl Pts',(-6.45420491120554,2.30830739273333,-0.471598752640533));
#54436=CARTESIAN_POINT('Ctrl Pts',(-6.32746279240575,1.65171500523044,1.68003748284402));
#54437=CARTESIAN_POINT('Ctrl Pts',(-6.20072067360598,-0.510772566486323,
2.29995647536138));
#54438=CARTESIAN_POINT('Ctrl Pts',(-6.10108144900563,-1.84473032498764,
1.13881147582941));
#54439=CARTESIAN_POINT('Ctrl Pts',(-6.04368959733857,-1.99403503471576,
0.239218986321839));
#54440=CARTESIAN_POINT('Ctrl Pts',(-6.02854511860477,-1.99253871694387,
0.00135657260398022));
#54441=CARTESIAN_POINT('Ctrl Pts',(-6.67045488139523,-1.99238576655478,
0.00127139358724077));
#54442=CARTESIAN_POINT('Ctrl Pts',(-6.64383331345979,-1.98993258053751,
-0.416933185350539));
#54443=CARTESIAN_POINT('Ctrl Pts',(-6.5749643725911,-1.65726775971581,-1.50238294145243));
#54444=CARTESIAN_POINT('Ctrl Pts',(-6.46384805878913,0.122197131302195,
-2.35281863047693));
#54445=CARTESIAN_POINT('Ctrl Pts',(-6.33710593998936,2.04049135411991,-1.17774474322024));
#54446=CARTESIAN_POINT('Ctrl Pts',(-6.21036382118955,2.09843673094916,1.07109800325793));
#54447=CARTESIAN_POINT('Ctrl Pts',(-6.08362170238978,0.243203528140627,
2.34340344166606));
#54448=CARTESIAN_POINT('Ctrl Pts',(-5.97031872245832,-1.61353055607485,
1.57082731498654));
#54449=CARTESIAN_POINT('Ctrl Pts',(-5.89926311546014,-1.98972044842943,
0.450508844706632));
#54450=CARTESIAN_POINT('Ctrl Pts',(-5.87045488139522,-1.99315854296458,
-0.00160486565277954));
#54451=CARTESIAN_POINT('Origin',(-11.2285451186048,0.,0.));
#54452=CARTESIAN_POINT('',(-7.62854511860478,-1.99410870701803,-0.00178313212496593));
#54453=CARTESIAN_POINT('',(-7.47045488139523,-1.99770021155217,0.000684642813972708));
#54454=CARTESIAN_POINT('',(-11.2285451186048,-1.99475,-1.35786321299982E-13));
#54455=CARTESIAN_POINT('Ctrl Pts',(-7.62854511860478,-1.99410870701803,
-0.00178313212496591));
#54456=CARTESIAN_POINT('Ctrl Pts',(-7.61732473920439,-1.99565114909841,
-0.1776621488792));
#54457=CARTESIAN_POINT('Ctrl Pts',(-7.56385698687075,-1.89390590255069,
-1.01401214084348));
#54458=CARTESIAN_POINT('Ctrl Pts',(-7.46814186160383,-0.720940648501152,
-2.24297408351883));
#54459=CARTESIAN_POINT('Ctrl Pts',(-7.34139974280405,1.48954593240367,-1.82536062259485));
#54460=CARTESIAN_POINT('Ctrl Pts',(-7.21465762400426,2.34198950274749,0.256463625198942));
#54461=CARTESIAN_POINT('Ctrl Pts',(-7.08791550520447,1.05920349809169,2.10446580356721));
#54462=CARTESIAN_POINT('Ctrl Pts',(-6.96117338640469,-1.18927539801392,
2.03379262579923));
#54463=CARTESIAN_POINT('Ctrl Pts',(-6.87471659087145,-1.98342949352272,
0.720717239997897));
#54464=CARTESIAN_POINT('Ctrl Pts',(-6.83050716827148,-1.99791316864271,
0.031163413541011));
#54465=CARTESIAN_POINT('Ctrl Pts',(-6.82854511860477,-1.99779957878814,
0.000555587305033239));
#54466=CARTESIAN_POINT('Ctrl Pts',(-7.47045488139522,-1.99770021155217,
0.000684642813972708));
#54467=CARTESIAN_POINT('Ctrl Pts',(-7.4306508843927,-1.99492802125712,-0.620336927842107));
#54468=CARTESIAN_POINT('Ctrl Pts',(-7.34859951445692,-1.35063127267045,
-1.90546653095491));
#54469=CARTESIAN_POINT('Ctrl Pts',(-7.22430077158785,0.835450035231239,
-2.20288694657198));
#54470=CARTESIAN_POINT('Ctrl Pts',(-7.09755865278807,2.30281051449999,-0.497746302890819));
#54471=CARTESIAN_POINT('Ctrl Pts',(-6.97081653398828,1.67066154010014,1.66119765838736));
#54472=CARTESIAN_POINT('Ctrl Pts',(-6.84407441518849,-0.484656478440782,
2.30560095130741));
#54473=CARTESIAN_POINT('Ctrl Pts',(-6.74395386432414,-1.83820373823975,
1.15412307625533));
#54474=CARTESIAN_POINT('Ctrl Pts',(-6.68608068639306,-1.99382568949329,
0.246740902202544));
#54475=CARTESIAN_POINT('Ctrl Pts',(-6.67045488139523,-1.99238576655478,
0.00127139358724077));
#54476=CARTESIAN_POINT('Origin',(-11.2285451186048,0.,0.));
#54477=CARTESIAN_POINT('',(-8.42854511860477,-1.99182883653917,0.000811954458581844));
#54478=CARTESIAN_POINT('',(-8.27045488139523,-1.99432920278645,-0.00179785228075047));
#54479=CARTESIAN_POINT('',(-11.2285451186048,-1.99475,-1.35786321299982E-13));
#54480=CARTESIAN_POINT('Ctrl Pts',(-8.42854511860477,-1.99182883653917,
0.000811954458581864));
#54481=CARTESIAN_POINT('Ctrl Pts',(-8.4041423101373,-1.99042079763708,-0.382807210105715));
#54482=CARTESIAN_POINT('Ctrl Pts',(-8.33749212873656,-1.69891434362089,
-1.43254947889824));
#54483=CARTESIAN_POINT('Ctrl Pts',(-8.22859457440256,-0.000914680687675627,
-2.35598723428903));
#54484=CARTESIAN_POINT('Ctrl Pts',(-8.10185245560277,1.97616110191247,-1.28276191309921));
#54485=CARTESIAN_POINT('Ctrl Pts',(-7.97511033680299,2.15153978631802,0.959982702237039));
#54486=CARTESIAN_POINT('Ctrl Pts',(-7.8483682180032,0.36532454981711,2.32749321407739));
#54487=CARTESIAN_POINT('Ctrl Pts',(-7.73284647860379,-1.56634391446507,
1.63978732290449));
#54488=CARTESIAN_POINT('Ctrl Pts',(-7.65957211213766,-1.98984349113318,
0.484563801492637));
#54489=CARTESIAN_POINT('Ctrl Pts',(-7.62854511860478,-1.99410870701803,
-0.00178313212496591));
#54490=CARTESIAN_POINT('Ctrl Pts',(-8.27045488139523,-1.99432920278645,
-0.00179785228075055));
#54491=CARTESIAN_POINT('Ctrl Pts',(-8.25971582825887,-1.99583155638226,
-0.170084723045423));
#54492=CARTESIAN_POINT('Ctrl Pts',(-8.20672940218925,-1.89945569290877,
-0.99871553949203));
#54493=CARTESIAN_POINT('Ctrl Pts',(-8.11149560318635,-0.746331107676049,
-2.23465339663279));
#54494=CARTESIAN_POINT('Ctrl Pts',(-7.98475348438659,1.4687490430934,-1.84213581757841));
#54495=CARTESIAN_POINT('Ctrl Pts',(-7.85801136558678,2.344747252036,0.229887303677403));
#54496=CARTESIAN_POINT('Ctrl Pts',(-7.73126924678701,1.08300149158113,2.09231813301428));
#54497=CARTESIAN_POINT('Ctrl Pts',(-7.60452712798722,-1.16613411679633,
2.04714898162071));
#54498=CARTESIAN_POINT('Ctrl Pts',(-7.51758900618996,-1.97963221169911,
0.735904795036756));
#54499=CARTESIAN_POINT('Ctrl Pts',(-7.47289825732596,-1.99787038298098,
0.0388061701096327));
#54500=CARTESIAN_POINT('Ctrl Pts',(-7.47045488139522,-1.99770021155217,
0.000684642813972708));
#54501=CARTESIAN_POINT('Origin',(-11.2285451186048,0.,0.));
#54502=CARTESIAN_POINT('',(-9.22854511860477,-1.99701091303081,0.00134739702958219));
#54503=CARTESIAN_POINT('',(-9.07045488139523,-1.99173797669883,0.000711821429190546));
#54504=CARTESIAN_POINT('',(-11.2285451186048,-1.99475,-1.35786321299982E-13));
#54505=CARTESIAN_POINT('Ctrl Pts',(-9.22854511860477,-1.99701091303081,
0.00134739702958217));
#54506=CARTESIAN_POINT('Ctrl Pts',(-9.1909598810702,-1.99279767918952,-0.585541655733389));
#54507=CARTESIAN_POINT('Ctrl Pts',(-9.11112727060237,-1.40970256146536,
-1.83984346058858));
#54508=CARTESIAN_POINT('Ctrl Pts',(-8.98904728720129,0.719219398296349,
-2.24341372601176));
#54509=CARTESIAN_POINT('Ctrl Pts',(-8.86230516840148,2.27364387353221,-0.617461289050906));
#54510=CARTESIAN_POINT('Ctrl Pts',(-8.73556304960172,1.75519010714565,1.57166161499472));
#54511=CARTESIAN_POINT('Ctrl Pts',(-8.60882093080191,-0.363519475821205,
2.32775941317825));
#54512=CARTESIAN_POINT('Ctrl Pts',(-8.5064816204696,-1.80667193342064,1.22468927408845));
#54513=CARTESIAN_POINT('Ctrl Pts',(-8.44638968307056,-1.99285846560797,
0.28133363791573));
#54514=CARTESIAN_POINT('Ctrl Pts',(-8.42854511860477,-1.99182883653917,
0.000811954458581864));
#54515=CARTESIAN_POINT('Ctrl Pts',(-9.07045488139523,-1.99173797669883,
0.000711821429190372));
#54516=CARTESIAN_POINT('Ctrl Pts',(-9.04653339919178,-1.99055413223079,
-0.375387133202429));
#54517=CARTESIAN_POINT('Ctrl Pts',(-8.98036454405507,-1.70760085155004,
-1.41737766741566));
#54518=CARTESIAN_POINT('Ctrl Pts',(-8.87194831598508,-0.0276278227480409,
-2.3558111213894));
#54519=CARTESIAN_POINT('Ctrl Pts',(-8.74520619718531,1.96148356546545,-1.30509783891208));
#54520=CARTESIAN_POINT('Ctrl Pts',(-8.61846407838551,2.16228968585577,0.935524719754586));
#54521=CARTESIAN_POINT('Ctrl Pts',(-8.49172195958573,0.391695740945932,
2.32319829923402));
#54522=CARTESIAN_POINT('Ctrl Pts',(-8.37571889392229,-1.55572672538957,
1.65467216178432));
#54523=CARTESIAN_POINT('Ctrl Pts',(-8.30196320119213,-1.98992130602461,
0.491954853320625));
#54524=CARTESIAN_POINT('Ctrl Pts',(-8.27045488139523,-1.99432920278645,
-0.00179785228075055));
#54525=CARTESIAN_POINT('Ctrl Pts',(-10.0126273851832,-0.875140871775484,
1.79252782880714));
#54526=CARTESIAN_POINT('Ctrl Pts',(-9.97038001224991,-1.46991969395398,
1.50214725641666));
#54527=CARTESIAN_POINT('Ctrl Pts',(-9.88588526638337,-2.33763048368433,
0.288012276356903));
#54528=CARTESIAN_POINT('Ctrl Pts',(-9.75914314758361,-1.51210248954419,
-1.80872878115075));
#54529=CARTESIAN_POINT('Ctrl Pts',(-9.63240102878379,0.693993151391669,
-2.25074530311671));
#54530=CARTESIAN_POINT('Ctrl Pts',(-9.50565890998404,2.2663578788523,-0.643561605617013));
#54531=CARTESIAN_POINT('Ctrl Pts',(-9.37891679118423,1.77297281393676,1.55184140168292));
#54532=CARTESIAN_POINT('Ctrl Pts',(-9.25217467238445,-0.337135258971208,
2.331634562323));
#54533=CARTESIAN_POINT('Ctrl Pts',(-9.12543255358466,-2.13972744825445,
0.986043024971392));
#54534=CARTESIAN_POINT('Ctrl Pts',(-8.99869043478488,-1.99157127464006,
-1.25875170116619));
#54535=CARTESIAN_POINT('Ctrl Pts',(-8.87194831598508,-0.0276278227480409,
-2.3558111213894));
#54536=CARTESIAN_POINT('Ctrl Pts',(-8.74520619718531,1.96148356546545,-1.30509783891208));
#54537=CARTESIAN_POINT('Ctrl Pts',(-8.61846407838551,2.16228968585577,0.935524719754586));
#54538=CARTESIAN_POINT('Ctrl Pts',(-8.49172195958573,0.391695740945932,
2.32319829923402));
#54539=CARTESIAN_POINT('Ctrl Pts',(-8.36497984078594,-1.73601052414358,
1.59278295504605));
#54540=CARTESIAN_POINT('Ctrl Pts',(-8.23823772198616,-2.28096959425052,
-0.589802678095906));
#54541=CARTESIAN_POINT('Ctrl Pts',(-8.11149560318635,-0.746331107676049,
-2.23465339663279));
#54542=CARTESIAN_POINT('Ctrl Pts',(-7.98475348438659,1.4687490430934,-1.84213581757841));
#54543=CARTESIAN_POINT('Ctrl Pts',(-7.85801136558678,2.344747252036,0.229887303677403));
#54544=CARTESIAN_POINT('Ctrl Pts',(-7.73126924678701,1.08300149158113,2.09231813301428));
#54545=CARTESIAN_POINT('Ctrl Pts',(-7.60452712798722,-1.16613411679633,
2.04714898162071));
#54546=CARTESIAN_POINT('Ctrl Pts',(-7.47778500918743,-2.35208649368352,
0.135561026464403));
#54547=CARTESIAN_POINT('Ctrl Pts',(-7.35104289038765,-1.39360369803105,
-1.89962005280031));
#54548=CARTESIAN_POINT('Ctrl Pts',(-7.22430077158785,0.835450035231239,
-2.20288694657198));
#54549=CARTESIAN_POINT('Ctrl Pts',(-7.09755865278807,2.30281051449999,-0.497746302890819));
#54550=CARTESIAN_POINT('Ctrl Pts',(-6.97081653398828,1.67066154010014,1.66119765838736));
#54551=CARTESIAN_POINT('Ctrl Pts',(-6.84407441518849,-0.484656478440782,
2.30560095130741));
#54552=CARTESIAN_POINT('Ctrl Pts',(-6.71733229638871,-2.19810537700899,
0.847950704926883));
#54553=CARTESIAN_POINT('Ctrl Pts',(-6.59059017758893,-1.90750618498507,
-1.38278986114584));
#54554=CARTESIAN_POINT('Ctrl Pts',(-6.46384805878913,0.122197131302195,
-2.35281863047693));
#54555=CARTESIAN_POINT('Ctrl Pts',(-6.33710593998936,2.04049135411991,-1.17774474322024));
#54556=CARTESIAN_POINT('Ctrl Pts',(-6.21036382118955,2.09843673094916,1.07109800325793));
#54557=CARTESIAN_POINT('Ctrl Pts',(-6.08362170238978,0.243203528140627,
2.34340344166606));
#54558=CARTESIAN_POINT('Ctrl Pts',(-5.95687958358998,-1.83376225002018,
1.47919020306685));
#54559=CARTESIAN_POINT('Ctrl Pts',(-5.8301374647902,-2.23885743746508,-0.733624577802266));
#54560=CARTESIAN_POINT('Ctrl Pts',(-5.70339534599041,-0.60275022452326,
-2.27758201022554));
#54561=CARTESIAN_POINT('Ctrl Pts',(-5.57665322719063,1.58289408021768,-1.74503122529871));
#54562=CARTESIAN_POINT('Ctrl Pts',(-5.44991110839084,2.32538834689053,0.378492645374279));
#54563=CARTESIAN_POINT('Ctrl Pts',(-5.32316898959105,0.947788588779759,
2.15693867261862));
#54564=CARTESIAN_POINT('Ctrl Pts',(-5.19642687079127,-1.29392529741552,
1.96886895733705));
#54565=CARTESIAN_POINT('Ctrl Pts',(-5.06968475199147,-2.35594664097114,
-0.0142503106843528));
#54566=CARTESIAN_POINT('Ctrl Pts',(-4.9429426331917,-1.27001347064424,-1.98437734084019));
#54567=CARTESIAN_POINT('Ctrl Pts',(-4.8162005143919,0.973811444563989,-2.14531557512957));
#54568=CARTESIAN_POINT('Ctrl Pts',(-4.68945839559212,2.3297967747643,-0.350335032157474));
#54569=CARTESIAN_POINT('Ctrl Pts',(-4.56271627679233,1.5616688454542,1.76405160457239));
#54570=CARTESIAN_POINT('Ctrl Pts',(-4.43597415799255,-0.630257733385777,
2.270123969294));
#54571=CARTESIAN_POINT('Ctrl Pts',(-4.30923203919275,-2.247568181374,0.706487732760443));
#54572=CARTESIAN_POINT('Ctrl Pts',(-4.18248992039297,-1.81573450338795,
-1.50126475335125));
#54573=CARTESIAN_POINT('Ctrl Pts',(-4.05574780159318,0.271533578210096,
-2.34028997398879));
#54574=CARTESIAN_POINT('Ctrl Pts',(-3.9290056827934,2.11124012136177,-1.04563511631196));
#54575=CARTESIAN_POINT('Ctrl Pts',(-3.80226356399361,2.02609502746784,1.20234212520804));
#54576=CARTESIAN_POINT('Ctrl Pts',(-3.67552144519382,0.0937264506913446,
2.35412467784988));
#54577=CARTESIAN_POINT('Ctrl Pts',(-3.54877932639404,-1.92409404154149,
1.35961382977754));
#54578=CARTESIAN_POINT('Ctrl Pts',(-3.42203720759425,-2.18768699293762,
-0.874478854390196));
#54579=CARTESIAN_POINT('Ctrl Pts',(-3.29529508879446,-0.456730463269167,
-2.31129507643307));
#54580=CARTESIAN_POINT('Ctrl Pts',(-3.16855296999467,1.69063459008238,-1.64086633568406));
#54581=CARTESIAN_POINT('Ctrl Pts',(-3.04181085119489,2.29662084453102,0.525566682988035));
#54582=CARTESIAN_POINT('Ctrl Pts',(-2.9150687323951,0.808740873387587,2.21283208749455));
#54583=CARTESIAN_POINT('Ctrl Pts',(-2.78832661359532,-1.41648119041691,
1.88262282413132));
#54584=CARTESIAN_POINT('Ctrl Pts',(-2.66158449479552,-2.35027451551463,
-0.164004005711231));
#54585=CARTESIAN_POINT('Ctrl Pts',(-2.53484237599575,-1.14128472098778,
-2.06110573511026));
#54586=CARTESIAN_POINT('Ctrl Pts',(-2.40810025719595,1.1082327929001,-2.07906416640946));
#54587=CARTESIAN_POINT('Ctrl Pts',(-2.28135813839617,2.34735651770835,-0.201506276029945));
#54588=CARTESIAN_POINT('Ctrl Pts',(-2.15461601959638,1.44635766333907,1.8597680925381));
#54589=CARTESIAN_POINT('Ctrl Pts',(-2.02787390079659,-0.773309122834207,
2.22546200204237));
#54590=CARTESIAN_POINT('Ctrl Pts',(-1.9011317819968,-2.28793686344939,0.562166198056052));
#54591=CARTESIAN_POINT('Ctrl Pts',(-1.77438966319702,-1.71661695495533,
-1.61366530573858));
#54592=CARTESIAN_POINT('Ctrl Pts',(-1.64764754439723,0.419772684089712,
-2.31829268547235));
#54593=CARTESIAN_POINT('Ctrl Pts',(-1.52090542559744,2.17344423984237,-0.909294246839299));
#54594=CARTESIAN_POINT('Ctrl Pts',(-1.39416330679766,1.94556036418415,1.3287204582401));
#54595=CARTESIAN_POINT('Ctrl Pts',(-1.26742118799787,-0.0561388408262527,
2.35532303034526));
#54596=CARTESIAN_POINT('Ctrl Pts',(-1.14067906919808,-2.00662370949219,
1.23453255313725));
#54597=CARTESIAN_POINT('Ctrl Pts',(-1.0139369503983,-2.12769776910723,-1.01178762124091));
#54598=CARTESIAN_POINT('Ctrl Pts',(-0.887194831598507,-0.308800379382655,
-2.3356705087836));
#54599=CARTESIAN_POINT('Ctrl Pts',(-0.760452712798722,1.7914157663844,-1.5300357731145));
#54600=CARTESIAN_POINT('Ctrl Pts',(-0.633710593998933,2.25878798203272,
0.670463412246034));
#54601=CARTESIAN_POINT('Ctrl Pts',(-0.506968475199148,0.665987972658192,
2.25986937576817));
#54602=CARTESIAN_POINT('Ctrl Pts',(-0.380226356399362,-1.53247742911832,
1.7885731304376));
#54603=CARTESIAN_POINT('Ctrl Pts',(-0.253484237599572,-2.33669743267895,
-0.312728077985436));
#54604=CARTESIAN_POINT('Ctrl Pts',(-0.126742118799788,-1.00466619559831,
-2.13028476617671));
#54605=CARTESIAN_POINT('Ctrl Pts',(-0.04224737293326,0.485218894542327,
-2.04491391286112));
#54606=CARTESIAN_POINT('Ctrl Pts',(2.22044604925031E-15,1.04832369103677,
-1.69706953343434));
#54607=CARTESIAN_POINT('Ctrl Pts',(-9.92491825678878,-0.941790067967425,
1.92904360906012));
#54608=CARTESIAN_POINT('Ctrl Pts',(-9.88267088385552,-1.58186620362845,
1.61654816080935));
#54609=CARTESIAN_POINT('Ctrl Pts',(-9.79817613798899,-2.51566032751424,
0.3099467869388));
#54610=CARTESIAN_POINT('Ctrl Pts',(-9.67143401918922,-1.62726156705764,
-1.94647839756206));
#54611=CARTESIAN_POINT('Ctrl Pts',(-9.54469190038941,0.746846454436609,
-2.42215812375346));
#54612=CARTESIAN_POINT('Ctrl Pts',(-9.41794978158964,2.43895972591532,-0.692574130454715));
#54613=CARTESIAN_POINT('Ctrl Pts',(-9.29120766278984,1.9079993185032,1.67002692515151));
#54614=CARTESIAN_POINT('Ctrl Pts',(-9.16446554399007,-0.362810889881688,
2.50920776728247));
#54615=CARTESIAN_POINT('Ctrl Pts',(-9.03772342519026,-2.30268534348643,
1.06113833493183));
#54616=CARTESIAN_POINT('Ctrl Pts',(-8.91098130639049,-2.14324585515011,
-1.35461602632079));
#54617=CARTESIAN_POINT('Ctrl Pts',(-8.78423918759069,-0.0297319093449403,
-2.53522557074784));
#54618=CARTESIAN_POINT('Ctrl Pts',(-8.65749706879091,2.11086671873626,-1.40449180475312));
#54619=CARTESIAN_POINT('Ctrl Pts',(-8.53075494999112,2.32696588159104,1.00677264406057));
#54620=CARTESIAN_POINT('Ctrl Pts',(-8.40401283119134,0.421526602613842,
2.50012901317076));
#54621=CARTESIAN_POINT('Ctrl Pts',(-8.27727071239154,-1.86822204545008,
1.71408651551934));
#54622=CARTESIAN_POINT('Ctrl Pts',(-8.15052859359177,-2.45468424396932,
-0.634721017159638));
#54623=CARTESIAN_POINT('Ctrl Pts',(-8.02378647479197,-0.803170377814069,
-2.40484068585289));
#54624=CARTESIAN_POINT('Ctrl Pts',(-7.89704435599219,1.58060639804846,-1.98242965537954));
#54625=CARTESIAN_POINT('Ctrl Pts',(-7.7703022371924,2.52331909648023,0.247395118132163));
#54626=CARTESIAN_POINT('Ctrl Pts',(-7.64356011839261,1.16548098855872,2.25166541782378));
#54627=CARTESIAN_POINT('Ctrl Pts',(-7.51681799959282,-1.25494484892315,
2.20305626296317));
#54628=CARTESIAN_POINT('Ctrl Pts',(-7.39007588079304,-2.53121728191868,
0.145885116836835));
#54629=CARTESIAN_POINT('Ctrl Pts',(-7.26333376199326,-1.49973811510549,
-2.04429178928587));
#54630=CARTESIAN_POINT('Ctrl Pts',(-7.13659164319346,0.899076446821093,
-2.37065495858689));
#54631=CARTESIAN_POINT('Ctrl Pts',(-7.00984952439368,2.47818853045577,-0.535653789633947));
#54632=CARTESIAN_POINT('Ctrl Pts',(-6.8831074055939,1.79789619722521,1.78771156285491));
#54633=CARTESIAN_POINT('Ctrl Pts',(-6.75636528679411,-0.521567067077507,
2.48119148204365));
#54634=CARTESIAN_POINT('Ctrl Pts',(-6.62962316799431,-2.36550923305976,
0.912529145628809));
#54635=CARTESIAN_POINT('Ctrl Pts',(-6.50288104919454,-2.05277851548714,
-1.48810071534096));
#54636=CARTESIAN_POINT('Ctrl Pts',(-6.37613893039474,0.131503450822755,
-2.53200517696812));
#54637=CARTESIAN_POINT('Ctrl Pts',(-6.24939681159496,2.19589160221116,-1.26743972032225));
#54638=CARTESIAN_POINT('Ctrl Pts',(-6.12265469279517,2.25824999746211,1.15267095141095));
#54639=CARTESIAN_POINT('Ctrl Pts',(-5.99591257399539,0.26172548293031,2.52187294386588));
#54640=CARTESIAN_POINT('Ctrl Pts',(-5.86917045519559,-1.97341837158038,
1.59184273848027));
#54641=CARTESIAN_POINT('Ctrl Pts',(-5.74242833639581,-2.40936489907259,
-0.789496140877558));
#54642=CARTESIAN_POINT('Ctrl Pts',(-5.61568621759603,-0.648654626048355,
-2.45103866747753));
#54643=CARTESIAN_POINT('Ctrl Pts',(-5.48894409879623,1.70344452130206,-1.87792974740757));
#54644=CARTESIAN_POINT('Ctrl Pts',(-5.36220197999645,2.50248585102143,0.407317982405529));
#54645=CARTESIAN_POINT('Ctrl Pts',(-5.23545986119667,1.01997050787345,2.32120734455678));
#54646=CARTESIAN_POINT('Ctrl Pts',(-5.10871774239687,-1.39246838206223,
2.11881456911904));
#54647=CARTESIAN_POINT('Ctrl Pts',(-4.98197562359709,-2.53537141126359,
-0.0153355893900096));
#54648=CARTESIAN_POINT('Ctrl Pts',(-4.8552335047973,-1.36673547243999,-2.1355040439505));
#54649=CARTESIAN_POINT('Ctrl Pts',(-4.72849138599752,1.04797521878131,-2.30869905231807));
#54650=CARTESIAN_POINT('Ctrl Pts',(-4.60174926719773,2.50723001704174,-0.377015934677563));
#54651=CARTESIAN_POINT('Ctrl Pts',(-4.47500714839794,1.68060280982999,1.89839868545702));
#54652=CARTESIAN_POINT('Ctrl Pts',(-4.34826502959816,-0.678257058612913,
2.44301263520966));
#54653=CARTESIAN_POINT('Ctrl Pts',(-4.22152291079836,-2.4187390379828,0.760292601241146));
#54654=CARTESIAN_POINT('Ctrl Pts',(-4.09478079199859,-1.954017663336,-1.61559844785595));
#54655=CARTESIAN_POINT('Ctrl Pts',(-3.96803867319879,0.292213099999658,
-2.51852235994282));
#54656=CARTESIAN_POINT('Ctrl Pts',(-3.84129655439901,2.27202847166641,-1.12526885558744));
#54657=CARTESIAN_POINT('Ctrl Pts',(-3.71455443559922,2.18039887653306,1.29391039584572));
#54658=CARTESIAN_POINT('Ctrl Pts',(-3.58781231679943,0.100864493036274,
2.53341069062175));
#54659=CARTESIAN_POINT('Ctrl Pts',(-3.46107019799964,-2.07062967414917,
1.46315963801102));
#54660=CARTESIAN_POINT('Ctrl Pts',(-3.33432807919986,-2.35429740310286,
-0.94107763249744));
#54661=CARTESIAN_POINT('Ctrl Pts',(-3.20758596040007,-0.491514255496263,
-2.48731926176697));
#54662=CARTESIAN_POINT('Ctrl Pts',(-3.08084384160029,1.819390359716,-1.76583184222006));
#54663=CARTESIAN_POINT('Ctrl Pts',(-2.9541017228005,2.47152746606171,0.56559292115852));
#54664=CARTESIAN_POINT('Ctrl Pts',(-2.82735960400071,0.870333161986235,
2.38135750402555));
#54665=CARTESIAN_POINT('Ctrl Pts',(-2.70061748520092,-1.52435791724691,
2.0260000814481));
#54666=CARTESIAN_POINT('Ctrl Pts',(-2.57387536640113,-2.5292673066657,-0.17649426357192));
#54667=CARTESIAN_POINT('Ctrl Pts',(-2.44713324760135,-1.22820296664768,
-2.21807593835652));
#54668=CARTESIAN_POINT('Ctrl Pts',(-2.32039112880156,1.19263386159946,-2.23740205233354));
#54669=CARTESIAN_POINT('Ctrl Pts',(-2.19364901000178,2.52612707925668,-0.216852641121762));
#54670=CARTESIAN_POINT('Ctrl Pts',(-2.06690689120199,1.55650973002526,2.00140477352138));
#54671=CARTESIAN_POINT('Ctrl Pts',(-1.9401647724022,-0.832202991361024,
2.39494929074703));
#54672=CARTESIAN_POINT('Ctrl Pts',(-1.81342265360242,-2.46218212818884,
0.604979791198736));
#54673=CARTESIAN_POINT('Ctrl Pts',(-1.68668053480263,-1.84735149599571,
-1.73655922947009));
#54674=CARTESIAN_POINT('Ctrl Pts',(-1.55993841600284,0.451741836577292,
-2.49484979645603));
#54675=CARTESIAN_POINT('Ctrl Pts',(-1.43319629720305,2.33896994687469,-0.978544504264554));
#54676=CARTESIAN_POINT('Ctrl Pts',(-1.30645417840327,2.09373083433111,1.4299134813997));
#54677=CARTESIAN_POINT('Ctrl Pts',(-1.17971205960348,-0.0604142766296505,
2.53470030754455));
#54678=CARTESIAN_POINT('Ctrl Pts',(-1.05296994080369,-2.15944465707978,
1.32855239039211));
#54679=CARTESIAN_POINT('Ctrl Pts',(-0.926227822003907,-2.2897395050425,
-1.08884359456764));
#54680=CARTESIAN_POINT('Ctrl Pts',(-0.799485703204116,-0.332318075485546,
-2.5135510843575));
#54681=CARTESIAN_POINT('Ctrl Pts',(-0.672743584404332,1.92784685391077,
-1.64656061809875));
#54682=CARTESIAN_POINT('Ctrl Pts',(-0.546001465604543,2.43081331901086,
0.721524731564423));
#54683=CARTESIAN_POINT('Ctrl Pts',(-0.419259346804758,0.716708450335271,
2.43197706979939));
#54684=CARTESIAN_POINT('Ctrl Pts',(-0.292517228004972,-1.64918822634783,
1.92478772778847));
#54685=CARTESIAN_POINT('Ctrl Pts',(-0.165775109205182,-2.51465621697831,
-0.336544900735453));
#54686=CARTESIAN_POINT('Ctrl Pts',(-0.0390329904053974,-1.08117981361961,
-2.29252352327827));
#54687=CARTESIAN_POINT('Ctrl Pts',(0.0454617554611303,0.522172315804407,
-2.20065097528105));
#54688=CARTESIAN_POINT('Ctrl Pts',(0.0877091283943924,1.12816218745486,
-1.82631537708437));
#54689=CARTESIAN_POINT('Ctrl Pts',(-9.83720912839439,-1.00843926415937,
2.0655593893131));
#54690=CARTESIAN_POINT('Ctrl Pts',(-9.79496175546113,-1.69381271330293,
1.73094906520204));
#54691=CARTESIAN_POINT('Ctrl Pts',(-9.7104670095946,-2.69369017134415,0.3318812975207));
#54692=CARTESIAN_POINT('Ctrl Pts',(-9.58372489079482,-1.74242064457108,
-2.08422801397338));
#54693=CARTESIAN_POINT('Ctrl Pts',(-9.45698277199502,0.799699757481549,
-2.5935709443902));
#54694=CARTESIAN_POINT('Ctrl Pts',(-9.33024065319525,2.61156157297835,-0.741586655292419));
#54695=CARTESIAN_POINT('Ctrl Pts',(-9.20349853439545,2.04302582306964,1.78821244862011));
#54696=CARTESIAN_POINT('Ctrl Pts',(-9.07675641559567,-0.38848652079217,
2.68678097224194));
#54697=CARTESIAN_POINT('Ctrl Pts',(-8.95001429679588,-2.4656432387184,1.13623364489228));
#54698=CARTESIAN_POINT('Ctrl Pts',(-8.8232721779961,-2.29492043566016,-1.45048035147539));
#54699=CARTESIAN_POINT('Ctrl Pts',(-8.6965300591963,-0.0318359959418395,
-2.71464002010627));
#54700=CARTESIAN_POINT('Ctrl Pts',(-8.56978794039653,2.26024987200707,-1.50388577059416));
#54701=CARTESIAN_POINT('Ctrl Pts',(-8.44304582159672,2.49164207732631,1.07802056836655));
#54702=CARTESIAN_POINT('Ctrl Pts',(-8.31630370279695,0.451357464281749,
2.67705972710749));
#54703=CARTESIAN_POINT('Ctrl Pts',(-8.18956158399716,-2.00043356675657,
1.83539007599263));
#54704=CARTESIAN_POINT('Ctrl Pts',(-8.06281946519737,-2.62839889368811,
-0.679639356223372));
#54705=CARTESIAN_POINT('Ctrl Pts',(-7.93607734639759,-0.860009647952086,
-2.57502797507298));
#54706=CARTESIAN_POINT('Ctrl Pts',(-7.80933522759779,1.69246375300351,-2.12272349318067));
#54707=CARTESIAN_POINT('Ctrl Pts',(-7.68259310879802,2.70189094092447,0.264902932586925));
#54708=CARTESIAN_POINT('Ctrl Pts',(-7.55585098999822,1.24796048553631,2.41101270263327));
#54709=CARTESIAN_POINT('Ctrl Pts',(-7.42910887119844,-1.34375558104996,
2.35896354430564));
#54710=CARTESIAN_POINT('Ctrl Pts',(-7.30236675239865,-2.71034807015384,
0.156209207209267));
#54711=CARTESIAN_POINT('Ctrl Pts',(-7.17562463359886,-1.60587253217993,
-2.18896352577142));
#54712=CARTESIAN_POINT('Ctrl Pts',(-7.04888251479907,0.962702858410947,
-2.53842297060179));
#54713=CARTESIAN_POINT('Ctrl Pts',(-6.92214039599929,2.65356654641154,-0.573561276377074));
#54714=CARTESIAN_POINT('Ctrl Pts',(-6.79539827719949,1.92513085435028,1.91422546732247));
#54715=CARTESIAN_POINT('Ctrl Pts',(-6.66865615839972,-0.558477655714234,
2.65678201277989));
#54716=CARTESIAN_POINT('Ctrl Pts',(-6.54191403959993,-2.53291308911053,
0.977107586330735));
#54717=CARTESIAN_POINT('Ctrl Pts',(-6.41517192080014,-2.1980508459892,-1.59341156953609));
#54718=CARTESIAN_POINT('Ctrl Pts',(-6.28842980200036,0.140809770343312,
-2.7111917234593));
#54719=CARTESIAN_POINT('Ctrl Pts',(-6.16168768320056,2.35129185030242,-1.35713469742426));
#54720=CARTESIAN_POINT('Ctrl Pts',(-6.03494556440078,2.41806326397505,1.23424389956398));
#54721=CARTESIAN_POINT('Ctrl Pts',(-5.90820344560099,0.280247437719996,
2.70034244606571));
#54722=CARTESIAN_POINT('Ctrl Pts',(-5.78146132680121,-2.11307449314059,
1.7044952738937));
#54723=CARTESIAN_POINT('Ctrl Pts',(-5.65471920800142,-2.5798723606801,-0.845367703952849));
#54724=CARTESIAN_POINT('Ctrl Pts',(-5.52797708920163,-0.694559027573452,
-2.62449532472953));
#54725=CARTESIAN_POINT('Ctrl Pts',(-5.40123497040184,1.82399496238643,-2.01082826951643));
#54726=CARTESIAN_POINT('Ctrl Pts',(-5.27449285160206,2.67958335515234,0.436143319436778));
#54727=CARTESIAN_POINT('Ctrl Pts',(-5.14775073280227,1.09215242696715,2.48547601649493));
#54728=CARTESIAN_POINT('Ctrl Pts',(-5.02100861400249,-1.49101146670894,
2.26876018090104));
#54729=CARTESIAN_POINT('Ctrl Pts',(-4.8942664952027,-2.71479618155604,-0.0164208680956645));
#54730=CARTESIAN_POINT('Ctrl Pts',(-4.76752437640291,-1.46345747423573,
-2.28663074706081));
#54731=CARTESIAN_POINT('Ctrl Pts',(-4.64078225760312,1.12213899299862,-2.47208252950658));
#54732=CARTESIAN_POINT('Ctrl Pts',(-4.51404013880334,2.68466325931919,-0.403696837197651));
#54733=CARTESIAN_POINT('Ctrl Pts',(-4.38729802000355,1.79953677420578,2.03274576634164));
#54734=CARTESIAN_POINT('Ctrl Pts',(-4.26055590120376,-0.726256383840051,
2.61590130112531));
#54735=CARTESIAN_POINT('Ctrl Pts',(-4.13381378240398,-2.58990989459159,
0.814097469721848));
#54736=CARTESIAN_POINT('Ctrl Pts',(-4.00707166360419,-2.09230082328405,
-1.72993214236066));
#54737=CARTESIAN_POINT('Ctrl Pts',(-3.8803295448044,0.312892621789216,-2.69675474589685));
#54738=CARTESIAN_POINT('Ctrl Pts',(-3.75358742600461,2.43281682197106,-1.20490259486291));
#54739=CARTESIAN_POINT('Ctrl Pts',(-3.62684530720483,2.33470272559827,1.38547866648339));
#54740=CARTESIAN_POINT('Ctrl Pts',(-3.50010318840504,0.108002535381206,
2.71269670339363));
#54741=CARTESIAN_POINT('Ctrl Pts',(-3.37336106960526,-2.21716530675685,
1.56670544624449));
#54742=CARTESIAN_POINT('Ctrl Pts',(-3.24661895080546,-2.52090781326811,
-1.00767641060468));
#54743=CARTESIAN_POINT('Ctrl Pts',(-3.11987683200569,-0.526298047723356,
-2.66334344710087));
#54744=CARTESIAN_POINT('Ctrl Pts',(-2.99313471320588,1.94814612934961,-1.89079734875606));
#54745=CARTESIAN_POINT('Ctrl Pts',(-2.86639259440611,2.6464340875924,0.605619159329004));
#54746=CARTESIAN_POINT('Ctrl Pts',(-2.73965047560631,0.931925450584883,
2.54988292055654));
#54747=CARTESIAN_POINT('Ctrl Pts',(-2.61290835680654,-1.63223464407691,
2.16937733876486));
#54748=CARTESIAN_POINT('Ctrl Pts',(-2.48616623800674,-2.70826009781677,
-0.188984521432605));
#54749=CARTESIAN_POINT('Ctrl Pts',(-2.35942411920696,-1.31512121230757,
-2.37504614160279));
#54750=CARTESIAN_POINT('Ctrl Pts',(-2.23268200040717,1.27703493029882,-2.39573993825761));
#54751=CARTESIAN_POINT('Ctrl Pts',(-2.10593988160739,2.704897640805,-0.232199006213583));
#54752=CARTESIAN_POINT('Ctrl Pts',(-1.97919776280759,1.66666179671145,2.14304145450466));
#54753=CARTESIAN_POINT('Ctrl Pts',(-1.85245564400781,-0.891096859887847,
2.56443657945168));
#54754=CARTESIAN_POINT('Ctrl Pts',(-1.72571352520802,-2.63642739292829,
0.647793384341421));
#54755=CARTESIAN_POINT('Ctrl Pts',(-1.59897140640824,-1.97808603703611,
-1.8594531532016));
#54756=CARTESIAN_POINT('Ctrl Pts',(-1.47222928760845,0.48371098906488,-2.6714069074397));
#54757=CARTESIAN_POINT('Ctrl Pts',(-1.34548716880866,2.504495653907,-1.04779476168981));
#54758=CARTESIAN_POINT('Ctrl Pts',(-1.21874505000888,2.24190130447808,1.53110650455931));
#54759=CARTESIAN_POINT('Ctrl Pts',(-1.09200293120909,-0.0646897124330518,
2.71407758474384));
#54760=CARTESIAN_POINT('Ctrl Pts',(-0.965260812409299,-2.31226560466736,
1.42257222764696));
#54761=CARTESIAN_POINT('Ctrl Pts',(-0.838518693609519,-2.45178124097777,
-1.16589956789437));
#54762=CARTESIAN_POINT('Ctrl Pts',(-0.711776574809725,-0.355835771588435,
-2.6914316599314));
#54763=CARTESIAN_POINT('Ctrl Pts',(-0.585034456009942,2.06427794143713,
-1.763085463083));
#54764=CARTESIAN_POINT('Ctrl Pts',(-0.458292337210153,2.602838655989,0.77258605088281));
#54765=CARTESIAN_POINT('Ctrl Pts',(-0.331550218410368,0.767428928012345,
2.60408476383061));
#54766=CARTESIAN_POINT('Ctrl Pts',(-0.204808099610581,-1.76589902357732,
2.06100232513935));
#54767=CARTESIAN_POINT('Ctrl Pts',(-0.0780659808107919,-2.69261500127767,
-0.360361723485471));
#54768=CARTESIAN_POINT('Ctrl Pts',(0.048676137988993,-1.15769343164092,
-2.45476228037983));
#54769=CARTESIAN_POINT('Ctrl Pts',(0.13317088385552,0.559125737066487,-2.35638803770098));
#54770=CARTESIAN_POINT('Ctrl Pts',(0.175418256788783,1.20800068387295,-1.95556122073441));
#54771=CARTESIAN_POINT('Ctrl Pts',(-9.7495,-1.07508846035131,2.20207516956608));
#54772=CARTESIAN_POINT('Ctrl Pts',(-9.70725262706674,-1.80575922297741,
1.84534996959472));
#54773=CARTESIAN_POINT('Ctrl Pts',(-9.62275788120021,-2.87172001517406,
0.353815808102598));
#54774=CARTESIAN_POINT('Ctrl Pts',(-9.49601576240043,-1.85757972208452,
-2.22197763038469));
#54775=CARTESIAN_POINT('Ctrl Pts',(-9.36927364360064,0.852553060526489,
-2.76498376502695));
#54776=CARTESIAN_POINT('Ctrl Pts',(-9.24253152480086,2.78416342004137,-0.790599180130123));
#54777=CARTESIAN_POINT('Ctrl Pts',(-9.11578940600106,2.17805232763608,1.9063979720887));
#54778=CARTESIAN_POINT('Ctrl Pts',(-8.98904728720128,-0.414162151702653,
2.86435417720141));
#54779=CARTESIAN_POINT('Ctrl Pts',(-8.86230516840148,-2.62860113395038,
1.21132895485272));
#54780=CARTESIAN_POINT('Ctrl Pts',(-8.73556304960171,-2.44659501617021,
-1.54634467663));
#54781=CARTESIAN_POINT('Ctrl Pts',(-8.6088209308019,-0.0339400825387369,
-2.89405446946471));
#54782=CARTESIAN_POINT('Ctrl Pts',(-8.48207881200215,2.40963302527788,-1.60327973643519));
#54783=CARTESIAN_POINT('Ctrl Pts',(-8.35533669320233,2.65631827306158,1.14926849267254));
#54784=CARTESIAN_POINT('Ctrl Pts',(-8.22859457440257,0.481188325949657,
2.85399044104422));
#54785=CARTESIAN_POINT('Ctrl Pts',(-8.10185245560276,-2.13264508806306,
1.95669363646592));
#54786=CARTESIAN_POINT('Ctrl Pts',(-7.97511033680299,-2.80211354340691,
-0.724557695287102));
#54787=CARTESIAN_POINT('Ctrl Pts',(-7.8483682180032,-0.9168489180901,-2.74521526429308));
#54788=CARTESIAN_POINT('Ctrl Pts',(-7.7216260992034,1.80432110795856,-2.2630173309818));
#54789=CARTESIAN_POINT('Ctrl Pts',(-7.59488398040362,2.8804627853687,0.282410747041685));
#54790=CARTESIAN_POINT('Ctrl Pts',(-7.46814186160384,1.33043998251391,2.57035998744277));
#54791=CARTESIAN_POINT('Ctrl Pts',(-7.34139974280405,-1.43256631317677,
2.51487082564811));
#54792=CARTESIAN_POINT('Ctrl Pts',(-7.21465762400426,-2.889478858389,0.166533297581697));
#54793=CARTESIAN_POINT('Ctrl Pts',(-7.08791550520448,-1.71200694925436,
-2.33363526225698));
#54794=CARTESIAN_POINT('Ctrl Pts',(-6.96117338640468,1.02632927000079,-2.7061909826167));
#54795=CARTESIAN_POINT('Ctrl Pts',(-6.8344312676049,2.82894456236732,-0.611468763120201));
#54796=CARTESIAN_POINT('Ctrl Pts',(-6.70768914880512,2.05236551147535,2.04073937179003));
#54797=CARTESIAN_POINT('Ctrl Pts',(-6.58094703000532,-0.595388244350957,
2.83237254351614));
#54798=CARTESIAN_POINT('Ctrl Pts',(-6.45420491120554,-2.7003169451613,1.04168602703266));
#54799=CARTESIAN_POINT('Ctrl Pts',(-6.32746279240576,-2.34332317649127,
-1.69872242373121));
#54800=CARTESIAN_POINT('Ctrl Pts',(-6.20072067360596,0.150116089863871,
-2.89037826995048));
#54801=CARTESIAN_POINT('Ctrl Pts',(-6.07397855480618,2.50669209839368,-1.44682967452627));
#54802=CARTESIAN_POINT('Ctrl Pts',(-5.94723643600639,2.577876530488,1.315816847717));
#54803=CARTESIAN_POINT('Ctrl Pts',(-5.8204943172066,0.298769392509677,2.87881194826553));
#54804=CARTESIAN_POINT('Ctrl Pts',(-5.69375219840682,-2.25273061470079,
1.81714780930712));
#54805=CARTESIAN_POINT('Ctrl Pts',(-5.56701007960703,-2.75037982228761,
-0.901239267028141));
#54806=CARTESIAN_POINT('Ctrl Pts',(-5.44026796080724,-0.740463429098543,
-2.79795198198153));
#54807=CARTESIAN_POINT('Ctrl Pts',(-5.31352584200746,1.9445454034708,-2.14372679162529));
#54808=CARTESIAN_POINT('Ctrl Pts',(-5.18678372320766,2.85668085928325,0.464968656468029));
#54809=CARTESIAN_POINT('Ctrl Pts',(-5.06004160440788,1.16433434606084,2.64974468843308));
#54810=CARTESIAN_POINT('Ctrl Pts',(-4.9332994856081,-1.58955455135565,2.41870579268303));
#54811=CARTESIAN_POINT('Ctrl Pts',(-4.8065573668083,-2.89422095184849,-0.0175061468013224));
#54812=CARTESIAN_POINT('Ctrl Pts',(-4.67981524800852,-1.56017947603147,
-2.43775745017111));
#54813=CARTESIAN_POINT('Ctrl Pts',(-4.55307312920873,1.19630276721594,-2.63546600669509));
#54814=CARTESIAN_POINT('Ctrl Pts',(-4.42633101040895,2.86209650159664,-0.430377739717738));
#54815=CARTESIAN_POINT('Ctrl Pts',(-4.29958889160916,1.91847073858157,2.16709284722627));
#54816=CARTESIAN_POINT('Ctrl Pts',(-4.17284677280938,-0.774255709067188,
2.78878996704097));
#54817=CARTESIAN_POINT('Ctrl Pts',(-4.04610465400958,-2.76108075120038,
0.86790233820255));
#54818=CARTESIAN_POINT('Ctrl Pts',(-3.9193625352098,-2.2305839832321,-1.84426583686536));
#54819=CARTESIAN_POINT('Ctrl Pts',(-3.79262041641001,0.333572143578779,
-2.87498713185087));
#54820=CARTESIAN_POINT('Ctrl Pts',(-3.66587829761023,2.59360517227571,-1.28453633413838));
#54821=CARTESIAN_POINT('Ctrl Pts',(-3.53913617881044,2.48900657466348,1.47704693712107));
#54822=CARTESIAN_POINT('Ctrl Pts',(-3.41239406001065,0.115140577726135,
2.8919827161655));
#54823=CARTESIAN_POINT('Ctrl Pts',(-3.28565194121086,-2.36370093936452,
1.67025125447797));
#54824=CARTESIAN_POINT('Ctrl Pts',(-3.15890982241108,-2.68751822343335,
-1.07427518871192));
#54825=CARTESIAN_POINT('Ctrl Pts',(-3.03216770361129,-0.561081839950451,
-2.83936763243476));
#54826=CARTESIAN_POINT('Ctrl Pts',(-2.9054255848115,2.07690189898324,-2.01576285529206));
#54827=CARTESIAN_POINT('Ctrl Pts',(-2.77868346601172,2.82134070912309,0.645645397499492));
#54828=CARTESIAN_POINT('Ctrl Pts',(-2.65194134721193,0.993517739183532,
2.71840833708754));
#54829=CARTESIAN_POINT('Ctrl Pts',(-2.52519922841214,-1.74011137090692,
2.31275459608164));
#54830=CARTESIAN_POINT('Ctrl Pts',(-2.39845710961236,-2.88725288896784,
-0.201474779293297));
#54831=CARTESIAN_POINT('Ctrl Pts',(-2.27171499081257,-1.40203945796747,
-2.53201634484905));
#54832=CARTESIAN_POINT('Ctrl Pts',(-2.14497287201278,1.36143599899819,-2.55407782418169));
#54833=CARTESIAN_POINT('Ctrl Pts',(-2.01823075321299,2.88366820235333,-0.2475453713054));
#54834=CARTESIAN_POINT('Ctrl Pts',(-1.89148863441321,1.77681386339764,2.28467813548794));
#54835=CARTESIAN_POINT('Ctrl Pts',(-1.76474651561342,-0.949990728414667,
2.73392386815634));
#54836=CARTESIAN_POINT('Ctrl Pts',(-1.63800439681363,-2.81067265766773,
0.690606977484108));
#54837=CARTESIAN_POINT('Ctrl Pts',(-1.51126227801385,-2.10882057807649,
-1.98234707693312));
#54838=CARTESIAN_POINT('Ctrl Pts',(-1.38452015921406,0.515680141552461,
-2.84796401842337));
#54839=CARTESIAN_POINT('Ctrl Pts',(-1.25777804041427,2.67002136093931,-1.11704501911506));
#54840=CARTESIAN_POINT('Ctrl Pts',(-1.13103592161449,2.39007177462504,1.63229952771891));
#54841=CARTESIAN_POINT('Ctrl Pts',(-1.0042938028147,-0.0689651482364484,
2.89345486194313));
#54842=CARTESIAN_POINT('Ctrl Pts',(-0.87755168401491,-2.46508655225495,
1.51659206490182));
#54843=CARTESIAN_POINT('Ctrl Pts',(-0.750809565215129,-2.61382297691304,
-1.2429555412211));
#54844=CARTESIAN_POINT('Ctrl Pts',(-0.624067446415335,-0.379353467691326,
-2.8693122355053));
#54845=CARTESIAN_POINT('Ctrl Pts',(-0.497325327615552,2.2007090289635,-1.87961030806724));
#54846=CARTESIAN_POINT('Ctrl Pts',(-0.370583208815762,2.77486399296714,
0.823647370201196));
#54847=CARTESIAN_POINT('Ctrl Pts',(-0.243841090015978,0.818149405689422,
2.77619245786183));
#54848=CARTESIAN_POINT('Ctrl Pts',(-0.117098971216191,-1.88260982080682,
2.19721692249022));
#54849=CARTESIAN_POINT('Ctrl Pts',(0.00964314758359831,-2.87057378557703,
-0.384178546235488));
#54850=CARTESIAN_POINT('Ctrl Pts',(0.136385266383383,-1.23420704966222,
-2.61700103748139));
#54851=CARTESIAN_POINT('Ctrl Pts',(0.220880012249911,0.596079158328567,
-2.51212510012091));
#54852=CARTESIAN_POINT('Ctrl Pts',(0.263127385183173,1.28783918029104,-2.08480706438444));
#54853=CARTESIAN_POINT('',(0.,-2.44644308591689,-0.140948491901913));
#54854=CARTESIAN_POINT('Ctrl Pts',(7.21644966006352E-16,-2.45032305592699,
-0.14210232202442));
#54855=CARTESIAN_POINT('Ctrl Pts',(8.8338875589462E-16,-2.44155110065596,
-0.203186250076526));
#54856=CARTESIAN_POINT('Ctrl Pts',(3.38686818731122E-15,-2.43033064707317,
-0.263814673487791));
#54857=CARTESIAN_POINT('Ctrl Pts',(3.33066907387547E-15,-2.41660092933931,
-0.32386049272943));
#54858=CARTESIAN_POINT('Ctrl Pts',(3.19830583638964E-15,-2.39759379521507,
-0.406986669250303));
#54859=CARTESIAN_POINT('Ctrl Pts',(3.59208164640204E-15,-2.37377911238307,
-0.488997644336173));
#54860=CARTESIAN_POINT('Ctrl Pts',(3.49720252756924E-15,-2.34542524376074,
-0.569597439065157));
#54861=CARTESIAN_POINT('Ctrl Pts',(3.4494265021795E-15,-2.33114775927456,
-0.610183164214713));
#54862=CARTESIAN_POINT('Ctrl Pts',(7.57069741264941E-15,-2.31571859533792,
-0.650410667591147));
#54863=CARTESIAN_POINT('Ctrl Pts',(7.35522753814166E-15,-2.29916808587573,
-0.690239206674431));
#54864=CARTESIAN_POINT('Ctrl Pts',(7.25579217878261E-15,-2.29153033206116,
-0.708619340349916));
#54865=CARTESIAN_POINT('Ctrl Pts',(7.532000478547E-15,-2.28365373778081,
-0.726914477167649));
#54866=CARTESIAN_POINT('Ctrl Pts',(7.66053886991358E-15,-2.27554112542911,
-0.745120441436594));
#54867=CARTESIAN_POINT('Ctrl Pts',(7.75996668184755E-15,-2.26926580731891,
-0.759203231583288));
#54868=CARTESIAN_POINT('Ctrl Pts',(3.19768457339427E-15,-2.26285104588459,
-0.773228550540596));
#54869=CARTESIAN_POINT('Ctrl Pts',(3.41393580072236E-15,-2.25630175870705,
-0.787187609752352));
#54870=CARTESIAN_POINT('Ctrl Pts',(4.60505114880462E-15,-2.22022817626985,
-0.864074339494172));
#54871=CARTESIAN_POINT('Ctrl Pts',(4.21062383696699E-15,-2.18004768888068,
-0.939018970625011));
#54872=CARTESIAN_POINT('Ctrl Pts',(3.77475828372553E-15,-2.13602667510567,
-1.01172829187081));
#54873=CARTESIAN_POINT('Ctrl Pts',(3.43626937052584E-15,-2.10184038761441,
-1.06819363753749));
#54874=CARTESIAN_POINT('Ctrl Pts',(3.26078485742034E-15,-2.0653368470231,
-1.12331045289651));
#54875=CARTESIAN_POINT('Ctrl Pts',(2.27595720048157E-15,-2.02662569898502,
-1.17692586826212));
#54876=CARTESIAN_POINT('Ctrl Pts',(1.80479797808039E-15,-2.0081055911475,
-1.20257644502486));
#54877=CARTESIAN_POINT('Ctrl Pts',(4.00425887293249E-15,-1.98908002883788,
-1.22788315234873));
#54878=CARTESIAN_POINT('Ctrl Pts',(3.85802501057242E-15,-1.96956020007441,
-1.2528279157208));
#54879=CARTESIAN_POINT('Ctrl Pts',(3.79622079563643E-15,-1.96131034827578,
-1.26337055948397));
#54880=CARTESIAN_POINT('Ctrl Pts',(3.69933407994927E-15,-1.95297173899764,
-1.27384911277981));
#54881=CARTESIAN_POINT('Ctrl Pts',(3.71924713249427E-15,-1.94454661500063,
-1.28426040453742));
#54882=CARTESIAN_POINT('Ctrl Pts',(3.84297659663999E-15,-1.89219722883017,
-1.34895081537832));
#54883=CARTESIAN_POINT('Ctrl Pts',(4.49708373539599E-15,-1.83671026325253,
-1.41080165676703));
#54884=CARTESIAN_POINT('Ctrl Pts',(4.08006961549745E-15,-1.77833558535246,
-1.46954266963193));
#54885=CARTESIAN_POINT('Ctrl Pts',(3.65993532101326E-15,-1.71952413762198,
-1.52872319331129));
#54886=CARTESIAN_POINT('Ctrl Pts',(3.1868423381574E-15,-1.65778083953034,
-1.58474793350827));
#54887=CARTESIAN_POINT('Ctrl Pts',(3.91353616180368E-15,-1.59333028273939,
-1.63729649350459));
#54888=CARTESIAN_POINT('Ctrl Pts',(4.60566849652001E-15,-1.53194498828118,
-1.68734584900033));
#54889=CARTESIAN_POINT('Ctrl Pts',(1.11149137391337E-15,-1.46810302924545,
-1.73424201917144));
#54890=CARTESIAN_POINT('Ctrl Pts',(3.88578058618805E-16,-1.40198217412125,
-1.77766217724644));
#54891=CARTESIAN_POINT('Ctrl Pts',(-4.44991515592973E-17,-1.36237101346623,
-1.80367398326354));
#54892=CARTESIAN_POINT('Ctrl Pts',(-6.02384006464205E-16,-1.32194172700703,
-1.82843739125673));
#54893=CARTESIAN_POINT('Ctrl Pts',(-6.66133814775094E-16,-1.28073120830839,
-1.85187402538876));
#54894=CARTESIAN_POINT('Ctrl Pts',(-6.82859527298684E-16,-1.26991901440593,
-1.85802297572131));
#54895=CARTESIAN_POINT('Ctrl Pts',(2.61624047662099E-15,-1.25905451156175,
-1.86407964602617));
#54896=CARTESIAN_POINT('Ctrl Pts',(2.58126853225349E-15,-1.2481486999723,
-1.87003721924977));
#54897=CARTESIAN_POINT('Ctrl Pts',(2.36135975416434E-15,-1.17957133762997,
-1.9074993241362));
#54898=CARTESIAN_POINT('Ctrl Pts',(3.45138597056157E-15,-1.10925109615776,
-1.94111053406059));
#54899=CARTESIAN_POINT('Ctrl Pts',(2.96984659087229E-15,-1.03737842643735,
-1.97059975361757));
#54900=CARTESIAN_POINT('Ctrl Pts',(2.77241870009471E-15,-1.00791111766478,
-1.98269013430787));
#54901=CARTESIAN_POINT('Ctrl Pts',(-2.46248839510159E-15,-0.978182658344809,
-1.99408706860885));
#54902=CARTESIAN_POINT('Ctrl Pts',(-2.41473507855972E-15,-0.94820551795056,
-2.00476939704612));
#54903=CARTESIAN_POINT('Ctrl Pts',(-2.29412135531255E-15,-0.873603723074189,
-2.03135368308536));
#54904=CARTESIAN_POINT('Ctrl Pts',(-3.153618749677E-16,-0.797461604255296,
-2.05351583539549));
#54905=CARTESIAN_POINT('Ctrl Pts',(-8.04911692853238E-16,-0.720145712205752,
-2.0713044916701));
#54906=CARTESIAN_POINT('Ctrl Pts',(-1.28269866053302E-15,-0.644687558068625,
-2.088665724031));
#54907=CARTESIAN_POINT('Ctrl Pts',(7.54333866482025E-16,-0.568110434241961,
-2.10186068177854));
#54908=CARTESIAN_POINT('Ctrl Pts',(6.24500451351651E-16,-0.490764188682584,
-2.11088835073633));
#54909=CARTESIAN_POINT('Ctrl Pts',(5.97115216600894E-16,-0.474449859358302,
-2.11279252027091));
#54910=CARTESIAN_POINT('Ctrl Pts',(2.32068381504038E-15,-0.458097295524432,
-2.11451139813136));
#54911=CARTESIAN_POINT('Ctrl Pts',(2.26207941267376E-15,-0.441737341756347,
-2.11604251162809));
#54912=CARTESIAN_POINT('Ctrl Pts',(1.98464631383226E-15,-0.364289360248237,
-2.12329079921267));
#54913=CARTESIAN_POINT('Ctrl Pts',(1.12528087701828E-16,-0.286562636972851,
-2.12635075284766));
#54914=CARTESIAN_POINT('Ctrl Pts',(2.91433543964104E-16,-0.208904513393389,
-2.12529913794706));
#54915=CARTESIAN_POINT('Ctrl Pts',(4.70215319664734E-16,-0.131300076272357,
-2.12424825004677));
#54916=CARTESIAN_POINT('Ctrl Pts',(8.34217908837847E-16,-0.0537631215199848,
-2.11909117443756));
#54917=CARTESIAN_POINT('Ctrl Pts',(7.91033905045424E-16,0.0233492957196826,
-2.10985382433648));
#54918=CARTESIAN_POINT('Ctrl Pts',(7.48568452864568E-16,0.0991786162843468,
-2.10077017727863));
#54919=CARTESIAN_POINT('Ctrl Pts',(-8.19324922797452E-17,0.174598278903728,
-2.08774052304607));
#54920=CARTESIAN_POINT('Ctrl Pts',(6.24500451351651E-17,0.249244746088756,
-2.07074577197039));
#54921=CARTESIAN_POINT('Ctrl Pts',(1.17902742706355E-16,0.277914057791417,
-2.06421863365734));
#54922=CARTESIAN_POINT('Ctrl Pts',(-2.14494948487106E-15,0.306468994429596,
-2.0571061774594));
#54923=CARTESIAN_POINT('Ctrl Pts',(-2.08166817117217E-15,0.33488758922636,
-2.04940574541392));
#54924=CARTESIAN_POINT('Ctrl Pts',(-2.05500365971468E-15,0.346862181760419,
-2.04616105521231));
#54925=CARTESIAN_POINT('Ctrl Pts',(2.87116891261715E-15,0.358812708148608,
-2.04281183170255));
#54926=CARTESIAN_POINT('Ctrl Pts',(2.94209101525666E-15,0.370723450786355,
-2.03936214920552));
#54927=CARTESIAN_POINT('Ctrl Pts',(3.37105542846375E-15,0.442764246762624,
-2.01849713007866));
#54928=CARTESIAN_POINT('Ctrl Pts',(-2.05713060706824E-15,0.513480573994915,
-1.99392658989113));
#54929=CARTESIAN_POINT('Ctrl Pts',(-1.47104550762833E-15,0.582550239122056,
-1.96568192161834));
#54930=CARTESIAN_POINT('Ctrl Pts',(-8.94437293564184E-16,0.650503060807899,
-1.93789396429752));
#54931=CARTESIAN_POINT('Ctrl Pts',(1.17556079316216E-15,0.716862809388789,
-1.90654934330102));
#54932=CARTESIAN_POINT('Ctrl Pts',(1.05124242644195E-15,0.781294350353864,
-1.87163706534072));
#54933=CARTESIAN_POINT('Ctrl Pts',(9.3090169927015E-16,0.843664366121419,
-1.83784182632811));
#54934=CARTESIAN_POINT('Ctrl Pts',(-5.67872315242143E-16,0.904228105376908,
-1.80070315888116));
#54935=CARTESIAN_POINT('Ctrl Pts',(-1.01915004213637E-15,0.962645699073296,
-1.76017850547857));
#54936=CARTESIAN_POINT('Ctrl Pts',(-1.24401152543879E-15,0.991753864592412,
-1.7399859873653));
#54937=CARTESIAN_POINT('Ctrl Pts',(3.93452992073837E-16,1.02032856987346,
-1.71895231866749));
#54938=CARTESIAN_POINT('Ctrl Pts',(4.16333634234434E-16,1.04832369103675,
-1.69706953343435));
#54939=CARTESIAN_POINT('Ctrl Pts',(-0.00732749621205394,-2.45343455551405,
-0.00158943503992818));
#54940=CARTESIAN_POINT('Ctrl Pts',(-0.00488499747470198,-2.45380114493864,
-0.0484711203631668));
#54941=CARTESIAN_POINT('Ctrl Pts',(-0.00244249873734994,-2.45277376440421,
-0.0953339889734099));
#54942=CARTESIAN_POINT('Ctrl Pts',(2.0122792321331E-15,-2.45032305592699,
-0.142102322024455));
#54943=CARTESIAN_POINT('',(-9.7495,-1.16034898466905,-1.62253437445174));
#54944=CARTESIAN_POINT('Ctrl Pts',(-9.7495,-1.16282954126729,-1.62470330690891));
#54945=CARTESIAN_POINT('Ctrl Pts',(-9.7495,-1.20725981866171,-1.60014194947285));
#54946=CARTESIAN_POINT('Ctrl Pts',(-9.7495,-1.25060328765507,-1.5738254301256));
#54947=CARTESIAN_POINT('Ctrl Pts',(-9.7495,-1.29274237783902,-1.54577696843486));
#54948=CARTESIAN_POINT('Ctrl Pts',(-9.7495,-1.3524385713109,-1.50604221411601));
#54949=CARTESIAN_POINT('Ctrl Pts',(-9.7495,-1.40971908969672,-1.462834007833));
#54950=CARTESIAN_POINT('Ctrl Pts',(-9.7495,-1.46450253747336,-1.41649569416386));
#54951=CARTESIAN_POINT('Ctrl Pts',(-9.7495,-1.49607334894272,-1.38979167636234));
#54952=CARTESIAN_POINT('Ctrl Pts',(-9.7495,-1.52681455759462,-1.36204718991875));
#54953=CARTESIAN_POINT('Ctrl Pts',(-9.7495,-1.55670736577458,-1.33332102299628));
#54954=CARTESIAN_POINT('Ctrl Pts',(-9.7495,-1.56738673003382,-1.32305844751357));
#54955=CARTESIAN_POINT('Ctrl Pts',(-9.7495,-1.57795933994072,-1.31266897018704));
#54956=CARTESIAN_POINT('Ctrl Pts',(-9.7495,-1.58841922270742,-1.30216020256279));
#54957=CARTESIAN_POINT('Ctrl Pts',(-9.7495,-1.6412280030767,-1.24910461735225));
#54958=CARTESIAN_POINT('Ctrl Pts',(-9.7495,-1.69106280077775,-1.19311726127152));
#54959=CARTESIAN_POINT('Ctrl Pts',(-9.7495,-1.73783694628383,-1.13457522246579));
#54960=CARTESIAN_POINT('Ctrl Pts',(-9.7495,-1.77722988062818,-1.08527143153372));
#54961=CARTESIAN_POINT('Ctrl Pts',(-9.7495,-1.81445176062988,-1.03415443567273));
#54962=CARTESIAN_POINT('Ctrl Pts',(-9.7495,-1.84943663148988,-0.981424505238737));
#54963=CARTESIAN_POINT('Ctrl Pts',(-9.7495,-1.86626768742428,-0.956056385056087));
#54964=CARTESIAN_POINT('Ctrl Pts',(-9.7495,-1.88258076640227,-0.930314641382609));
#54965=CARTESIAN_POINT('Ctrl Pts',(-9.7495,-1.89836721070883,-0.904220041890348));
#54966=CARTESIAN_POINT('Ctrl Pts',(-9.7495,-1.90557741537134,-0.892301753055215));
#54967=CARTESIAN_POINT('Ctrl Pts',(-9.7495,-1.9126788769199,-0.880307889440038));
#54968=CARTESIAN_POINT('Ctrl Pts',(-9.7495,-1.91966705326428,-0.868246692004634));
#54969=CARTESIAN_POINT('Ctrl Pts',(-9.7495,-1.95856708378478,-0.801107437751533));
#54970=CARTESIAN_POINT('Ctrl Pts',(-9.7495,-1.99386743501311,-0.732046302786897));
#54971=CARTESIAN_POINT('Ctrl Pts',(-9.7495,-2.02547777089641,-0.661443958471542));
#54972=CARTESIAN_POINT('Ctrl Pts',(-9.7495,-2.05827310139699,-0.588194903969676));
#54973=CARTESIAN_POINT('Ctrl Pts',(-9.7495,-2.08709738788047,-0.513286256910227));
#54974=CARTESIAN_POINT('Ctrl Pts',(-9.7495,-2.11181354003572,-0.437098919306861));
#54975=CARTESIAN_POINT('Ctrl Pts',(-9.7495,-2.13035065415217,-0.379958416104337));
#54976=CARTESIAN_POINT('Ctrl Pts',(-9.7495,-2.14657625138598,-0.32209762752316));
#54977=CARTESIAN_POINT('Ctrl Pts',(-9.7495,-2.16041564568172,-0.263665648852278));
#54978=CARTESIAN_POINT('Ctrl Pts',(-9.7495,-2.17079519140352,-0.219841664849117));
#54979=CARTESIAN_POINT('Ctrl Pts',(-9.7495,-2.17983221265302,-0.175696166465712));
#54980=CARTESIAN_POINT('Ctrl Pts',(-9.7495,-2.18748897925106,-0.131289748942107));
#54981=CARTESIAN_POINT('Ctrl Pts',(-9.7495,-2.18975737345239,-0.118133900618595));
#54982=CARTESIAN_POINT('Ctrl Pts',(-9.7495,-2.19190458459009,-0.104955142021024));
#54983=CARTESIAN_POINT('Ctrl Pts',(-9.7495,-2.19392953304095,-0.0917550286362238));
#54984=CARTESIAN_POINT('Ctrl Pts',(-9.7495,-2.19598691316673,-0.0783435015801452));
#54985=CARTESIAN_POINT('Ctrl Pts',(-9.7495,-2.19791670474282,-0.0649186893148607));
#54986=CARTESIAN_POINT('Ctrl Pts',(-9.7495,-2.19971761564778,-0.0514875996340031));
#54987=CARTESIAN_POINT('Ctrl Pts',(-9.7495,-2.21048362106498,0.0288046479531155));
#54988=CARTESIAN_POINT('Ctrl Pts',(-9.7495,-2.21665631602757,0.109377787870744));
#54989=CARTESIAN_POINT('Ctrl Pts',(-9.7495,-2.21810551533992,0.189856369992003));
#54990=CARTESIAN_POINT('Ctrl Pts',(-9.7495,-2.21859139159652,0.216838602101243));
#54991=CARTESIAN_POINT('Ctrl Pts',(-9.7495,-2.21854594662738,0.243810439064412));
#54992=CARTESIAN_POINT('Ctrl Pts',(-9.7495,-2.21796310993972,0.270758339650537));
#54993=CARTESIAN_POINT('Ctrl Pts',(-9.7495,-2.21628399885951,0.34839332629562));
#54994=CARTESIAN_POINT('Ctrl Pts',(-9.7495,-2.21014862867717,0.42582911455849));
#54995=CARTESIAN_POINT('Ctrl Pts',(-9.7495,-2.19978974399978,0.502815302022679));
#54996=CARTESIAN_POINT('Ctrl Pts',(-9.7495,-2.18921662014655,0.581393693461284));
#54997=CARTESIAN_POINT('Ctrl Pts',(-9.7495,-2.17424335640218,0.659504469453206));
#54998=CARTESIAN_POINT('Ctrl Pts',(-9.7495,-2.15506353264355,0.736883240528982));
#54999=CARTESIAN_POINT('Ctrl Pts',(-9.7495,-2.15038816510247,0.755745467794927));
#55000=CARTESIAN_POINT('Ctrl Pts',(-9.7495,-2.14546061333694,0.774570849813381));
#55001=CARTESIAN_POINT('Ctrl Pts',(-9.7495,-2.14029345944492,0.793319915467821));
#55002=CARTESIAN_POINT('Ctrl Pts',(-9.7495,-2.11879135289761,0.871340507807307));
#55003=CARTESIAN_POINT('Ctrl Pts',(-9.7495,-2.09312591146214,0.948126958360234));
#55004=CARTESIAN_POINT('Ctrl Pts',(-9.7495,-2.06357340075898,1.02340971215714));
#55005=CARTESIAN_POINT('Ctrl Pts',(-9.7495,-2.03343217208749,1.10019217981288));
#55006=CARTESIAN_POINT('Ctrl Pts',(-9.7495,-1.99924727417101,1.17541126817356));
#55007=CARTESIAN_POINT('Ctrl Pts',(-9.7495,-1.96125645040679,1.24878274079809));
#55008=CARTESIAN_POINT('Ctrl Pts',(-9.7495,-1.92297082575374,1.32272356078602));
#55009=CARTESIAN_POINT('Ctrl Pts',(-9.7495,-1.88081965493645,1.39478889359068));
#55010=CARTESIAN_POINT('Ctrl Pts',(-9.7495,-1.83499464778345,1.46467637745762));
#55011=CARTESIAN_POINT('Ctrl Pts',(-9.7495,-1.8155367458887,1.49435152404764));
#55012=CARTESIAN_POINT('Ctrl Pts',(-9.7495,-1.79541586112841,1.52363379132999));
#55013=CARTESIAN_POINT('Ctrl Pts',(-9.7495,-1.77464411274757,1.55249878188989));
#55014=CARTESIAN_POINT('Ctrl Pts',(-9.7495,-1.76421881478994,1.56698606151671));
#55015=CARTESIAN_POINT('Ctrl Pts',(-9.7495,-1.75362655654722,1.58137198762931));
#55016=CARTESIAN_POINT('Ctrl Pts',(-9.7495,-1.74288704456025,1.59562963858262));
#55017=CARTESIAN_POINT('Ctrl Pts',(-9.7495,-1.69123008364333,1.66420881787453));
#55018=CARTESIAN_POINT('Ctrl Pts',(-9.7495,-1.63610306663109,1.72991874708502));
#55019=CARTESIAN_POINT('Ctrl Pts',(-9.7495,-1.57776314502671,1.79246368429379));
#55020=CARTESIAN_POINT('Ctrl Pts',(-9.7495,-1.51932766137129,1.85511107145994));
#55021=CARTESIAN_POINT('Ctrl Pts',(-9.7495,-1.45766830476388,1.91458402426312));
#55022=CARTESIAN_POINT('Ctrl Pts',(-9.7495,-1.39299427766318,1.97056794509669));
#55023=CARTESIAN_POINT('Ctrl Pts',(-9.7495,-1.32968169197049,2.02537335839916));
#55024=CARTESIAN_POINT('Ctrl Pts',(-9.7495,-1.263479463329,2.07683587217845));
#55025=CARTESIAN_POINT('Ctrl Pts',(-9.7495,-1.19454434316117,2.12463112085497));
#55026=CARTESIAN_POINT('Ctrl Pts',(-9.7495,-1.15559117428643,2.15163878238619));
#55027=CARTESIAN_POINT('Ctrl Pts',(-9.7495,-1.11576470790424,2.17747487576121));
#55028=CARTESIAN_POINT('Ctrl Pts',(-9.7495,-1.07508846035131,2.20207516956607));
#55029=CARTESIAN_POINT('Ctrl Pts',(-9.7495,-1.16282954126728,-1.62470330690891));
#55030=CARTESIAN_POINT('Ctrl Pts',(-9.7104670095946,-0.665448492800351,
-1.9765110105703));
#55031=CARTESIAN_POINT('Ctrl Pts',(-9.62918664625593,0.733870831796914,
-2.20998455802869));
#55032=CARTESIAN_POINT('Ctrl Pts',(-9.50565890998404,2.2663578788523,-0.643561605617013));
#55033=CARTESIAN_POINT('Ctrl Pts',(-9.37891679118423,1.77297281393676,1.55184140168292));
#55034=CARTESIAN_POINT('Ctrl Pts',(-9.25217467238445,-0.337135258971208,
2.331634562323));
#55035=CARTESIAN_POINT('Ctrl Pts',(-9.14935403578811,-1.7995037137583,1.24001182649284));
#55036=CARTESIAN_POINT('Ctrl Pts',(-9.08878077212504,-1.99264490228889,
0.288835621098305));
#55037=CARTESIAN_POINT('Ctrl Pts',(-9.07045488139523,-1.99173797669883,
0.000711821429190372));
#55038=CARTESIAN_POINT('Origin',(-9.7495,-5.69858952725515E-16,8.58067791224701E-17));
#55039=CARTESIAN_POINT('',(-9.7495,-2.4505,-3.00099698131059E-16));
#55040=CARTESIAN_POINT('Origin',(-9.7495,0.,0.));
#55041=CARTESIAN_POINT('Origin',(-9.7495,0.,0.));
#55042=CARTESIAN_POINT('',(-9.7495,1.16034898466907,-1.62253437445173));
#55043=CARTESIAN_POINT('Ctrl Pts',(-9.7495,1.07765198048948,2.20520778639847));
#55044=CARTESIAN_POINT('Ctrl Pts',(-9.7495,1.13060525254771,2.17351956564304));
#55045=CARTESIAN_POINT('Ctrl Pts',(-9.7495,1.18219250140317,2.13974889587976));
#55046=CARTESIAN_POINT('Ctrl Pts',(-9.7495,1.23227301946895,2.10388882904113));
#55047=CARTESIAN_POINT('Ctrl Pts',(-9.7495,1.30160344320515,2.0542449011196));
#55048=CARTESIAN_POINT('Ctrl Pts',(-9.7495,1.36804803363604,2.00059746133367));
#55049=CARTESIAN_POINT('Ctrl Pts',(-9.7495,1.43143746154022,1.94330837559225));
#55050=CARTESIAN_POINT('Ctrl Pts',(-9.7495,1.46335696993216,1.91446067158941));
#55051=CARTESIAN_POINT('Ctrl Pts',(-9.7495,1.4945011602568,1.88468908019348));
#55052=CARTESIAN_POINT('Ctrl Pts',(-9.7495,1.52484417134257,1.85403731928515));
#55053=CARTESIAN_POINT('Ctrl Pts',(-9.7495,1.53884696008258,1.83989204770035));
#55054=CARTESIAN_POINT('Ctrl Pts',(-9.7495,1.55267908267023,1.82555931105367));
#55055=CARTESIAN_POINT('Ctrl Pts',(-9.7495,1.56633777788309,1.81104332574806));
#55056=CARTESIAN_POINT('Ctrl Pts',(-9.7495,1.57690316529314,1.7998148001823));
#55057=CARTESIAN_POINT('Ctrl Pts',(-9.7495,1.58736167323699,1.78847985698288));
#55058=CARTESIAN_POINT('Ctrl Pts',(-9.7495,1.59770709521557,1.7770464269894));
#55059=CARTESIAN_POINT('Ctrl Pts',(-9.7495,1.65468948937111,1.71407130468052));
#55060=CARTESIAN_POINT('Ctrl Pts',(-9.7495,1.70829401366604,1.64805835503819));
#55061=CARTESIAN_POINT('Ctrl Pts',(-9.7495,1.75835312501744,1.57936654442874));
#55062=CARTESIAN_POINT('Ctrl Pts',(-9.7495,1.79722852674469,1.52602117610869));
#55063=CARTESIAN_POINT('Ctrl Pts',(-9.7495,1.83396491012993,1.47105939656799));
#55064=CARTESIAN_POINT('Ctrl Pts',(-9.7495,1.8684636308021,1.41464139286296));
#55065=CARTESIAN_POINT('Ctrl Pts',(-9.7495,1.88496848237078,1.38764993466363));
#55066=CARTESIAN_POINT('Ctrl Pts',(-9.7495,1.90096089521604,1.36032509902764));
#55067=CARTESIAN_POINT('Ctrl Pts',(-9.7495,1.91642851998693,1.33268418774228));
#55068=CARTESIAN_POINT('Ctrl Pts',(-9.7495,1.9229656492837,1.32100222534473));
#55069=CARTESIAN_POINT('Ctrl Pts',(-9.7495,1.92940937815796,1.30926315589405));
#55070=CARTESIAN_POINT('Ctrl Pts',(-9.7495,1.93575764807029,1.29747027314868));
#55071=CARTESIAN_POINT('Ctrl Pts',(-9.7495,1.97520304718045,1.22419440854714));
#55072=CARTESIAN_POINT('Ctrl Pts',(-9.7495,2.01081723995188,1.14912148554907));
#55073=CARTESIAN_POINT('Ctrl Pts',(-9.7495,2.04244747514414,1.07258637442353));
#55074=CARTESIAN_POINT('Ctrl Pts',(-9.7495,2.07431436729968,0.995478628700962));
#55075=CARTESIAN_POINT('Ctrl Pts',(-9.7495,2.10213786509534,0.916885736586536));
#55076=CARTESIAN_POINT('Ctrl Pts',(-9.7495,2.12570920792973,0.837138623357578));
#55077=CARTESIAN_POINT('Ctrl Pts',(-9.7495,2.14815951980743,0.761184208035744));
#55078=CARTESIAN_POINT('Ctrl Pts',(-9.7495,2.16675239673109,0.68418193503517));
#55079=CARTESIAN_POINT('Ctrl Pts',(-9.7495,2.18125874771835,0.606420481194756));
#55080=CARTESIAN_POINT('Ctrl Pts',(-9.7495,2.18994910664117,0.559835716712814));
#55081=CARTESIAN_POINT('Ctrl Pts',(-9.7495,2.19717192894386,0.512978600722697));
#55082=CARTESIAN_POINT('Ctrl Pts',(-9.7495,2.20286917549892,0.465913439685798));
#55083=CARTESIAN_POINT('Ctrl Pts',(-9.7495,2.2043639310029,0.453565210093529));
#55084=CARTESIAN_POINT('Ctrl Pts',(-9.7495,2.20575336285344,0.441204380991941));
#55085=CARTESIAN_POINT('Ctrl Pts',(-9.7495,2.20703543274385,0.428843731680537));
#55086=CARTESIAN_POINT('Ctrl Pts',(-9.7495,2.215097279967,0.35111812009494));
#55087=CARTESIAN_POINT('Ctrl Pts',(-9.7495,2.21893389153702,0.273272553006201));
#55088=CARTESIAN_POINT('Ctrl Pts',(-9.7495,2.21836879129015,0.195587420768878));
#55089=CARTESIAN_POINT('Ctrl Pts',(-9.7495,2.21813710572717,0.163737277900239));
#55090=CARTESIAN_POINT('Ctrl Pts',(-9.7495,2.21716493310934,0.131914139447269));
#55091=CARTESIAN_POINT('Ctrl Pts',(-9.7495,2.21543757405891,0.100137680361018));
#55092=CARTESIAN_POINT('Ctrl Pts',(-9.7495,2.21113879773801,0.0210574857432948));
#55093=CARTESIAN_POINT('Ctrl Pts',(-9.7495,2.20216614528477,-0.0577351639422519));
#55094=CARTESIAN_POINT('Ctrl Pts',(-9.7495,2.1887060785629,-0.135920959021978));
#55095=CARTESIAN_POINT('Ctrl Pts',(-9.7495,2.17556943398582,-0.212228084548267));
#55096=CARTESIAN_POINT('Ctrl Pts',(-9.7495,2.15815768408866,-0.287957857661971));
#55097=CARTESIAN_POINT('Ctrl Pts',(-9.7495,2.13660504087781,-0.362787194479743));
#55098=CARTESIAN_POINT('Ctrl Pts',(-9.7495,2.13205903634164,-0.378570618409907));
#55099=CARTESIAN_POINT('Ctrl Pts',(-9.7495,2.12732735489629,-0.394317729407546));
#55100=CARTESIAN_POINT('Ctrl Pts',(-9.7495,2.12241963127094,-0.40999912220641));
#55101=CARTESIAN_POINT('Ctrl Pts',(-9.7495,2.09918643850731,-0.484234928765601));
#55102=CARTESIAN_POINT('Ctrl Pts',(-9.7495,2.07198237645875,-0.557109856056304));
#55103=CARTESIAN_POINT('Ctrl Pts',(-9.7495,2.04101243041346,-0.628333178632409));
#55104=CARTESIAN_POINT('Ctrl Pts',(-9.7495,2.01006390965093,-0.699507228283652));
#55105=CARTESIAN_POINT('Ctrl Pts',(-9.7495,1.97535404006358,-0.769032784087818));
#55106=CARTESIAN_POINT('Ctrl Pts',(-9.7495,1.93704465465342,-0.836590516839988));
#55107=CARTESIAN_POINT('Ctrl Pts',(-9.7495,1.8993727277891,-0.903024105896846));
#55108=CARTESIAN_POINT('Ctrl Pts',(-9.7495,1.85821938417217,-0.96755546663314));
#55109=CARTESIAN_POINT('Ctrl Pts',(-9.7495,1.81370745162356,-1.02984190631639));
#55110=CARTESIAN_POINT('Ctrl Pts',(-9.7495,1.79661180052436,-1.05376419366874));
#55111=CARTESIAN_POINT('Ctrl Pts',(-9.7495,1.77902045192394,-1.07735487007615));
#55112=CARTESIAN_POINT('Ctrl Pts',(-9.7495,1.76093944008161,-1.10059264695084));
#55113=CARTESIAN_POINT('Ctrl Pts',(-9.7495,1.75332075268837,-1.11038420946216));
#55114=CARTESIAN_POINT('Ctrl Pts',(-9.7495,1.74561494379555,-1.12011319186763));
#55115=CARTESIAN_POINT('Ctrl Pts',(-9.7495,1.73783184327634,-1.12976667062739));
#55116=CARTESIAN_POINT('Ctrl Pts',(-9.7495,1.69075667140557,-1.18815460621232));
#55117=CARTESIAN_POINT('Ctrl Pts',(-9.7495,1.64077529421437,-1.2438894167514));
#55118=CARTESIAN_POINT('Ctrl Pts',(-9.7495,1.58804113169155,-1.29668604581243));
#55119=CARTESIAN_POINT('Ctrl Pts',(-9.7495,1.53615968694636,-1.34862894700437));
#55120=CARTESIAN_POINT('Ctrl Pts',(-9.7495,1.48161310229243,-1.39772847498648));
#55121=CARTESIAN_POINT('Ctrl Pts',(-9.7495,1.42452070117096,-1.44367126303871));
#55122=CARTESIAN_POINT('Ctrl Pts',(-9.7495,1.36925502008041,-1.48814407243243));
#55123=CARTESIAN_POINT('Ctrl Pts',(-9.7495,1.31160324244574,-1.52965923065524));
#55124=CARTESIAN_POINT('Ctrl Pts',(-9.7495,1.25165740686919,-1.56788681092577));
#55125=CARTESIAN_POINT('Ctrl Pts',(-9.7495,1.22178755544821,-1.58693487543071));
#55126=CARTESIAN_POINT('Ctrl Pts',(-9.7495,1.19134792456383,-1.60516593716848));
#55127=CARTESIAN_POINT('Ctrl Pts',(-9.7495,1.16034898466909,-1.62253437445172));
#55128=CARTESIAN_POINT('Origin',(-9.7495,0.,0.));
#55129=CARTESIAN_POINT('Origin',(-11.2285451186048,0.,0.));
#55130=CARTESIAN_POINT('Ctrl Pts',(-9.7495,1.16034898466907,-1.62253437445173));
#55131=CARTESIAN_POINT('Ctrl Pts',(-9.70725262706674,1.69872226327124,-1.23751887213913));
#55132=CARTESIAN_POINT('Ctrl Pts',(-9.62275788120021,2.35301974079721,0.103728689921924));
#55133=CARTESIAN_POINT('Ctrl Pts',(-9.49601576240043,1.19113795339939,2.03448789178737));
#55134=CARTESIAN_POINT('Ctrl Pts',(-9.36927364360064,-1.05771687947754,
2.10445274652685));
#55135=CARTESIAN_POINT('Ctrl Pts',(-9.28011676233542,-1.96094440164537,
0.806069483628623));
#55136=CARTESIAN_POINT('Ctrl Pts',(-9.23320725400347,-1.99753352956653,
0.0741460916094852));
#55137=CARTESIAN_POINT('Ctrl Pts',(-9.22854511860477,-1.99701091303081,
0.00134739702958217));
#55138=CARTESIAN_POINT('Ctrl Pts',(-10.0126273851832,1.42545942445495,-1.99324250386965));
#55139=CARTESIAN_POINT('Ctrl Pts',(-9.97038001224991,2.08683740125135,-1.52026068237975));
#55140=CARTESIAN_POINT('Ctrl Pts',(-9.88588526638338,2.89062532890015,0.127428076026371));
#55141=CARTESIAN_POINT('Ctrl Pts',(-9.75914314758361,1.46328289500202,2.49931699652835));
#55142=CARTESIAN_POINT('Ctrl Pts',(-9.63240102878381,-1.2993784750769,2.58526705369799));
#55143=CARTESIAN_POINT('Ctrl Pts',(-9.50565890998404,-2.8767336334322,0.317830015974396));
#55144=CARTESIAN_POINT('Ctrl Pts',(-9.37891679118423,-1.83166120490144,
-2.24126795020257));
#55145=CARTESIAN_POINT('Ctrl Pts',(-9.25217467238446,0.883542867790515,
-2.75597710770364));
#55146=CARTESIAN_POINT('Ctrl Pts',(-9.12543255358466,2.79311408050666,-0.758535600360605));
#55147=CARTESIAN_POINT('Ctrl Pts',(-8.99869043478488,2.15620672142397,1.93074660360672));
#55148=CARTESIAN_POINT('Ctrl Pts',(-8.8719483159851,-0.446574495801375,
2.8595936543393));
#55149=CARTESIAN_POINT('Ctrl Pts',(-8.7452061971853,-2.64219320892422,1.1813777274502));
#55150=CARTESIAN_POINT('Ctrl Pts',(-8.61846407838552,-2.42888879364233,
-1.57395843532259));
#55151=CARTESIAN_POINT('Ctrl Pts',(-8.49172195958573,-0.00112366212568968,
-2.89427081971438));
#55152=CARTESIAN_POINT('Ctrl Pts',(-8.36497984078595,2.4276640081396,-1.5758406156409));
#55153=CARTESIAN_POINT('Ctrl Pts',(-8.23823772198616,2.64311229295518,1.17931450649545));
#55154=CARTESIAN_POINT('Ctrl Pts',(-8.11149560318636,0.448791983620454,
2.85926663546641));
#55155=CARTESIAN_POINT('Ctrl Pts',(-7.98475348438658,-2.15469893161674,
1.93238085090762));
#55156=CARTESIAN_POINT('Ctrl Pts',(-7.85801136558679,-2.79371625747268,
-0.756288504049397));
#55157=CARTESIAN_POINT('Ctrl Pts',(-7.73126924678701,-0.885657380199097,
-2.7554370180037));
#55158=CARTESIAN_POINT('Ctrl Pts',(-7.60452712798722,1.82986956127592,-2.24240942758177));
#55159=CARTESIAN_POINT('Ctrl Pts',(-7.47778500918743,2.87707496001139,0.315059086878021));
#55160=CARTESIAN_POINT('Ctrl Pts',(-7.35104289038765,1.3012047485017,2.58528309394231));
#55161=CARTESIAN_POINT('Ctrl Pts',(-7.22430077158787,-1.46099479274749,
2.49846287982005));
#55162=CARTESIAN_POINT('Ctrl Pts',(-7.09755865278807,-2.89118184349023,
0.133753783635275));
#55163=CARTESIAN_POINT('Ctrl Pts',(-6.97081653398828,-1.68543182040245,
-2.35290078342189));
#55164=CARTESIAN_POINT('Ctrl Pts',(-6.8440744151885,1.05695354983856,-2.69437779863599));
#55165=CARTESIAN_POINT('Ctrl Pts',(-6.71733229638871,2.83569733845996,-0.579347157962499));
#55166=CARTESIAN_POINT('Ctrl Pts',(-6.59059017758893,2.02909017185975,2.06388362035805));
#55167=CARTESIAN_POINT('Ctrl Pts',(-6.46384805878913,-0.627471198984668,
2.82543844736086));
#55168=CARTESIAN_POINT('Ctrl Pts',(-6.33710593998935,-2.71195696734964,
1.01099551533597));
#55169=CARTESIAN_POINT('Ctrl Pts',(-6.21036382118956,-2.32390787085462,
-1.72518831798258));
#55170=CARTESIAN_POINT('Ctrl Pts',(-6.08362170238978,0.182885476550568,
-2.88849016397656));
#55171=CARTESIAN_POINT('Ctrl Pts',(-5.95687958358999,2.52293918816451,-1.41830898525316));
#55172=CARTESIAN_POINT('Ctrl Pts',(-5.8301374647902,2.56278858986834,1.34496734847618));
#55173=CARTESIAN_POINT('Ctrl Pts',(-5.70339534599041,0.266102340043448,
2.88201527918852));
#55174=CARTESIAN_POINT('Ctrl Pts',(-5.57665322719064,-2.27319370090067,
1.79148344201757));
#55175=CARTESIAN_POINT('Ctrl Pts',(-5.44991110839083,-2.73998241681994,
-0.932372715364727));
#55176=CARTESIAN_POINT('Ctrl Pts',(-5.32316898959106,-0.708685014056901,
-2.80616964485284));
#55177=CARTESIAN_POINT('Ctrl Pts',(-5.19642687079127,1.9687319350458,-2.12153649338652));
#55178=CARTESIAN_POINT('Ctrl Pts',(-5.06968475199148,2.85122425683898,0.497335663363999));
#55179=CARTESIAN_POINT('Ctrl Pts',(-4.94294263319169,1.13420948196707,2.66277888226879));
#55180=CARTESIAN_POINT('Ctrl Pts',(-4.81620051439191,-1.61688235310285,
2.40052368891968));
#55181=CARTESIAN_POINT('Ctrl Pts',(-4.68945839559212,-2.89383649406469,
-0.0503276311953479));
#55182=CARTESIAN_POINT('Ctrl Pts',(-4.56271627679233,-1.5324332750719,-2.45529443902181));
#55183=CARTESIAN_POINT('Ctrl Pts',(-4.43597415799255,1.22611405286081,-2.62172974469429));
#55184=CARTESIAN_POINT('Ctrl Pts',(-4.30923203919275,2.86679344245922,-0.397891798263646));
#55185=CARTESIAN_POINT('Ctrl Pts',(-4.18248992039298,1.89377105798942,2.18871051186493));
#55186=CARTESIAN_POINT('Ctrl Pts',(-4.05574780159318,-0.805832914320809,
2.77983018168796));
#55187=CARTESIAN_POINT('Ctrl Pts',(-3.9290056827934,-2.77074603430605,0.836533883533555));
#55188=CARTESIAN_POINT('Ctrl Pts',(-3.80226356399361,-2.209525349802,-1.86944383529057));
#55189=CARTESIAN_POINT('Ctrl Pts',(-3.67552144519382,0.366155198045445,
-2.87101948717351));
#55190=CARTESIAN_POINT('Ctrl Pts',(-3.54877932639404,2.60800615217148,-1.25504041194532));
#55191=CARTESIAN_POINT('Ctrl Pts',(-3.42203720759424,2.47209587427006,1.50517922930694));
#55192=CARTESIAN_POINT('Ctrl Pts',(-3.29529508879447,0.0823359556551343,
2.89310271424892));
#55193=CARTESIAN_POINT('Ctrl Pts',(-3.16855296999467,-2.38249098169967,
1.64333783818743));
#55194=CARTESIAN_POINT('Ctrl Pts',(-3.04181085119489,-2.67516249955718,
-1.10468462414187));
#55195=CARTESIAN_POINT('Ctrl Pts',(-2.9150687323951,-0.528845266442932,
-2.84554831463556));
#55196=CARTESIAN_POINT('Ctrl Pts',(-2.78832661359532,2.09962872632452,-1.99207975690403));
#55197=CARTESIAN_POINT('Ctrl Pts',(-2.66158449479553,2.81383736093294,0.677600014437121));
#55198=CARTESIAN_POINT('Ctrl Pts',(-2.53484237599574,0.962625166914014,
2.72950093272979));
#55199=CARTESIAN_POINT('Ctrl Pts',(-2.40810025719596,-1.76622796476978,
2.29287187358059));
#55200=CARTESIAN_POINT('Ctrl Pts',(-2.28135813839617,-2.88478248307408,
-0.23420542400883));
#55201=CARTESIAN_POINT('Ctrl Pts',(-2.15461601959638,-1.37323455557573,
-2.5477538507472));
#55202=CARTESIAN_POINT('Ctrl Pts',(-2.02787390079659,1.39031387507737,-2.53847406282439));
#55203=CARTESIAN_POINT('Ctrl Pts',(-1.9011317819968,2.88628991979766,-0.214826525661565));
#55204=CARTESIAN_POINT('Ctrl Pts',(-1.77438966319702,1.75079050957589,2.30468173290378));
#55205=CARTESIAN_POINT('Ctrl Pts',(-1.64764754439723,-0.980935816608061,
2.72297467965007));
#55206=CARTESIAN_POINT('Ctrl Pts',(-1.52090542559744,-2.81832143441497,
0.6586874317792));
#55207=CARTESIAN_POINT('Ctrl Pts',(-1.39416330679766,-2.08620889714375,
-2.0061351812584));
#55208=CARTESIAN_POINT('Ctrl Pts',(-1.26742118799787,0.54795471416747,-2.84193313070915));
#55209=CARTESIAN_POINT('Ctrl Pts',(-1.14067906919808,2.682499493013,-1.0866927432457));
#55210=CARTESIAN_POINT('Ctrl Pts',(-1.0139369503983,2.37144197069276,1.65929890390176));
#55211=CARTESIAN_POINT('Ctrl Pts',(-0.887194831598508,-0.101841824517894,
2.89248868044766));
#55212=CARTESIAN_POINT('Ctrl Pts',(-0.760452712798723,-2.48199930473078,
1.48853527627866));
#55213=CARTESIAN_POINT('Ctrl Pts',(-0.633710593998933,-2.59980356409773,
-1.27251177686141));
#55214=CARTESIAN_POINT('Ctrl Pts',(-0.506968475199149,-0.346322090654253,
-2.8734427654469));
#55215=CARTESIAN_POINT('Ctrl Pts',(-0.380226356399359,2.22098961772557,
-1.85450674800193));
#55216=CARTESIAN_POINT('Ctrl Pts',(-0.253484237599575,2.76708226469713,
0.855007614199791));
#55217=CARTESIAN_POINT('Ctrl Pts',(-0.126742118799785,0.783023399402025,
2.78546711749175));
#55218=CARTESIAN_POINT('Ctrl Pts',(-0.0422473729332622,-1.00451454043688,
2.37845189560396));
#55219=CARTESIAN_POINT('Ctrl Pts',(0.,-1.6158113816168,1.84230937386683));
#55220=CARTESIAN_POINT('Ctrl Pts',(-9.92491825678878,1.33708927785966,-1.86967312739701));
#55221=CARTESIAN_POINT('Ctrl Pts',(-9.88267088385552,1.95746568859131,-1.42601341229954));
#55222=CARTESIAN_POINT('Ctrl Pts',(-9.79817613798899,2.71142346619917,0.119528280658224));
#55223=CARTESIAN_POINT('Ctrl Pts',(-9.67143401918922,1.37256791446781,2.34437396161469));
#55224=CARTESIAN_POINT('Ctrl Pts',(-9.54469190038942,-1.21882460987711,
2.42499561797428));
#55225=CARTESIAN_POINT('Ctrl Pts',(-9.41794978158964,-2.69839297459568,
0.298126414018276));
#55226=CARTESIAN_POINT('Ctrl Pts',(-9.29120766278985,-1.71810892385214,
-2.10232244679445));
#55227=CARTESIAN_POINT('Ctrl Pts',(-9.16446554399006,0.828768377959128,
-2.58512264713969));
#55228=CARTESIAN_POINT('Ctrl Pts',(-9.03772342519027,2.61995734484851,-0.711510829924037));
#55229=CARTESIAN_POINT('Ctrl Pts',(-8.91098130639049,2.02253451666453,1.81105160740271));
#55230=CARTESIAN_POINT('Ctrl Pts',(-8.7842391875907,-0.418889489141318,
2.68231557395229));
#55231=CARTESIAN_POINT('Ctrl Pts',(-8.65749706879092,-2.4783926845459,1.10813921839959));
#55232=CARTESIAN_POINT('Ctrl Pts',(-8.53075494999112,-2.27831189536272,
-1.47638221864597));
#55233=CARTESIAN_POINT('Ctrl Pts',(-8.40401283119134,-0.00105400164635133,
-2.71484295790593));
#55234=CARTESIAN_POINT('Ctrl Pts',(-8.27727071239155,2.27716303939722,-1.47814771479367));
#55235=CARTESIAN_POINT('Ctrl Pts',(-8.15052859359177,2.47925479074279,1.10620390507598));
#55236=CARTESIAN_POINT('Ctrl Pts',(-8.02378647479198,0.420969505686005,
2.68200882833674));
#55237=CARTESIAN_POINT('Ctrl Pts',(-7.8970443559922,-2.02112020100608,1.81258454092991));
#55238=CARTESIAN_POINT('Ctrl Pts',(-7.7703022371924,-2.62052219036486,-0.709403040440553));
#55239=CARTESIAN_POINT('Ctrl Pts',(-7.64356011839262,-0.830751802966448,
-2.58461603984207));
#55240=CARTESIAN_POINT('Ctrl Pts',(-7.51681799959283,1.71642835165184,-2.1033931592528));
#55241=CARTESIAN_POINT('Ctrl Pts',(-7.39007588079305,2.69871314092343,0.29552726631833));
#55242=CARTESIAN_POINT('Ctrl Pts',(-7.26333376199325,1.2205376650317,2.42501066381727));
#55243=CARTESIAN_POINT('Ctrl Pts',(-7.13659164319347,-1.37042166116963,
2.34357279514644));
#55244=CARTESIAN_POINT('Ctrl Pts',(-7.00984952439368,-2.71194548013981,
0.125461831395346));
#55245=CARTESIAN_POINT('Ctrl Pts',(-6.8831074055939,-1.58094490587501,-2.20703469731096));
#55246=CARTESIAN_POINT('Ctrl Pts',(-6.75636528679411,0.99142861202466,-2.52734213493084));
#55247=CARTESIAN_POINT('Ctrl Pts',(-6.62962316799432,2.65990068988442,-0.543431022855178));
#55248=CARTESIAN_POINT('Ctrl Pts',(-6.50288104919453,1.90329844964998,1.93593490785338));
#55249=CARTESIAN_POINT('Ctrl Pts',(-6.37613893039475,-0.588571654818552,
2.6502777900277));
#55250=CARTESIAN_POINT('Ctrl Pts',(-6.24939681159495,-2.54383149800739,
0.948319706845946));
#55251=CARTESIAN_POINT('Ctrl Pts',(-6.12265469279518,-2.17983917573905,
-1.61823673314677));
#55252=CARTESIAN_POINT('Ctrl Pts',(-5.99591257399538,0.171547646728372,
-2.70942066901194));
#55253=CARTESIAN_POINT('Ctrl Pts',(-5.8691704551956,2.36653171553907,-1.3303821240644));
#55254=CARTESIAN_POINT('Ctrl Pts',(-5.74242833639581,2.40391068742223,1.26158723978164));
#55255=CARTESIAN_POINT('Ctrl Pts',(-5.61568621759602,0.2496055514323,2.70334718920823));
#55256=CARTESIAN_POINT('Ctrl Pts',(-5.48894409879623,-2.13226898768766,
1.68042194726145));
#55257=CARTESIAN_POINT('Ctrl Pts',(-5.36220197999646,-2.57011953353548,
-0.874571060596665));
#55258=CARTESIAN_POINT('Ctrl Pts',(-5.23545986119665,-0.664750688387785,
-2.63220354056913));
#55259=CARTESIAN_POINT('Ctrl Pts',(-5.10871774239688,1.84668207047434,-1.99001363997416));
#55260=CARTESIAN_POINT('Ctrl Pts',(-4.98197562359709,2.67446503014315,0.466503761224565));
#55261=CARTESIAN_POINT('Ctrl Pts',(-4.85523350479731,1.06389512824245,2.49770216655173));
#55262=CARTESIAN_POINT('Ctrl Pts',(-4.72849138599751,-1.51664510459213,
2.25170526122123));
#55263=CARTESIAN_POINT('Ctrl Pts',(-4.60174926719773,-2.71443555790608,
-0.0472076124349324));
#55264=CARTESIAN_POINT('Ctrl Pts',(-4.47500714839794,-1.43743137544406,
-2.30308054517917));
#55265=CARTESIAN_POINT('Ctrl Pts',(-4.34826502959816,1.15010215330408,-2.45919783540443));
#55266=CARTESIAN_POINT('Ctrl Pts',(-4.22152291079836,2.68906901732139,-0.373224834098681));
#55267=CARTESIAN_POINT('Ctrl Pts',(-4.09478079199859,1.77636832933829,2.05302326221759));
#55268=CARTESIAN_POINT('Ctrl Pts',(-3.96803867319879,-0.755875987067642,
2.60749697005709));
#55269=CARTESIAN_POINT('Ctrl Pts',(-3.84129655439901,-2.59897598667836,
0.784673675763648));
#55270=CARTESIAN_POINT('Ctrl Pts',(-3.71455443559922,-2.07254770195159,
-1.75354925215331));
#55271=CARTESIAN_POINT('Ctrl Pts',(-3.58781231679943,0.343455717462007,
-2.69303307198214));
#55272=CARTESIAN_POINT('Ctrl Pts',(-3.46107019799965,2.44632502534674,-1.17723524731985));
#55273=CARTESIAN_POINT('Ctrl Pts',(-3.33432807919985,2.31884038971607,1.41186692110364));
#55274=CARTESIAN_POINT('Ctrl Pts',(-3.20758596040008,0.0772316079995686,
2.71374726814691));
#55275=CARTESIAN_POINT('Ctrl Pts',(-3.08084384160028,-2.23479047637292,
1.54146050434346));
#55276=CARTESIAN_POINT('Ctrl Pts',(-2.9541017228005,-2.50931807200182,-1.03620063890721));
#55277=CARTESIAN_POINT('Ctrl Pts',(-2.82735960400071,-0.496059953216865,
-2.66914096315693));
#55278=CARTESIAN_POINT('Ctrl Pts',(-2.70061748520092,1.96946402632828,-1.86858246394218));
#55279=CARTESIAN_POINT('Ctrl Pts',(-2.57387536640114,2.63939590310186,0.635592776923738));
#55280=CARTESIAN_POINT('Ctrl Pts',(-2.44713324760135,0.902948037100895,
2.56028784015119));
#55281=CARTESIAN_POINT('Ctrl Pts',(-2.32039112880156,-1.65673216188006,
2.15072722876193));
#55282=CARTESIAN_POINT('Ctrl Pts',(-2.19364901000178,-2.70594284263865,
-0.219686057622113));
#55283=CARTESIAN_POINT('Ctrl Pts',(-2.06690689120199,-1.28810204538003,
-2.38980801418622));
#55284=CARTESIAN_POINT('Ctrl Pts',(-1.9401647724022,1.30412254697203,-2.38110351883578));
#55285=CARTESIAN_POINT('Ctrl Pts',(-1.81342265360241,2.7073568271026,-0.201508537622347));
#55286=CARTESIAN_POINT('Ctrl Pts',(-1.68668053480263,1.64225173861224,2.16180494588469));
#55287=CARTESIAN_POINT('Ctrl Pts',(-1.55993841600284,-0.920123533615601,
2.55416617658939));
#55288=CARTESIAN_POINT('Ctrl Pts',(-1.43319629720305,-2.64360199025601,
0.617852663768124));
#55289=CARTESIAN_POINT('Ctrl Pts',(-1.30645417840327,-1.95687614806216,
-1.88176653419882));
#55290=CARTESIAN_POINT('Ctrl Pts',(-1.17971205960348,0.513984726956457,
-2.66574989948821));
#55291=CARTESIAN_POINT('Ctrl Pts',(-1.05296994080369,2.51620021477854,-1.01932414938945));
#55292=CARTESIAN_POINT('Ctrl Pts',(-0.926227822003905,2.22442643942114,
1.55643207734212));
#55293=CARTESIAN_POINT('Ctrl Pts',(-0.799485703204116,-0.0955282270855373,
2.71317130084975));
#55294=CARTESIAN_POINT('Ctrl Pts',(-0.672743584404332,-2.32812986541486,
1.39625479581018));
#55295=CARTESIAN_POINT('Ctrl Pts',(-0.546001465604542,-2.43863094975541,
-1.19362348980373));
#55296=CARTESIAN_POINT('Ctrl Pts',(-0.419259346804758,-0.324852146722302,
-2.6953061211767));
#55297=CARTESIAN_POINT('Ctrl Pts',(-0.292517228004968,2.08330125232009,
-1.73953817690733));
#55298=CARTESIAN_POINT('Ctrl Pts',(-0.165775109205184,2.59553934935526,
0.802002143184149));
#55299=CARTESIAN_POINT('Ctrl Pts',(-0.0390329904053946,0.734480528657613,
2.61278444881232));
#55300=CARTESIAN_POINT('Ctrl Pts',(0.0454617554611288,-0.942240514482439,
2.23100178998994));
#55301=CARTESIAN_POINT('Ctrl Pts',(0.0877091283943909,-1.51564052707394,
1.72809696862439));
#55302=CARTESIAN_POINT('Ctrl Pts',(-9.83720912839439,1.24871913126436,-1.74610375092437));
#55303=CARTESIAN_POINT('Ctrl Pts',(-9.79496175546113,1.82809397593127,-1.33176614221934));
#55304=CARTESIAN_POINT('Ctrl Pts',(-9.71046700959461,2.53222160349819,0.111628485290073));
#55305=CARTESIAN_POINT('Ctrl Pts',(-9.58372489079481,1.2818529339336,2.18943092670103));
#55306=CARTESIAN_POINT('Ctrl Pts',(-9.45698277199503,-1.13827074467732,
2.26472418225056));
#55307=CARTESIAN_POINT('Ctrl Pts',(-9.33024065319525,-2.52005231575915,
0.278422812062161));
#55308=CARTESIAN_POINT('Ctrl Pts',(-9.20349853439546,-1.60455664280285,
-1.96337694338634));
#55309=CARTESIAN_POINT('Ctrl Pts',(-9.07675641559566,0.773993888127739,
-2.41426818657572));
#55310=CARTESIAN_POINT('Ctrl Pts',(-8.9500142967959,2.44680060919036,-0.664486059487474));
#55311=CARTESIAN_POINT('Ctrl Pts',(-8.82327217799609,1.88886231190509,1.69135661119872));
#55312=CARTESIAN_POINT('Ctrl Pts',(-8.69653005919631,-0.391204482481263,
2.50503749356526));
#55313=CARTESIAN_POINT('Ctrl Pts',(-8.56978794039652,-2.31459216016759,
1.034900709349));
#55314=CARTESIAN_POINT('Ctrl Pts',(-8.44304582159674,-2.12773499708311,
-1.37880600196934));
#55315=CARTESIAN_POINT('Ctrl Pts',(-8.31630370279695,-0.00098434116701247,
-2.53541509609748));
#55316=CARTESIAN_POINT('Ctrl Pts',(-8.18956158399716,2.12666207065484,-1.38045481394644));
#55317=CARTESIAN_POINT('Ctrl Pts',(-8.06281946519737,2.31539728853041,1.03309330365651));
#55318=CARTESIAN_POINT('Ctrl Pts',(-7.93607734639759,0.393147027751557,
2.50475102120706));
#55319=CARTESIAN_POINT('Ctrl Pts',(-7.8093352275978,-1.88754147039541,1.69278823095219));
#55320=CARTESIAN_POINT('Ctrl Pts',(-7.68259310879802,-2.44732812325703,
-0.662517576831704));
#55321=CARTESIAN_POINT('Ctrl Pts',(-7.55585098999822,-0.775846225733801,
-2.41379506168045));
#55322=CARTESIAN_POINT('Ctrl Pts',(-7.42910887119844,1.60298714202776,-1.96437689092383));
#55323=CARTESIAN_POINT('Ctrl Pts',(-7.30236675239865,2.52035132183546,0.275995445758637));
#55324=CARTESIAN_POINT('Ctrl Pts',(-7.17562463359886,1.1398705815617,2.26473823369224));
#55325=CARTESIAN_POINT('Ctrl Pts',(-7.04888251479908,-1.27984852959178,
2.18868271047284));
#55326=CARTESIAN_POINT('Ctrl Pts',(-6.92214039599929,-2.53270911678938,
0.117169879155415));
#55327=CARTESIAN_POINT('Ctrl Pts',(-6.7953982771995,-1.47645799134757,-2.06116861120004));
#55328=CARTESIAN_POINT('Ctrl Pts',(-6.66865615839972,0.925903674210762,
-2.36030647122569));
#55329=CARTESIAN_POINT('Ctrl Pts',(-6.54191403959993,2.48410404130888,-0.507514887747857));
#55330=CARTESIAN_POINT('Ctrl Pts',(-6.41517192080014,1.7775067274402,1.8079861953487));
#55331=CARTESIAN_POINT('Ctrl Pts',(-6.28842980200036,-0.549672110652437,
2.47511713269453));
#55332=CARTESIAN_POINT('Ctrl Pts',(-6.16168768320056,-2.37570602866514,
0.885643898355919));
#55333=CARTESIAN_POINT('Ctrl Pts',(-6.03494556440078,-2.0357704806235,-1.51128514831095));
#55334=CARTESIAN_POINT('Ctrl Pts',(-5.908203445601,0.160209816906179,-2.53035117404734));
#55335=CARTESIAN_POINT('Ctrl Pts',(-5.78146132680121,2.21012424291363,-1.24245526287563));
#55336=CARTESIAN_POINT('Ctrl Pts',(-5.65471920800142,2.24503278497613,1.17820713108709));
#55337=CARTESIAN_POINT('Ctrl Pts',(-5.52797708920164,0.233108762821149,
2.52467909922792));
#55338=CARTESIAN_POINT('Ctrl Pts',(-5.40123497040184,-1.99134427447465,
1.56936045250534));
#55339=CARTESIAN_POINT('Ctrl Pts',(-5.27449285160206,-2.40025665025101,
-0.816769405828604));
#55340=CARTESIAN_POINT('Ctrl Pts',(-5.14775073280227,-0.620816362718671,
-2.45823743628542));
#55341=CARTESIAN_POINT('Ctrl Pts',(-5.02100861400248,1.72463220590289,-1.8584907865618));
#55342=CARTESIAN_POINT('Ctrl Pts',(-4.8942664952027,2.49770580344732,0.435671859085126));
#55343=CARTESIAN_POINT('Ctrl Pts',(-4.7675243764029,0.993580774517831,2.33262545083467));
#55344=CARTESIAN_POINT('Ctrl Pts',(-4.64078225760313,-1.41640785608141,
2.10288683352277));
#55345=CARTESIAN_POINT('Ctrl Pts',(-4.51404013880334,-2.53503462174748,
-0.0440875936745136));
#55346=CARTESIAN_POINT('Ctrl Pts',(-4.38729802000355,-1.34242947581622,
-2.15086665133653));
#55347=CARTESIAN_POINT('Ctrl Pts',(-4.26055590120377,1.07409025374736,-2.29666592611456));
#55348=CARTESIAN_POINT('Ctrl Pts',(-4.13381378240397,2.51134459218356,-0.348557869933718));
#55349=CARTESIAN_POINT('Ctrl Pts',(-4.0070716636042,1.65896560068717,1.91733601257026));
#55350=CARTESIAN_POINT('Ctrl Pts',(-3.8803295448044,-0.705919059814479,
2.43516375842623));
#55351=CARTESIAN_POINT('Ctrl Pts',(-3.75358742600462,-2.42720593905067,
0.732813467993737));
#55352=CARTESIAN_POINT('Ctrl Pts',(-3.62684530720482,-1.93557005410118,
-1.63765466901604));
#55353=CARTESIAN_POINT('Ctrl Pts',(-3.50010318840505,0.32075623687857,-2.51504665679077));
#55354=CARTESIAN_POINT('Ctrl Pts',(-3.37336106960525,2.28464389852199,-1.09943008269438));
#55355=CARTESIAN_POINT('Ctrl Pts',(-3.24661895080547,2.16558490516209,1.31855461290034));
#55356=CARTESIAN_POINT('Ctrl Pts',(-3.11987683200568,0.0721272603440025,
2.5343918220449));
#55357=CARTESIAN_POINT('Ctrl Pts',(-2.9931347132059,-2.08708997104618,1.43958317049948));
#55358=CARTESIAN_POINT('Ctrl Pts',(-2.86639259440611,-2.34347364444646,
-0.967716653672553));
#55359=CARTESIAN_POINT('Ctrl Pts',(-2.73965047560632,-0.463274639990797,
-2.4927336116783));
#55360=CARTESIAN_POINT('Ctrl Pts',(-2.61290835680653,1.83929932633204,-1.74508517098032));
#55361=CARTESIAN_POINT('Ctrl Pts',(-2.48616623800675,2.46495444527078,0.593585539410353));
#55362=CARTESIAN_POINT('Ctrl Pts',(-2.35942411920696,0.843270907287779,
2.39107474757259));
#55363=CARTESIAN_POINT('Ctrl Pts',(-2.23268200040717,-1.54723635899034,
2.00858258394327));
#55364=CARTESIAN_POINT('Ctrl Pts',(-2.10593988160738,-2.52710320220323,
-0.205166691235395));
#55365=CARTESIAN_POINT('Ctrl Pts',(-1.9791977628076,-1.20296953518432,-2.23186217762525));
#55366=CARTESIAN_POINT('Ctrl Pts',(-1.85245564400781,1.21793121886668,-2.22373297484717));
#55367=CARTESIAN_POINT('Ctrl Pts',(-1.72571352520802,2.52842373440753,-0.188190549583124));
#55368=CARTESIAN_POINT('Ctrl Pts',(-1.59897140640823,1.53371296764859,2.0189281588656));
#55369=CARTESIAN_POINT('Ctrl Pts',(-1.47222928760845,-0.859311250623144,
2.38535767352872));
#55370=CARTESIAN_POINT('Ctrl Pts',(-1.34548716880866,-2.46888254609704,
0.577017895757046));
#55371=CARTESIAN_POINT('Ctrl Pts',(-1.21874505000888,-1.82754339898057,
-1.75739788713925));
#55372=CARTESIAN_POINT('Ctrl Pts',(-1.09200293120909,0.480014739745447,
-2.48956666826728));
#55373=CARTESIAN_POINT('Ctrl Pts',(-0.965260812409302,2.34990093654407,
-0.951955555533188));
#55374=CARTESIAN_POINT('Ctrl Pts',(-0.838518693609514,2.07741090814953,
1.45356525078249));
#55375=CARTESIAN_POINT('Ctrl Pts',(-0.711776574809726,-0.0892146296531849,
2.53385392125184));
#55376=CARTESIAN_POINT('Ctrl Pts',(-0.585034456009941,-2.17426042609893,
1.3039743153417));
#55377=CARTESIAN_POINT('Ctrl Pts',(-0.458292337210151,-2.27745833541309,
-1.11473520274606));
#55378=CARTESIAN_POINT('Ctrl Pts',(-0.331550218410368,-0.303382202790349,
-2.51716947690649));
#55379=CARTESIAN_POINT('Ctrl Pts',(-0.204808099610577,1.94561288691461,
-1.62456960581273));
#55380=CARTESIAN_POINT('Ctrl Pts',(-0.078065980810793,2.42399643401339,
0.74899667216851));
#55381=CARTESIAN_POINT('Ctrl Pts',(0.0486761379889964,0.685937657913202,
2.44010178013288));
#55382=CARTESIAN_POINT('Ctrl Pts',(0.13317088385552,-0.879966488528001,
2.08355168437591));
#55383=CARTESIAN_POINT('Ctrl Pts',(0.175418256788782,-1.41546967253109,
1.61388456338194));
#55384=CARTESIAN_POINT('Ctrl Pts',(-9.7495,1.16034898466907,-1.62253437445173));
#55385=CARTESIAN_POINT('Ctrl Pts',(-9.70725262706674,1.69872226327124,-1.23751887213913));
#55386=CARTESIAN_POINT('Ctrl Pts',(-9.62275788120021,2.35301974079721,0.103728689921924));
#55387=CARTESIAN_POINT('Ctrl Pts',(-9.49601576240043,1.19113795339939,2.03448789178737));
#55388=CARTESIAN_POINT('Ctrl Pts',(-9.36927364360064,-1.05771687947754,
2.10445274652685));
#55389=CARTESIAN_POINT('Ctrl Pts',(-9.24253152480086,-2.34171165692263,
0.258719210106041));
#55390=CARTESIAN_POINT('Ctrl Pts',(-9.11578940600106,-1.49100436175355,
-1.82443143997822));
#55391=CARTESIAN_POINT('Ctrl Pts',(-8.98904728720129,0.719219398296349,
-2.24341372601176));
#55392=CARTESIAN_POINT('Ctrl Pts',(-8.86230516840148,2.27364387353221,-0.617461289050906));
#55393=CARTESIAN_POINT('Ctrl Pts',(-8.73556304960172,1.75519010714565,1.57166161499472));
#55394=CARTESIAN_POINT('Ctrl Pts',(-8.60882093080191,-0.363519475821205,
2.32775941317825));
#55395=CARTESIAN_POINT('Ctrl Pts',(-8.48207881200213,-2.15079163578927,
0.961662200298393));
#55396=CARTESIAN_POINT('Ctrl Pts',(-8.35533669320235,-1.97715809880351,
-1.28122978529272));
#55397=CARTESIAN_POINT('Ctrl Pts',(-8.22859457440256,-0.000914680687675627,
-2.35598723428903));
#55398=CARTESIAN_POINT('Ctrl Pts',(-8.10185245560277,1.97616110191247,-1.28276191309921));
#55399=CARTESIAN_POINT('Ctrl Pts',(-7.97511033680299,2.15153978631802,0.959982702237039));
#55400=CARTESIAN_POINT('Ctrl Pts',(-7.8483682180032,0.36532454981711,2.32749321407739));
#55401=CARTESIAN_POINT('Ctrl Pts',(-7.7216260992034,-1.75396273978475,1.57299192097447));
#55402=CARTESIAN_POINT('Ctrl Pts',(-7.59488398040363,-2.2741340561492,-0.615632113222856));
#55403=CARTESIAN_POINT('Ctrl Pts',(-7.46814186160383,-0.720940648501152,
-2.24297408351883));
#55404=CARTESIAN_POINT('Ctrl Pts',(-7.34139974280405,1.48954593240367,-1.82536062259485));
#55405=CARTESIAN_POINT('Ctrl Pts',(-7.21465762400426,2.34198950274749,0.256463625198942));
#55406=CARTESIAN_POINT('Ctrl Pts',(-7.08791550520447,1.05920349809169,2.10446580356721));
#55407=CARTESIAN_POINT('Ctrl Pts',(-6.96117338640469,-1.18927539801392,
2.03379262579923));
#55408=CARTESIAN_POINT('Ctrl Pts',(-6.8344312676049,-2.35347275343895,0.108877926915484));
#55409=CARTESIAN_POINT('Ctrl Pts',(-6.70768914880511,-1.37197107682013,
-1.91530252508911));
#55410=CARTESIAN_POINT('Ctrl Pts',(-6.58094703000533,0.860378736396868,
-2.19327080752055));
#55411=CARTESIAN_POINT('Ctrl Pts',(-6.45420491120554,2.30830739273333,-0.471598752640533));
#55412=CARTESIAN_POINT('Ctrl Pts',(-6.32746279240575,1.65171500523044,1.68003748284402));
#55413=CARTESIAN_POINT('Ctrl Pts',(-6.20072067360598,-0.510772566486323,
2.29995647536138));
#55414=CARTESIAN_POINT('Ctrl Pts',(-6.07397855480617,-2.20758055932288,
0.822968089865889));
#55415=CARTESIAN_POINT('Ctrl Pts',(-5.94723643600639,-1.89170178550794,
-1.40433356347513));
#55416=CARTESIAN_POINT('Ctrl Pts',(-5.82049431720661,0.148871987083987,
-2.35128167908273));
#55417=CARTESIAN_POINT('Ctrl Pts',(-5.69375219840681,2.05371677028819,-1.15452840168687));
#55418=CARTESIAN_POINT('Ctrl Pts',(-5.56701007960703,2.08615488253003,1.09482702239254));
#55419=CARTESIAN_POINT('Ctrl Pts',(-5.44026796080724,0.216611974209998,
2.34601100924763));
#55420=CARTESIAN_POINT('Ctrl Pts',(-5.31352584200746,-1.85041956126164,
1.45829895774923));
#55421=CARTESIAN_POINT('Ctrl Pts',(-5.18678372320767,-2.23039376696656,
-0.75896775106054));
#55422=CARTESIAN_POINT('Ctrl Pts',(-5.06004160440788,-0.576882037049555,
-2.28427133200172));
#55423=CARTESIAN_POINT('Ctrl Pts',(-4.93329948560809,1.60258234133143,-1.72696793314944));
#55424=CARTESIAN_POINT('Ctrl Pts',(-4.80655736680831,2.32094657675149,0.404839956945686));
#55425=CARTESIAN_POINT('Ctrl Pts',(-4.67981524800852,0.923266420793207,
2.16754873511761));
#55426=CARTESIAN_POINT('Ctrl Pts',(-4.55307312920873,-1.31617060757069,
1.95406840582431));
#55427=CARTESIAN_POINT('Ctrl Pts',(-4.42633101040895,-2.35563368558887,
-0.0409675749140953));
#55428=CARTESIAN_POINT('Ctrl Pts',(-4.29958889160916,-1.24742757618837,
-1.9986527574939));
#55429=CARTESIAN_POINT('Ctrl Pts',(-4.17284677280937,0.998078354190639,
-2.13413401682469));
#55430=CARTESIAN_POINT('Ctrl Pts',(-4.04610465400959,2.33362016704573,-0.323890905768756));
#55431=CARTESIAN_POINT('Ctrl Pts',(-3.9193625352098,1.54156287203605,1.78164876292292));
#55432=CARTESIAN_POINT('Ctrl Pts',(-3.79262041641001,-0.655962132561314,
2.26283054679536));
#55433=CARTESIAN_POINT('Ctrl Pts',(-3.66587829761022,-2.25543589142298,
0.680953260223828));
#55434=CARTESIAN_POINT('Ctrl Pts',(-3.53913617881044,-1.79859240625076,
-1.52176008587877));
#55435=CARTESIAN_POINT('Ctrl Pts',(-3.41239406001065,0.298056756295131,
-2.33706024159941));
#55436=CARTESIAN_POINT('Ctrl Pts',(-3.28565194121087,2.12296277169725,-1.02162491806891));
#55437=CARTESIAN_POINT('Ctrl Pts',(-3.15890982241107,2.0123294206081,1.22524230469704));
#55438=CARTESIAN_POINT('Ctrl Pts',(-3.03216770361129,0.067022912688436,
2.35503637594289));
#55439=CARTESIAN_POINT('Ctrl Pts',(-2.9054255848115,-1.93938946571943,1.3377058366555));
#55440=CARTESIAN_POINT('Ctrl Pts',(-2.77868346601171,-2.17762921689111,
-0.899232668437894));
#55441=CARTESIAN_POINT('Ctrl Pts',(-2.65194134721193,-0.43048932676473,
-2.31632626019967));
#55442=CARTESIAN_POINT('Ctrl Pts',(-2.52519922841214,1.7091346263358,-1.62158787801847));
#55443=CARTESIAN_POINT('Ctrl Pts',(-2.39845710961236,2.29051298743969,0.551578301896968));
#55444=CARTESIAN_POINT('Ctrl Pts',(-2.27171499081256,0.783593777474662,
2.22186165499399));
#55445=CARTESIAN_POINT('Ctrl Pts',(-2.14497287201278,-1.43774055610062,
1.8664379391246));
#55446=CARTESIAN_POINT('Ctrl Pts',(-2.01823075321299,-2.34826356176781,
-0.190647324848677));
#55447=CARTESIAN_POINT('Ctrl Pts',(-1.89148863441321,-1.11783702498862,
-2.07391634106428));
#55448=CARTESIAN_POINT('Ctrl Pts',(-1.76474651561342,1.13173989076134,-2.06636243085856));
#55449=CARTESIAN_POINT('Ctrl Pts',(-1.63800439681363,2.34949064171247,-0.174872561543903));
#55450=CARTESIAN_POINT('Ctrl Pts',(-1.51126227801384,1.42517419668494,1.87605137184651));
#55451=CARTESIAN_POINT('Ctrl Pts',(-1.38452015921406,-0.798498967630685,
2.21654917046805));
#55452=CARTESIAN_POINT('Ctrl Pts',(-1.25777804041427,-2.29416310193808,
0.536183127745966));
#55453=CARTESIAN_POINT('Ctrl Pts',(-1.13103592161449,-1.69821064989898,
-1.63302924007967));
#55454=CARTESIAN_POINT('Ctrl Pts',(-1.0042938028147,0.446044752534434,-2.31338343704634));
#55455=CARTESIAN_POINT('Ctrl Pts',(-0.87755168401491,2.18360165830961,-0.884586961676926));
#55456=CARTESIAN_POINT('Ctrl Pts',(-0.750809565215123,1.93039537687792,
1.35069842422285));
#55457=CARTESIAN_POINT('Ctrl Pts',(-0.624067446415335,-0.0829010322208286,
2.35453654165394));
#55458=CARTESIAN_POINT('Ctrl Pts',(-0.49732532761555,-2.02039098678301,
1.21169383487321));
#55459=CARTESIAN_POINT('Ctrl Pts',(-0.37058320881576,-2.11628572107077,
-1.03584691568837));
#55460=CARTESIAN_POINT('Ctrl Pts',(-0.243841090015977,-0.281912258858396,
-2.33903283263629));
#55461=CARTESIAN_POINT('Ctrl Pts',(-0.117098971216186,1.80792452150913,
-1.50960103471813));
#55462=CARTESIAN_POINT('Ctrl Pts',(0.00964314758359784,2.25245351867153,
0.695991201152868));
#55463=CARTESIAN_POINT('Ctrl Pts',(0.136385266383387,0.637394787168788,
2.26741911145345));
#55464=CARTESIAN_POINT('Ctrl Pts',(0.220880012249911,-0.817692462573564,
1.93610157876188));
#55465=CARTESIAN_POINT('Ctrl Pts',(0.263127385183173,-1.31529881798823,
1.49967215813949));
#55466=CARTESIAN_POINT('Ctrl Pts',(-3.33066907387547E-16,1.94778769460277,
0.44492227130092));
#55467=CARTESIAN_POINT('Ctrl Pts',(-2.78017970008656E-16,1.94229684361246,
0.495391667149364));
#55468=CARTESIAN_POINT('Ctrl Pts',(-8.36995712052826E-17,1.93476724548118,
0.545536653760479));
#55469=CARTESIAN_POINT('Ctrl Pts',(4.44089209850063E-16,1.92517489938227,
0.595239817297363));
#55470=CARTESIAN_POINT('Ctrl Pts',(1.30360610691075E-15,1.91158592682602,
0.665651676742075));
#55471=CARTESIAN_POINT('Ctrl Pts',(1.86666261596114E-15,1.89385995586343,
0.735177204263595));
#55472=CARTESIAN_POINT('Ctrl Pts',(2.16493489801906E-15,1.87228223168555,
0.803608687878914));
#55473=CARTESIAN_POINT('Ctrl Pts',(2.33682441395151E-15,1.85984733650095,
0.843044650590637));
#55474=CARTESIAN_POINT('Ctrl Pts',(3.09850546232639E-15,1.84613226217488,
0.882117351599893));
#55475=CARTESIAN_POINT('Ctrl Pts',(3.3584246494911E-15,1.83118397114934,
0.92078674243017));
#55476=CARTESIAN_POINT('Ctrl Pts',(3.4512817092519E-15,1.82584364068654,
0.934601520686482));
#55477=CARTESIAN_POINT('Ctrl Pts',(5.14526117317723E-15,1.82034502120261,
0.948366855376327));
#55478=CARTESIAN_POINT('Ctrl Pts',(5.10702591327572E-15,1.81469282599686,
0.962074296960212));
#55479=CARTESIAN_POINT('Ctrl Pts',(4.91398682270459E-15,1.78615647957058,
1.03127932039215));
#55480=CARTESIAN_POINT('Ctrl Pts',(1.57991081056868E-15,1.75376708458297,
1.09887379297229));
#55481=CARTESIAN_POINT('Ctrl Pts',(2.02615701994091E-15,1.71783897253111,
1.16463210299435));
#55482=CARTESIAN_POINT('Ctrl Pts',(2.40198295802782E-15,1.68758052745753,
1.22001336569643));
#55483=CARTESIAN_POINT('Ctrl Pts',(9.6226338214899E-16,1.65481094394572,
1.27409256788157));
#55484=CARTESIAN_POINT('Ctrl Pts',(-1.11022302462516E-16,1.61968946493905,
1.32673151007246));
#55485=CARTESIAN_POINT('Ctrl Pts',(-6.27375591389265E-16,1.60279266713668,
1.35205588671848));
#55486=CARTESIAN_POINT('Ctrl Pts',(1.75865109731242E-15,1.58535115062893,
1.3770468300385));
#55487=CARTESIAN_POINT('Ctrl Pts',(2.08166817117217E-15,1.56738072623534,
1.40168833178254));
#55488=CARTESIAN_POINT('Ctrl Pts',(2.22920138240781E-15,1.55917300400452,
1.41294296869237));
#55489=CARTESIAN_POINT('Ctrl Pts',(2.71625400367046E-15,1.55085356468685,
1.42412649900037));
#55490=CARTESIAN_POINT('Ctrl Pts',(2.74780198594726E-15,1.54242825515624,
1.43523154925794));
#55491=CARTESIAN_POINT('Ctrl Pts',(2.92341485402674E-15,1.49552849598478,
1.49704817222887));
#55492=CARTESIAN_POINT('Ctrl Pts',(-2.81995048998912E-16,1.44546546398451,
1.5562869964589));
#55493=CARTESIAN_POINT('Ctrl Pts',(2.77555756156289E-16,1.39255537912687,
1.61271764417995));
#55494=CARTESIAN_POINT('Ctrl Pts',(8.58082221464105E-16,1.3376618748042,
1.67126368531636));
#55495=CARTESIAN_POINT('Ctrl Pts',(4.15797763651073E-15,1.27970356617436,
1.72678807561908));
#55496=CARTESIAN_POINT('Ctrl Pts',(4.16333634234434E-15,1.21897882333849,
1.77901722439187));
#55497=CARTESIAN_POINT('Ctrl Pts',(4.16735537171954E-15,1.17343526621159,
1.81818908597146));
#55498=CARTESIAN_POINT('Ctrl Pts',(3.33284943214798E-15,1.1263343801715,
1.85550713131994));
#55499=CARTESIAN_POINT('Ctrl Pts',(3.21964677141295E-15,1.07778483301809,
1.89084487676288));
#55500=CARTESIAN_POINT('Ctrl Pts',(3.13474477586169E-15,1.04137267265304,
1.91734818584509));
#55501=CARTESIAN_POINT('Ctrl Pts',(-5.66770666261751E-16,1.00414532731161,
1.94273739803079));
#55502=CARTESIAN_POINT('Ctrl Pts',(-1.2490009027033E-15,0.966144112163664,
1.96695430423757));
#55503=CARTESIAN_POINT('Ctrl Pts',(-1.45112461612772E-15,0.954885527729754,
1.97412902436679));
#55504=CARTESIAN_POINT('Ctrl Pts',(2.39597543965932E-15,0.943558993222492,
1.98120081342834));
#55505=CARTESIAN_POINT('Ctrl Pts',(2.47024622979097E-15,0.93216552638612,
1.9881680745812));
#55506=CARTESIAN_POINT('Ctrl Pts',(2.54570229372929E-15,0.920590233319215,
1.99524652496652));
#55507=CARTESIAN_POINT('Ctrl Pts',(2.81004988937245E-15,0.908953402112989,
2.00221242915967));
#55508=CARTESIAN_POINT('Ctrl Pts',(2.83106871279415E-15,0.897260995259629,
2.00906188950943));
#55509=CARTESIAN_POINT('Ctrl Pts',(2.95672443316249E-15,0.827360897784044,
2.05000965604785));
#55510=CARTESIAN_POINT('Ctrl Pts',(1.01791631789566E-15,0.755427269601269,
2.08682921292429));
#55511=CARTESIAN_POINT('Ctrl Pts',(1.02695629777827E-15,0.681756120222867,
2.11925544414052));
#55512=CARTESIAN_POINT('Ctrl Pts',(1.02998713989497E-15,0.657056328274081,
2.13012701559668));
#55513=CARTESIAN_POINT('Ctrl Pts',(-4.90495785102318E-16,0.632160870785924,
2.14050450196444));
#55514=CARTESIAN_POINT('Ctrl Pts',(-3.05311331771918E-16,0.607079892476986,
2.15037707313459));
#55515=CARTESIAN_POINT('Ctrl Pts',(2.28194171035767E-16,0.534823071221345,
2.17881936918813));
#55516=CARTESIAN_POINT('Ctrl Pts',(-3.84602209731775E-16,0.461028480592185,
2.20307440482459));
#55517=CARTESIAN_POINT('Ctrl Pts',(-7.21644966006352E-16,0.386016998127302,
2.22326012171866));
#55518=CARTESIAN_POINT('Ctrl Pts',(-1.06565834813591E-15,0.309454148753157,
2.24386331407382));
#55519=CARTESIAN_POINT('Ctrl Pts',(2.04973673170663E-17,0.231622791270828,
2.26022731453648));
#55520=CARTESIAN_POINT('Ctrl Pts',(-9.71445146547012E-17,0.152841574836257,
2.27242853705113));
#55521=CARTESIAN_POINT('Ctrl Pts',(-1.25821375813147E-16,0.133637546749305,
2.27540275642055));
#55522=CARTESIAN_POINT('Ctrl Pts',(-1.6506500080672E-16,0.114370082645178,
2.27813013708582));
#55523=CARTESIAN_POINT('Ctrl Pts',(-1.38777878078145E-16,0.0950804498402654,
2.28060703633122));
#55524=CARTESIAN_POINT('Ctrl Pts',(-2.93887515852296E-17,0.0148101173019452,
2.29091420641076));
#55525=CARTESIAN_POINT('Ctrl Pts',(1.50839573175713E-15,-0.0659302194831374,
2.29690448772608));
#55526=CARTESIAN_POINT('Ctrl Pts',(1.72084568816899E-15,-0.146785204436318,
2.2987285654627));
#55527=CARTESIAN_POINT('Ctrl Pts',(1.93752787510066E-15,-0.229250907229958,
2.30058898078018));
#55528=CARTESIAN_POINT('Ctrl Pts',(1.87752606053914E-15,-0.31183670491661,
2.29811569375814));
#55529=CARTESIAN_POINT('Ctrl Pts',(2.78943534937071E-15,-0.394188581132097,
2.29141818620213));
#55530=CARTESIAN_POINT('Ctrl Pts',(3.70842065500646E-15,-0.477179471849459,
2.28466870891997));
#55531=CARTESIAN_POINT('Ctrl Pts',(1.18560937916683E-15,-0.559933765294961,
2.27362925411048));
#55532=CARTESIAN_POINT('Ctrl Pts',(1.08246744900953E-15,-0.642098510266275,
2.25835984156219));
#55533=CARTESIAN_POINT('Ctrl Pts',(1.03867200960394E-15,-0.676986757016934,
2.251876245308));
#55534=CARTESIAN_POINT('Ctrl Pts',(2.77700457960347E-15,-0.711768739488473,
2.2446293603931));
#55535=CARTESIAN_POINT('Ctrl Pts',(2.94902990916057E-15,-0.746417272235456,
2.2366209401127));
#55536=CARTESIAN_POINT('Ctrl Pts',(3.03536878136454E-15,-0.763807241774236,
2.23260154380097));
#55537=CARTESIAN_POINT('Ctrl Pts',(9.62922053153124E-16,-0.781168224136483,
2.22838899571903));
#55538=CARTESIAN_POINT('Ctrl Pts',(9.64506252643105E-16,-0.798467774965364,
2.22399107243053));
#55539=CARTESIAN_POINT('Ctrl Pts',(9.72126262098133E-16,-0.881678722650616,
2.20283703390646));
#55540=CARTESIAN_POINT('Ctrl Pts',(-3.22349389677964E-15,-0.963583670002293,
2.17737390106192));
#55541=CARTESIAN_POINT('Ctrl Pts',(-2.8796409701215E-15,-1.04381049082807,
2.14772461235836));
#55542=CARTESIAN_POINT('Ctrl Pts',(-2.53522490946127E-15,-1.12416870053318,
2.1180267664918));
#55543=CARTESIAN_POINT('Ctrl Pts',(1.71723154797487E-15,-1.20284431254245,
2.08412900274903));
#55544=CARTESIAN_POINT('Ctrl Pts',(2.46330733588707E-15,-1.27946633222789,
2.0461027486611));
#55545=CARTESIAN_POINT('Ctrl Pts',(3.19367717044613E-15,-1.3544753497405,
2.00887700114715));
#55546=CARTESIAN_POINT('Ctrl Pts',(-9.56957227323442E-16,-1.42751726659118,
1.9676945422236));
#55547=CARTESIAN_POINT('Ctrl Pts',(-1.46410661372443E-15,-1.4982323415318,
1.92257464684908));
#55548=CARTESIAN_POINT('Ctrl Pts',(-1.75068212599161E-15,-1.53819139377464,
1.89707869343356));
#55549=CARTESIAN_POINT('Ctrl Pts',(-1.59168655826546E-16,-1.57740718395233,
1.87032464339947));
#55550=CARTESIAN_POINT('Ctrl Pts',(-2.77555756156289E-17,-1.6158113816168,
1.84230937386684));
#55551=CARTESIAN_POINT('Origin',(2.95,-2.77555756156289E-16,-1.73205080756888));
#55552=CARTESIAN_POINT('',(2.6551551490412,-3.18172571617472E-16,-1.73205080756888));
#55553=CARTESIAN_POINT('',(2.6551551490412,-1.5,-0.866025403784439));
#55554=CARTESIAN_POINT('Ctrl Pts',(2.6551551490412,-3.12250225675825E-16,
-1.73205080756888));
#55555=CARTESIAN_POINT('Ctrl Pts',(2.69311148359047,-0.255925908896418,
-1.58429191517493));
#55556=CARTESIAN_POINT('Ctrl Pts',(2.70817242652387,-0.510403274945606,
-1.43736933938377));
#55557=CARTESIAN_POINT('Ctrl Pts',(2.70817242652387,-0.989596725054395,
-1.16070687196955));
#55558=CARTESIAN_POINT('Ctrl Pts',(2.69311148359047,-1.24407409110358,-1.01378429617839));
#55559=CARTESIAN_POINT('Ctrl Pts',(2.6551551490412,-1.5,-0.866025403784439));
#55560=CARTESIAN_POINT('',(0.75,-2.77555756156289E-16,-1.73205080756888));
#55561=CARTESIAN_POINT('',(2.95,-3.18172571617472E-16,-1.73205080756888));
#55562=CARTESIAN_POINT('',(0.75,-1.5,-0.866025403784439));
#55563=CARTESIAN_POINT('',(0.75,-1.5,-0.866025403784439));
#55564=CARTESIAN_POINT('',(2.95,-1.5,-0.866025403784439));
#55565=CARTESIAN_POINT('Origin',(2.95,-1.5,-0.866025403784439));
#55566=CARTESIAN_POINT('',(2.6551551490412,-1.5,0.866025403784439));
#55567=CARTESIAN_POINT('Ctrl Pts',(2.6551551490412,-1.5,-0.866025403784439));
#55568=CARTESIAN_POINT('Ctrl Pts',(2.69311148359047,-1.5,-0.570507618996547));
#55569=CARTESIAN_POINT('Ctrl Pts',(2.70817242652387,-1.5,-0.276662467414215));
#55570=CARTESIAN_POINT('Ctrl Pts',(2.70817242652387,-1.5,0.276662467414215));
#55571=CARTESIAN_POINT('Ctrl Pts',(2.69311148359047,-1.5,0.570507618996546));
#55572=CARTESIAN_POINT('Ctrl Pts',(2.6551551490412,-1.5,0.866025403784439));
#55573=CARTESIAN_POINT('',(0.75,-1.5,0.866025403784439));
#55574=CARTESIAN_POINT('',(0.75,-1.5,0.866025403784439));
#55575=CARTESIAN_POINT('',(2.95,-1.5,0.866025403784439));
#55576=CARTESIAN_POINT('Origin',(2.95,-1.5,0.866025403784439));
#55577=CARTESIAN_POINT('',(2.6551551490412,1.06057523872491E-16,1.73205080756888));
#55578=CARTESIAN_POINT('Ctrl Pts',(2.6551551490412,-1.5,0.866025403784439));
#55579=CARTESIAN_POINT('Ctrl Pts',(2.69311148359047,-1.24407409110358,1.01378429617838));
#55580=CARTESIAN_POINT('Ctrl Pts',(2.70817242652387,-0.989596725054395,
1.16070687196955));
#55581=CARTESIAN_POINT('Ctrl Pts',(2.70817242652387,-0.510403274945606,
1.43736933938377));
#55582=CARTESIAN_POINT('Ctrl Pts',(2.69311148359047,-0.255925908896417,
1.58429191517493));
#55583=CARTESIAN_POINT('Ctrl Pts',(2.6551551490412,3.46944695195361E-17,
1.73205080756888));
#55584=CARTESIAN_POINT('',(0.75,0.,1.73205080756888));
#55585=CARTESIAN_POINT('',(0.75,1.06057523872491E-16,1.73205080756888));
#55586=CARTESIAN_POINT('',(2.95,1.06057523872491E-16,1.73205080756888));
#55587=CARTESIAN_POINT('Origin',(2.95,0.,1.73205080756888));
#55588=CARTESIAN_POINT('',(2.6551551490412,1.5,0.866025403784439));
#55589=CARTESIAN_POINT('Ctrl Pts',(2.6551551490412,1.04083408558608E-16,
1.73205080756888));
#55590=CARTESIAN_POINT('Ctrl Pts',(2.69311148359047,0.255925908896417,1.58429191517493));
#55591=CARTESIAN_POINT('Ctrl Pts',(2.70817242652387,0.510403274945606,1.43736933938377));
#55592=CARTESIAN_POINT('Ctrl Pts',(2.70817242652387,0.989596725054395,1.16070687196955));
#55593=CARTESIAN_POINT('Ctrl Pts',(2.69311148359047,1.24407409110358,1.01378429617838));
#55594=CARTESIAN_POINT('Ctrl Pts',(2.6551551490412,1.5,0.866025403784438));
#55595=CARTESIAN_POINT('',(0.75,1.5,0.866025403784439));
#55596=CARTESIAN_POINT('',(0.75,1.5,0.866025403784439));
#55597=CARTESIAN_POINT('',(2.95,1.5,0.866025403784439));
#55598=CARTESIAN_POINT('Origin',(2.95,1.5,-0.866025403784439));
#55599=CARTESIAN_POINT('',(2.6551551490412,1.5,-0.866025403784439));
#55600=CARTESIAN_POINT('Ctrl Pts',(2.6551551490412,1.5,-0.866025403784439));
#55601=CARTESIAN_POINT('Ctrl Pts',(2.69311148359047,1.24407409110358,-1.01378429617839));
#55602=CARTESIAN_POINT('Ctrl Pts',(2.70817242652387,0.989596725054393,-1.16070687196955));
#55603=CARTESIAN_POINT('Ctrl Pts',(2.70817242652387,0.510403274945605,-1.43736933938377));
#55604=CARTESIAN_POINT('Ctrl Pts',(2.69311148359047,0.255925908896417,-1.58429191517493));
#55605=CARTESIAN_POINT('Ctrl Pts',(2.6551551490412,-2.08166817117217E-16,
-1.73205080756888));
#55606=CARTESIAN_POINT('',(0.75,1.5,-0.866025403784439));
#55607=CARTESIAN_POINT('',(2.95,1.5,-0.866025403784439));
#55608=CARTESIAN_POINT('',(0.75,-3.18172571617472E-16,-1.73205080756888));
#55609=CARTESIAN_POINT('Origin',(2.95,1.5,0.866025403784439));
#55610=CARTESIAN_POINT('Ctrl Pts',(2.6551551490412,1.5,0.866025403784439));
#55611=CARTESIAN_POINT('Ctrl Pts',(2.69311148359047,1.5,0.570507618996546));
#55612=CARTESIAN_POINT('Ctrl Pts',(2.70817242652387,1.5,0.276662467414214));
#55613=CARTESIAN_POINT('Ctrl Pts',(2.70817242652387,1.5,-0.276662467414215));
#55614=CARTESIAN_POINT('Ctrl Pts',(2.69311148359047,1.5,-0.570507618996547));
#55615=CARTESIAN_POINT('Ctrl Pts',(2.6551551490412,1.5,-0.866025403784439));
#55616=CARTESIAN_POINT('',(0.75,1.5,-0.866025403784439));
#55617=CARTESIAN_POINT('Origin',(0.75,0.,0.));
#55618=CARTESIAN_POINT('Origin',(-10.,2.2,0.));
#55619=CARTESIAN_POINT('',(-10.,-2.2,-2.69422295812418E-16));
#55620=CARTESIAN_POINT('Origin',(-10.,0.,0.));
#55621=CARTESIAN_POINT('Origin',(-9.85,0.,0.));
#55622=CARTESIAN_POINT('',(-9.85,-2.35,-2.87791997799628E-16));
#55623=CARTESIAN_POINT('Origin',(-4.85,0.,0.));
#55624=CARTESIAN_POINT('Origin',(0.,0.,0.));
#55625=CARTESIAN_POINT('Origin',(0.,4.75,0.));
#55626=CARTESIAN_POINT('',(0.,-5.81707229594993E-16,4.75));
#55627=CARTESIAN_POINT('Origin',(0.,0.,0.));
#55628=CARTESIAN_POINT('Ctrl Pts',(0.,0.,4.75));
#55629=CARTESIAN_POINT('Ctrl Pts',(0.,-4.75,4.75));
#55630=CARTESIAN_POINT('Ctrl Pts',(0.,-4.75,0.));
#55631=CARTESIAN_POINT('Ctrl Pts',(0.,-4.75,-4.75));
#55632=CARTESIAN_POINT('Ctrl Pts',(0.,0.,-4.75));
#55633=CARTESIAN_POINT('Ctrl Pts',(0.,4.75,-4.75));
#55634=CARTESIAN_POINT('Ctrl Pts',(0.,4.75,0.));
#55635=CARTESIAN_POINT('Ctrl Pts',(0.,4.75,4.75));
#55636=CARTESIAN_POINT('Ctrl Pts',(0.,0.,4.75));
#55637=CARTESIAN_POINT('Ctrl Pts',(2.23533561342085,0.,3.85933086966187));
#55638=CARTESIAN_POINT('Ctrl Pts',(2.23533561342085,-3.85933086966187,3.85933086966187));
#55639=CARTESIAN_POINT('Ctrl Pts',(2.23533561342085,-3.85933086966187,0.));
#55640=CARTESIAN_POINT('Ctrl Pts',(2.23533561342085,-3.85933086966187,-3.85933086966187));
#55641=CARTESIAN_POINT('Ctrl Pts',(2.23533561342085,0.,-3.85933086966187));
#55642=CARTESIAN_POINT('Ctrl Pts',(2.23533561342085,3.85933086966187,-3.85933086966187));
#55643=CARTESIAN_POINT('Ctrl Pts',(2.23533561342085,3.85933086966187,0.));
#55644=CARTESIAN_POINT('Ctrl Pts',(2.23533561342085,3.85933086966187,3.85933086966187));
#55645=CARTESIAN_POINT('Ctrl Pts',(2.23533561342085,0.,3.85933086966187));
#55646=CARTESIAN_POINT('Ctrl Pts',(2.70817242652387,0.,1.5));
#55647=CARTESIAN_POINT('Ctrl Pts',(2.70817242652387,-1.5,1.5));
#55648=CARTESIAN_POINT('Ctrl Pts',(2.70817242652387,-1.5,0.));
#55649=CARTESIAN_POINT('Ctrl Pts',(2.70817242652387,-1.5,-1.5));
#55650=CARTESIAN_POINT('Ctrl Pts',(2.70817242652387,0.,-1.5));
#55651=CARTESIAN_POINT('Ctrl Pts',(2.70817242652387,1.5,-1.5));
#55652=CARTESIAN_POINT('Ctrl Pts',(2.70817242652387,1.5,0.));
#55653=CARTESIAN_POINT('Ctrl Pts',(2.70817242652387,1.5,1.5));
#55654=CARTESIAN_POINT('Ctrl Pts',(2.70817242652387,0.,1.5));
#55655=CARTESIAN_POINT('Ctrl Pts',(2.6551551490412,0.,1.73205080756888));
#55656=CARTESIAN_POINT('Ctrl Pts',(2.09425930345968,0.,3.91554270360305));
#55657=CARTESIAN_POINT('Ctrl Pts',(0.,0.,4.75));
#55658=CARTESIAN_POINT('',(0.,0.,140.));
#55659=CARTESIAN_POINT('',(0.,0.,140.));
#55660=CARTESIAN_POINT('',(0.,0.,140.));
#55661=CARTESIAN_POINT('',(0.,0.,140.));
#55662=CARTESIAN_POINT('',(0.,0.,140.));
#55663=CARTESIAN_POINT('',(0.,66.,140.));
#55664=CARTESIAN_POINT('',(0.,113.,140.));
#55665=CARTESIAN_POINT('',(0.,0.,140.));
#55666=CARTESIAN_POINT('',(0.,0.,140.));
#55667=CARTESIAN_POINT('',(0.,0.,140.));
#55668=CARTESIAN_POINT('',(0.,81.,140.));
#55669=CARTESIAN_POINT('',(0.,81.5,140.));
#55670=CARTESIAN_POINT('',(0.,0.,140.));
#55671=CARTESIAN_POINT('',(0.,128.02,140.));
#55672=CARTESIAN_POINT('',(0.,128.,140.));
#55673=CARTESIAN_POINT('',(92.,24.5,220.));
#55674=CARTESIAN_POINT('',(0.,0.,140.));
#55675=CARTESIAN_POINT('',(0.,0.,140.));
#55676=CARTESIAN_POINT('',(75.7581216659255,-14.,171.380041453937));
#55677=CARTESIAN_POINT('',(31.3800414539374,-14.,215.758121665926));
#55678=CARTESIAN_POINT('',(-31.3800414539374,-14.,215.758121665926));
#55679=CARTESIAN_POINT('',(-75.7581216659255,-14.,171.380041453937));
#55680=CARTESIAN_POINT('',(-75.7581216659255,-14.,108.619958546063));
#55681=CARTESIAN_POINT('',(-31.3800414539373,-14.,64.2418783340745));
#55682=CARTESIAN_POINT('',(31.3800414539374,-14.,64.2418783340745));
#55683=CARTESIAN_POINT('',(75.7581216659255,-14.,108.619958546063));
#55684=CARTESIAN_POINT('',(41.0121933088198,62.,181.01219330882));
#55685=CARTESIAN_POINT('',(-41.0121933088198,62.,181.01219330882));
#55686=CARTESIAN_POINT('',(-41.0121933088198,62.,98.9878066911803));
#55687=CARTESIAN_POINT('',(41.0121933088197,62.,98.9878066911802));
#55688=CARTESIAN_POINT('',(-45.,24.5,254.));
#55689=CARTESIAN_POINT('',(45.,24.5,254.));
#55690=CARTESIAN_POINT('',(-56.5,141.,102.));
#55691=CARTESIAN_POINT('',(-56.5,141.,178.));
#55692=CARTESIAN_POINT('',(-56.5,193.,102.));
#55693=CARTESIAN_POINT('',(-56.5,193.,178.));
#55694=UNCERTAINTY_MEASURE_WITH_UNIT(LENGTH_MEASURE(0.01),#55738,
'DISTANCE_ACCURACY_VALUE',
'Maximum model space distance between geometric entities at asserted c
onnectivities');
#55695=UNCERTAINTY_MEASURE_WITH_UNIT(LENGTH_MEASURE(0.01),#55738,
'DISTANCE_ACCURACY_VALUE',
'Maximum model space distance between geometric entities at asserted c
onnectivities');
#55696=UNCERTAINTY_MEASURE_WITH_UNIT(LENGTH_MEASURE(0.01),#55738,
'DISTANCE_ACCURACY_VALUE',
'Maximum model space distance between geometric entities at asserted c
onnectivities');
#55697=UNCERTAINTY_MEASURE_WITH_UNIT(LENGTH_MEASURE(0.01),#55738,
'DISTANCE_ACCURACY_VALUE',
'Maximum model space distance between geometric entities at asserted c
onnectivities');
#55698=UNCERTAINTY_MEASURE_WITH_UNIT(LENGTH_MEASURE(0.01),#55738,
'DISTANCE_ACCURACY_VALUE',
'Maximum model space distance between geometric entities at asserted c
onnectivities');
#55699=UNCERTAINTY_MEASURE_WITH_UNIT(LENGTH_MEASURE(0.01),#55738,
'DISTANCE_ACCURACY_VALUE',
'Maximum model space distance between geometric entities at asserted c
onnectivities');
#55700=UNCERTAINTY_MEASURE_WITH_UNIT(LENGTH_MEASURE(0.01),#55738,
'DISTANCE_ACCURACY_VALUE',
'Maximum model space distance between geometric entities at asserted c
onnectivities');
#55701=UNCERTAINTY_MEASURE_WITH_UNIT(LENGTH_MEASURE(0.01),#55738,
'DISTANCE_ACCURACY_VALUE',
'Maximum model space distance between geometric entities at asserted c
onnectivities');
#55702=UNCERTAINTY_MEASURE_WITH_UNIT(LENGTH_MEASURE(0.01),#55738,
'DISTANCE_ACCURACY_VALUE',
'Maximum model space distance between geometric entities at asserted c
onnectivities');
#55703=UNCERTAINTY_MEASURE_WITH_UNIT(LENGTH_MEASURE(0.01),#55738,
'DISTANCE_ACCURACY_VALUE',
'Maximum model space distance between geometric entities at asserted c
onnectivities');
#55704=UNCERTAINTY_MEASURE_WITH_UNIT(LENGTH_MEASURE(0.01),#55738,
'DISTANCE_ACCURACY_VALUE',
'Maximum model space distance between geometric entities at asserted c
onnectivities');
#55705=UNCERTAINTY_MEASURE_WITH_UNIT(LENGTH_MEASURE(0.01),#55738,
'DISTANCE_ACCURACY_VALUE',
'Maximum model space distance between geometric entities at asserted c
onnectivities');
#55706=UNCERTAINTY_MEASURE_WITH_UNIT(LENGTH_MEASURE(0.01),#55738,
'DISTANCE_ACCURACY_VALUE',
'Maximum model space distance between geometric entities at asserted c
onnectivities');
#55707=UNCERTAINTY_MEASURE_WITH_UNIT(LENGTH_MEASURE(0.01),#55738,
'DISTANCE_ACCURACY_VALUE',
'Maximum model space distance between geometric entities at asserted c
onnectivities');
#55708=UNCERTAINTY_MEASURE_WITH_UNIT(LENGTH_MEASURE(0.01),#55738,
'DISTANCE_ACCURACY_VALUE',
'Maximum model space distance between geometric entities at asserted c
onnectivities');
#55709=UNCERTAINTY_MEASURE_WITH_UNIT(LENGTH_MEASURE(0.01),#55738,
'DISTANCE_ACCURACY_VALUE',
'Maximum model space distance between geometric entities at asserted c
onnectivities');
#55710=UNCERTAINTY_MEASURE_WITH_UNIT(LENGTH_MEASURE(0.01),#55738,
'DISTANCE_ACCURACY_VALUE',
'Maximum model space distance between geometric entities at asserted c
onnectivities');
#55711=UNCERTAINTY_MEASURE_WITH_UNIT(LENGTH_MEASURE(0.01),#55738,
'DISTANCE_ACCURACY_VALUE',
'Maximum model space distance between geometric entities at asserted c
onnectivities');
#55712=UNCERTAINTY_MEASURE_WITH_UNIT(LENGTH_MEASURE(0.01),#55738,
'DISTANCE_ACCURACY_VALUE',
'Maximum model space distance between geometric entities at asserted c
onnectivities');
#55713=UNCERTAINTY_MEASURE_WITH_UNIT(LENGTH_MEASURE(0.01),#55738,
'DISTANCE_ACCURACY_VALUE',
'Maximum model space distance between geometric entities at asserted c
onnectivities');
#55714=UNCERTAINTY_MEASURE_WITH_UNIT(LENGTH_MEASURE(0.01),#55738,
'DISTANCE_ACCURACY_VALUE',
'Maximum model space distance between geometric entities at asserted c
onnectivities');
#55715=UNCERTAINTY_MEASURE_WITH_UNIT(LENGTH_MEASURE(0.01),#55738,
'DISTANCE_ACCURACY_VALUE',
'Maximum model space distance between geometric entities at asserted c
onnectivities');
#55716=(
GEOMETRIC_REPRESENTATION_CONTEXT(3)
GLOBAL_UNCERTAINTY_ASSIGNED_CONTEXT((#55694))
GLOBAL_UNIT_ASSIGNED_CONTEXT((#55738,#55740,#55741))
REPRESENTATION_CONTEXT('','3D')
);
#55717=(
GEOMETRIC_REPRESENTATION_CONTEXT(3)
GLOBAL_UNCERTAINTY_ASSIGNED_CONTEXT((#55695))
GLOBAL_UNIT_ASSIGNED_CONTEXT((#55738,#55740,#55741))
REPRESENTATION_CONTEXT('','3D')
);
#55718=(
GEOMETRIC_REPRESENTATION_CONTEXT(3)
GLOBAL_UNCERTAINTY_ASSIGNED_CONTEXT((#55696))
GLOBAL_UNIT_ASSIGNED_CONTEXT((#55738,#55740,#55741))
REPRESENTATION_CONTEXT('','3D')
);
#55719=(
GEOMETRIC_REPRESENTATION_CONTEXT(3)
GLOBAL_UNCERTAINTY_ASSIGNED_CONTEXT((#55697))
GLOBAL_UNIT_ASSIGNED_CONTEXT((#55738,#55740,#55741))
REPRESENTATION_CONTEXT('','3D')
);
#55720=(
GEOMETRIC_REPRESENTATION_CONTEXT(3)
GLOBAL_UNCERTAINTY_ASSIGNED_CONTEXT((#55698))
GLOBAL_UNIT_ASSIGNED_CONTEXT((#55738,#55740,#55741))
REPRESENTATION_CONTEXT('','3D')
);
#55721=(
GEOMETRIC_REPRESENTATION_CONTEXT(3)
GLOBAL_UNCERTAINTY_ASSIGNED_CONTEXT((#55699))
GLOBAL_UNIT_ASSIGNED_CONTEXT((#55738,#55740,#55741))
REPRESENTATION_CONTEXT('','3D')
);
#55722=(
GEOMETRIC_REPRESENTATION_CONTEXT(3)
GLOBAL_UNCERTAINTY_ASSIGNED_CONTEXT((#55700))
GLOBAL_UNIT_ASSIGNED_CONTEXT((#55738,#55740,#55741))
REPRESENTATION_CONTEXT('','3D')
);
#55723=(
GEOMETRIC_REPRESENTATION_CONTEXT(3)
GLOBAL_UNCERTAINTY_ASSIGNED_CONTEXT((#55701))
GLOBAL_UNIT_ASSIGNED_CONTEXT((#55738,#55740,#55741))
REPRESENTATION_CONTEXT('','3D')
);
#55724=(
GEOMETRIC_REPRESENTATION_CONTEXT(3)
GLOBAL_UNCERTAINTY_ASSIGNED_CONTEXT((#55702))
GLOBAL_UNIT_ASSIGNED_CONTEXT((#55738,#55740,#55741))
REPRESENTATION_CONTEXT('','3D')
);
#55725=(
GEOMETRIC_REPRESENTATION_CONTEXT(3)
GLOBAL_UNCERTAINTY_ASSIGNED_CONTEXT((#55703))
GLOBAL_UNIT_ASSIGNED_CONTEXT((#55738,#55740,#55741))
REPRESENTATION_CONTEXT('','3D')
);
#55726=(
GEOMETRIC_REPRESENTATION_CONTEXT(3)
GLOBAL_UNCERTAINTY_ASSIGNED_CONTEXT((#55704))
GLOBAL_UNIT_ASSIGNED_CONTEXT((#55738,#55740,#55741))
REPRESENTATION_CONTEXT('','3D')
);
#55727=(
GEOMETRIC_REPRESENTATION_CONTEXT(3)
GLOBAL_UNCERTAINTY_ASSIGNED_CONTEXT((#55705))
GLOBAL_UNIT_ASSIGNED_CONTEXT((#55738,#55740,#55741))
REPRESENTATION_CONTEXT('','3D')
);
#55728=(
GEOMETRIC_REPRESENTATION_CONTEXT(3)
GLOBAL_UNCERTAINTY_ASSIGNED_CONTEXT((#55706))
GLOBAL_UNIT_ASSIGNED_CONTEXT((#55738,#55740,#55741))
REPRESENTATION_CONTEXT('','3D')
);
#55729=(
GEOMETRIC_REPRESENTATION_CONTEXT(3)
GLOBAL_UNCERTAINTY_ASSIGNED_CONTEXT((#55707))
GLOBAL_UNIT_ASSIGNED_CONTEXT((#55738,#55740,#55741))
REPRESENTATION_CONTEXT('','3D')
);
#55730=(
GEOMETRIC_REPRESENTATION_CONTEXT(3)
GLOBAL_UNCERTAINTY_ASSIGNED_CONTEXT((#55708))
GLOBAL_UNIT_ASSIGNED_CONTEXT((#55738,#55740,#55741))
REPRESENTATION_CONTEXT('','3D')
);
#55731=(
GEOMETRIC_REPRESENTATION_CONTEXT(3)
GLOBAL_UNCERTAINTY_ASSIGNED_CONTEXT((#55709))
GLOBAL_UNIT_ASSIGNED_CONTEXT((#55738,#55740,#55741))
REPRESENTATION_CONTEXT('','3D')
);
#55732=(
GEOMETRIC_REPRESENTATION_CONTEXT(3)
GLOBAL_UNCERTAINTY_ASSIGNED_CONTEXT((#55710))
GLOBAL_UNIT_ASSIGNED_CONTEXT((#55738,#55740,#55741))
REPRESENTATION_CONTEXT('','3D')
);
#55733=(
GEOMETRIC_REPRESENTATION_CONTEXT(3)
GLOBAL_UNCERTAINTY_ASSIGNED_CONTEXT((#55711))
GLOBAL_UNIT_ASSIGNED_CONTEXT((#55738,#55740,#55741))
REPRESENTATION_CONTEXT('','3D')
);
#55734=(
GEOMETRIC_REPRESENTATION_CONTEXT(3)
GLOBAL_UNCERTAINTY_ASSIGNED_CONTEXT((#55712))
GLOBAL_UNIT_ASSIGNED_CONTEXT((#55738,#55740,#55741))
REPRESENTATION_CONTEXT('','3D')
);
#55735=(
GEOMETRIC_REPRESENTATION_CONTEXT(3)
GLOBAL_UNCERTAINTY_ASSIGNED_CONTEXT((#55713))
GLOBAL_UNIT_ASSIGNED_CONTEXT((#55738,#55740,#55741))
REPRESENTATION_CONTEXT('','3D')
);
#55736=(
GEOMETRIC_REPRESENTATION_CONTEXT(3)
GLOBAL_UNCERTAINTY_ASSIGNED_CONTEXT((#55714))
GLOBAL_UNIT_ASSIGNED_CONTEXT((#55738,#55740,#55741))
REPRESENTATION_CONTEXT('','3D')
);
#55737=(
GEOMETRIC_REPRESENTATION_CONTEXT(3)
GLOBAL_UNCERTAINTY_ASSIGNED_CONTEXT((#55715))
GLOBAL_UNIT_ASSIGNED_CONTEXT((#55738,#55740,#55741))
REPRESENTATION_CONTEXT('','3D')
);
#55738=(
LENGTH_UNIT()
NAMED_UNIT(*)
SI_UNIT(.MILLI.,.METRE.)
);
#55739=(
LENGTH_UNIT()
NAMED_UNIT(*)
SI_UNIT($,.METRE.)
);
#55740=(
NAMED_UNIT(*)
PLANE_ANGLE_UNIT()
SI_UNIT($,.RADIAN.)
);
#55741=(
NAMED_UNIT(*)
SI_UNIT($,.STERADIAN.)
SOLID_ANGLE_UNIT()
);
#55742=SHAPE_DEFINITION_REPRESENTATION(#55763,#55820);
#55743=SHAPE_DEFINITION_REPRESENTATION(#55764,#55821);
#55744=SHAPE_DEFINITION_REPRESENTATION(#55765,#55822);
#55745=SHAPE_DEFINITION_REPRESENTATION(#55766,#55823);
#55746=SHAPE_DEFINITION_REPRESENTATION(#55767,#55824);
#55747=SHAPE_DEFINITION_REPRESENTATION(#55768,#55825);
#55748=SHAPE_DEFINITION_REPRESENTATION(#55769,#55826);
#55749=SHAPE_DEFINITION_REPRESENTATION(#55770,#55827);
#55750=SHAPE_DEFINITION_REPRESENTATION(#55771,#55828);
#55751=SHAPE_DEFINITION_REPRESENTATION(#55772,#55829);
#55752=SHAPE_DEFINITION_REPRESENTATION(#55773,#55830);
#55753=SHAPE_DEFINITION_REPRESENTATION(#55774,#55831);
#55754=SHAPE_DEFINITION_REPRESENTATION(#55775,#55832);
#55755=SHAPE_DEFINITION_REPRESENTATION(#55776,#55833);
#55756=SHAPE_DEFINITION_REPRESENTATION(#55777,#55834);
#55757=SHAPE_DEFINITION_REPRESENTATION(#55778,#55835);
#55758=SHAPE_DEFINITION_REPRESENTATION(#55779,#55836);
#55759=SHAPE_DEFINITION_REPRESENTATION(#55780,#55837);
#55760=SHAPE_DEFINITION_REPRESENTATION(#55781,#55838);
#55761=SHAPE_DEFINITION_REPRESENTATION(#55782,#55839);
#55762=SHAPE_DEFINITION_REPRESENTATION(#55783,#55840);
#55763=PRODUCT_DEFINITION_SHAPE('',$,#55842);
#55764=PRODUCT_DEFINITION_SHAPE('',$,#55843);
#55765=PRODUCT_DEFINITION_SHAPE('',$,#55844);
#55766=PRODUCT_DEFINITION_SHAPE('',$,#55845);
#55767=PRODUCT_DEFINITION_SHAPE('',$,#55846);
#55768=PRODUCT_DEFINITION_SHAPE('',$,#55847);
#55769=PRODUCT_DEFINITION_SHAPE('',$,#55848);
#55770=PRODUCT_DEFINITION_SHAPE('',$,#55849);
#55771=PRODUCT_DEFINITION_SHAPE('',$,#55850);
#55772=PRODUCT_DEFINITION_SHAPE('',$,#55851);
#55773=PRODUCT_DEFINITION_SHAPE('',$,#55852);
#55774=PRODUCT_DEFINITION_SHAPE('',$,#55853);
#55775=PRODUCT_DEFINITION_SHAPE('',$,#55854);
#55776=PRODUCT_DEFINITION_SHAPE('',$,#55855);
#55777=PRODUCT_DEFINITION_SHAPE('',$,#55856);
#55778=PRODUCT_DEFINITION_SHAPE('',$,#55857);
#55779=PRODUCT_DEFINITION_SHAPE('',$,#55858);
#55780=PRODUCT_DEFINITION_SHAPE('',$,#55859);
#55781=PRODUCT_DEFINITION_SHAPE('',$,#55860);
#55782=PRODUCT_DEFINITION_SHAPE('',$,#55861);
#55783=PRODUCT_DEFINITION_SHAPE('',$,#55862);
#55784=PRODUCT_DEFINITION_SHAPE($,$,#119);
#55785=PRODUCT_DEFINITION_SHAPE($,$,#120);
#55786=PRODUCT_DEFINITION_SHAPE($,$,#121);
#55787=PRODUCT_DEFINITION_SHAPE($,$,#122);
#55788=PRODUCT_DEFINITION_SHAPE($,$,#123);
#55789=PRODUCT_DEFINITION_SHAPE($,$,#124);
#55790=PRODUCT_DEFINITION_SHAPE($,$,#125);
#55791=PRODUCT_DEFINITION_SHAPE($,$,#126);
#55792=PRODUCT_DEFINITION_SHAPE($,$,#127);
#55793=PRODUCT_DEFINITION_SHAPE($,$,#128);
#55794=PRODUCT_DEFINITION_SHAPE($,$,#129);
#55795=PRODUCT_DEFINITION_SHAPE($,$,#130);
#55796=PRODUCT_DEFINITION_SHAPE($,$,#131);
#55797=PRODUCT_DEFINITION_SHAPE($,$,#132);
#55798=PRODUCT_DEFINITION_SHAPE($,$,#133);
#55799=PRODUCT_DEFINITION_SHAPE($,$,#134);
#55800=PRODUCT_DEFINITION_SHAPE($,$,#135);
#55801=PRODUCT_DEFINITION_SHAPE($,$,#136);
#55802=PRODUCT_DEFINITION_SHAPE($,$,#137);
#55803=PRODUCT_DEFINITION_SHAPE($,$,#138);
#55804=PRODUCT_DEFINITION_SHAPE($,$,#139);
#55805=PRODUCT_DEFINITION_SHAPE($,$,#140);
#55806=PRODUCT_DEFINITION_SHAPE($,$,#141);
#55807=PRODUCT_DEFINITION_SHAPE($,$,#142);
#55808=PRODUCT_DEFINITION_SHAPE($,$,#143);
#55809=PRODUCT_DEFINITION_SHAPE($,$,#144);
#55810=PRODUCT_DEFINITION_SHAPE($,$,#145);
#55811=PRODUCT_DEFINITION_SHAPE($,$,#146);
#55812=PRODUCT_DEFINITION_SHAPE($,$,#147);
#55813=PRODUCT_DEFINITION_SHAPE($,$,#148);
#55814=PRODUCT_DEFINITION_SHAPE($,$,#149);
#55815=PRODUCT_DEFINITION_SHAPE($,$,#150);
#55816=PRODUCT_DEFINITION_SHAPE($,$,#151);
#55817=PRODUCT_DEFINITION_SHAPE($,$,#152);
#55818=PRODUCT_DEFINITION_SHAPE($,$,#153);
#55819=PRODUCT_DEFINITION_SHAPE($,$,#154);
#55820=SHAPE_REPRESENTATION('',(#27462,#29940,#29941,#29942,#29943,#29944,
#29945,#29946,#29947,#29948,#29949,#29950,#29951,#29952,#29953,#29954,#29955,
#29956,#29957,#29958,#29959,#29960,#29961,#29962,#29963,#29964,#29965,#29966,
#29967,#29968,#29969,#29970,#29971,#29972,#29973,#29974,#29975),#55716);
#55821=SHAPE_REPRESENTATION('',(#27463),#55717);
#55822=SHAPE_REPRESENTATION('',(#27785),#55718);
#55823=SHAPE_REPRESENTATION('',(#27989),#55719);
#55824=SHAPE_REPRESENTATION('',(#28371),#55720);
#55825=SHAPE_REPRESENTATION('',(#29069),#55721);
#55826=SHAPE_REPRESENTATION('',(#29111),#55722);
#55827=SHAPE_REPRESENTATION('',(#29144),#55723);
#55828=SHAPE_REPRESENTATION('',(#29166),#55724);
#55829=SHAPE_REPRESENTATION('',(#29177),#55725);
#55830=SHAPE_REPRESENTATION('',(#29187),#55726);
#55831=SHAPE_REPRESENTATION('',(#29196),#55727);
#55832=SHAPE_REPRESENTATION('',(#29200),#55728);
#55833=SHAPE_REPRESENTATION('',(#29223),#55729);
#55834=SHAPE_REPRESENTATION('',(#29252),#55730);
#55835=SHAPE_REPRESENTATION('',(#29306),#55731);
#55836=SHAPE_REPRESENTATION('',(#29390),#55732);
#55837=SHAPE_REPRESENTATION('',(#29496),#55733);
#55838=SHAPE_REPRESENTATION('',(#29560),#55734);
#55839=SHAPE_REPRESENTATION('',(#29846),#55735);
#55840=SHAPE_REPRESENTATION('',(#29892),#55736);
#55841=PRODUCT_DEFINITION_CONTEXT('part definition',#55906,'design');
#55842=PRODUCT_DEFINITION('2026-10-26-00-33-53-140','MAS-344',#55863,#55841);
#55843=PRODUCT_DEFINITION('2026-10-26-00-33-54-182','01_Pump_Casing',#55864,
#55841);
#55844=PRODUCT_DEFINITION('2026-10-26-00-33-58-284','02_Casing_Cover',#55865,
#55841);
#55845=PRODUCT_DEFINITION('2026-10-26-00-34-02-758',
'03_Bearing_Bracket_Motor_Adaptor',#55866,#55841);
#55846=PRODUCT_DEFINITION('2026-10-26-00-34-17-360',
'04_Turbine_Impeller_Brass',#55867,#55841);
#55847=PRODUCT_DEFINITION('2026-10-26-00-34-20-668','05_Pump_Shaft',#55868,
#55841);
#55848=PRODUCT_DEFINITION('2026-10-26-00-34-22-718',
'06_Ball_Bearing_6205-2RS',#55869,#55841);
#55849=PRODUCT_DEFINITION('2026-10-26-00-34-23-727',
'07_Mechanical_Seal_Carbon_Head',#55870,#55841);
#55850=PRODUCT_DEFINITION('2026-10-26-00-34-24-473',
'08_Mechanical_Seal_Seat',#55871,#55841);
#55851=PRODUCT_DEFINITION('2026-10-26-00-34-25-074',
'09_Impeller_Drive_Pin_D5x23',#55872,#55841);
#55852=PRODUCT_DEFINITION('2026-10-26-00-34-25-749',
'10_Axial_Preload_Shim_25x32x0.5',#55873,#55841);
#55853=PRODUCT_DEFINITION('2026-10-26-00-34-26-328',
'11_Cover_O-Ring_147x3',#55874,#55841);
#55854=PRODUCT_DEFINITION('2026-10-26-00-34-26-883',
'12_Circlip_DIN_471_-_25',#55875,#55841);
#55855=PRODUCT_DEFINITION('2026-10-26-00-34-27-500',
'13_Circlip_DIN_472_-_52',#55876,#55841);
#55856=PRODUCT_DEFINITION('2026-10-26-00-34-32-795',
'16_Port_Plug_1in_NPT',#55877,#55841);
#55857=PRODUCT_DEFINITION('2026-10-26-00-34-36-690',
'18_Coupling_Window_Plate',#55878,#55841);
#55858=PRODUCT_DEFINITION('2026-10-26-00-34-41-330','20_Coupling_Hub',#55879,
#55841);
#55859=PRODUCT_DEFINITION('2026-10-26-00-34-28-124',
'14_Cover_Bolt_ISO_4017_M10x30',#55880,#55841);
#55860=PRODUCT_DEFINITION('2026-10-26-00-34-30-011',
'15_Bracket_Screw_ISO_4762_M10x30',#55881,#55841);
#55861=PRODUCT_DEFINITION('2026-10-26-00-34-34-597',
'17_Gauge_Plug_1-4_NPT',#55882,#55841);
#55862=PRODUCT_DEFINITION('2026-10-26-00-34-39-424',
'19_Window_Screw_ISO_7380_M5x10',#55883,#55841);
#55863=PRODUCT_DEFINITION_FORMATION('',$,#55908);
#55864=PRODUCT_DEFINITION_FORMATION('',$,#55909);
#55865=PRODUCT_DEFINITION_FORMATION('',$,#55910);
#55866=PRODUCT_DEFINITION_FORMATION('',$,#55911);
#55867=PRODUCT_DEFINITION_FORMATION('',$,#55912);
#55868=PRODUCT_DEFINITION_FORMATION('',$,#55913);
#55869=PRODUCT_DEFINITION_FORMATION('',$,#55914);
#55870=PRODUCT_DEFINITION_FORMATION('',$,#55915);
#55871=PRODUCT_DEFINITION_FORMATION('',$,#55916);
#55872=PRODUCT_DEFINITION_FORMATION('',$,#55917);
#55873=PRODUCT_DEFINITION_FORMATION('',$,#55918);
#55874=PRODUCT_DEFINITION_FORMATION('',$,#55919);
#55875=PRODUCT_DEFINITION_FORMATION('',$,#55920);
#55876=PRODUCT_DEFINITION_FORMATION('',$,#55921);
#55877=PRODUCT_DEFINITION_FORMATION('',$,#55922);
#55878=PRODUCT_DEFINITION_FORMATION('',$,#55923);
#55879=PRODUCT_DEFINITION_FORMATION('',$,#55924);
#55880=PRODUCT_DEFINITION_FORMATION('',$,#55925);
#55881=PRODUCT_DEFINITION_FORMATION('',$,#55926);
#55882=PRODUCT_DEFINITION_FORMATION('',$,#55927);
#55883=PRODUCT_DEFINITION_FORMATION('',$,#55928);
#55884=PRODUCT_RELATED_PRODUCT_CATEGORY('MAS-344','MAS-344',(#55908));
#55885=PRODUCT_RELATED_PRODUCT_CATEGORY('01_Pump_Casing',
'01_Pump_Casing',(#55909));
#55886=PRODUCT_RELATED_PRODUCT_CATEGORY('02_Casing_Cover',
'02_Casing_Cover',(#55910));
#55887=PRODUCT_RELATED_PRODUCT_CATEGORY(
'03_Bearing_Bracket_Motor_Adaptor','03_Bearing_Bracket_Motor_Adaptor',(#55911));
#55888=PRODUCT_RELATED_PRODUCT_CATEGORY('04_Turbine_Impeller_Brass',
'04_Turbine_Impeller_Brass',(#55912));
#55889=PRODUCT_RELATED_PRODUCT_CATEGORY('05_Pump_Shaft','05_Pump_Shaft',
(#55913));
#55890=PRODUCT_RELATED_PRODUCT_CATEGORY('06_Ball_Bearing_6205-2RS',
'06_Ball_Bearing_6205-2RS',(#55914));
#55891=PRODUCT_RELATED_PRODUCT_CATEGORY(
'07_Mechanical_Seal_Carbon_Head','07_Mechanical_Seal_Carbon_Head',(#55915));
#55892=PRODUCT_RELATED_PRODUCT_CATEGORY('08_Mechanical_Seal_Seat',
'08_Mechanical_Seal_Seat',(#55916));
#55893=PRODUCT_RELATED_PRODUCT_CATEGORY('09_Impeller_Drive_Pin_D5x23',
'09_Impeller_Drive_Pin_D5x23',(#55917));
#55894=PRODUCT_RELATED_PRODUCT_CATEGORY(
'10_Axial_Preload_Shim_25x32x0.5','10_Axial_Preload_Shim_25x32x0.5',(#55918));
#55895=PRODUCT_RELATED_PRODUCT_CATEGORY('11_Cover_O-Ring_147x3',
'11_Cover_O-Ring_147x3',(#55919));
#55896=PRODUCT_RELATED_PRODUCT_CATEGORY('12_Circlip_DIN_471_-_25',
'12_Circlip_DIN_471_-_25',(#55920));
#55897=PRODUCT_RELATED_PRODUCT_CATEGORY('13_Circlip_DIN_472_-_52',
'13_Circlip_DIN_472_-_52',(#55921));
#55898=PRODUCT_RELATED_PRODUCT_CATEGORY('16_Port_Plug_1in_NPT',
'16_Port_Plug_1in_NPT',(#55922));
#55899=PRODUCT_RELATED_PRODUCT_CATEGORY('18_Coupling_Window_Plate',
'18_Coupling_Window_Plate',(#55923));
#55900=PRODUCT_RELATED_PRODUCT_CATEGORY('20_Coupling_Hub',
'20_Coupling_Hub',(#55924));
#55901=PRODUCT_RELATED_PRODUCT_CATEGORY('14_Cover_Bolt_ISO_4017_M10x30',
'14_Cover_Bolt_ISO_4017_M10x30',(#55925));
#55902=PRODUCT_RELATED_PRODUCT_CATEGORY(
'15_Bracket_Screw_ISO_4762_M10x30','15_Bracket_Screw_ISO_4762_M10x30',(#55926));
#55903=PRODUCT_RELATED_PRODUCT_CATEGORY('17_Gauge_Plug_1-4_NPT',
'17_Gauge_Plug_1-4_NPT',(#55927));
#55904=PRODUCT_RELATED_PRODUCT_CATEGORY(
'19_Window_Screw_ISO_7380_M5x10','19_Window_Screw_ISO_7380_M5x10',(#55928));
#55905=APPLICATION_PROTOCOL_DEFINITION('international standard',
'automotive_design',2009,#55906);
#55906=APPLICATION_CONTEXT(
'Core Data for Automotive Mechanical Design Process');
#55907=PRODUCT_CONTEXT('part definition',#55906,'mechanical');
#55908=PRODUCT('2026-10-26-00-33-53-140','MAS-344',$,(#55907));
#55909=PRODUCT('2026-10-26-00-33-54-182','01_Pump_Casing',$,(#55907));
#55910=PRODUCT('2026-10-26-00-33-58-284','02_Casing_Cover',$,(#55907));
#55911=PRODUCT('2026-10-26-00-34-02-758',
'03_Bearing_Bracket_Motor_Adaptor',$,(#55907));
#55912=PRODUCT('2026-10-26-00-34-17-360','04_Turbine_Impeller_Brass',$,
(#55907));
#55913=PRODUCT('2026-10-26-00-34-20-668','05_Pump_Shaft',$,(#55907));
#55914=PRODUCT('2026-10-26-00-34-22-718','06_Ball_Bearing_6205-2RS',$,(#55907));
#55915=PRODUCT('2026-10-26-00-34-23-727',
'07_Mechanical_Seal_Carbon_Head',$,(#55907));
#55916=PRODUCT('2026-10-26-00-34-24-473','08_Mechanical_Seal_Seat',$,(#55907));
#55917=PRODUCT('2026-10-26-00-34-25-074','09_Impeller_Drive_Pin_D5x23',
$,(#55907));
#55918=PRODUCT('2026-10-26-00-34-25-749',
'10_Axial_Preload_Shim_25x32x0.5',$,(#55907));
#55919=PRODUCT('2026-10-26-00-34-26-328','11_Cover_O-Ring_147x3',$,(#55907));
#55920=PRODUCT('2026-10-26-00-34-26-883','12_Circlip_DIN_471_-_25',$,(#55907));
#55921=PRODUCT('2026-10-26-00-34-27-500','13_Circlip_DIN_472_-_52',$,(#55907));
#55922=PRODUCT('2026-10-26-00-34-32-795','16_Port_Plug_1in_NPT',$,(#55907));
#55923=PRODUCT('2026-10-26-00-34-36-690','18_Coupling_Window_Plate',$,(#55907));
#55924=PRODUCT('2026-10-26-00-34-41-330','20_Coupling_Hub',$,(#55907));
#55925=PRODUCT('2026-10-26-00-34-28-124',
'14_Cover_Bolt_ISO_4017_M10x30',$,(#55907));
#55926=PRODUCT('2026-10-26-00-34-30-011',
'15_Bracket_Screw_ISO_4762_M10x30',$,(#55907));
#55927=PRODUCT('2026-10-26-00-34-34-597','17_Gauge_Plug_1-4_NPT',$,(#55907));
#55928=PRODUCT('2026-10-26-00-34-39-424',
'19_Window_Screw_ISO_7380_M5x10',$,(#55907));
#55929=PRESENTATION_STYLE_ASSIGNMENT((#55934));
#55930=PRESENTATION_STYLE_ASSIGNMENT((#55935));
#55931=PRESENTATION_STYLE_ASSIGNMENT((#55936));
#55932=PRESENTATION_STYLE_ASSIGNMENT((#55937));
#55933=PRESENTATION_STYLE_ASSIGNMENT((#55938));
#55934=SURFACE_STYLE_USAGE(.BOTH.,#55939);
#55935=SURFACE_STYLE_USAGE(.BOTH.,#55940);
#55936=SURFACE_STYLE_USAGE(.BOTH.,#55941);
#55937=SURFACE_STYLE_USAGE(.BOTH.,#55942);
#55938=SURFACE_STYLE_USAGE(.BOTH.,#55943);
#55939=SURFACE_SIDE_STYLE('',(#55944));
#55940=SURFACE_SIDE_STYLE('',(#55945));
#55941=SURFACE_SIDE_STYLE('',(#55946));
#55942=SURFACE_SIDE_STYLE('',(#55947));
#55943=SURFACE_SIDE_STYLE('',(#55948));
#55944=SURFACE_STYLE_FILL_AREA(#55949);
#55945=SURFACE_STYLE_FILL_AREA(#55950);
#55946=SURFACE_STYLE_FILL_AREA(#55951);
#55947=SURFACE_STYLE_FILL_AREA(#55952);
#55948=SURFACE_STYLE_FILL_AREA(#55953);
#55949=FILL_AREA_STYLE('Steel - Satin',(#55954));
#55950=FILL_AREA_STYLE('MAS496_al',(#55955));
#55951=FILL_AREA_STYLE('MAS496_ti',(#55956));
#55952=FILL_AREA_STYLE('MAS496_ss',(#55957));
#55953=FILL_AREA_STYLE('MAS496_gun',(#55958));
#55954=FILL_AREA_STYLE_COLOUR('Steel - Satin',#55959);
#55955=FILL_AREA_STYLE_COLOUR('MAS496_al',#55960);
#55956=FILL_AREA_STYLE_COLOUR('MAS496_ti',#55961);
#55957=FILL_AREA_STYLE_COLOUR('MAS496_ss',#55962);
#55958=FILL_AREA_STYLE_COLOUR('MAS496_gun',#55963);
#55959=COLOUR_RGB('Steel - Satin',0.627450980392157,0.627450980392157,0.627450980392157);
#55960=COLOUR_RGB('MAS496_al',0.67843137254902,0.705882352941177,0.729411764705882);
#55961=COLOUR_RGB('MAS496_ti',0.549019607843137,0.572549019607843,0.596078431372549);
#55962=COLOUR_RGB('MAS496_ss',0.83921568627451,0.850980392156863,0.862745098039216);
#55963=COLOUR_RGB('MAS496_gun',0.313725490196078,0.337254901960784,0.364705882352941);
#55964=COLOUR_RGB('Dark Blue',0.08,0.2,0.34);
#55965=FILL_AREA_STYLE_COLOUR('',#55964);
#55966=FILL_AREA_STYLE('',(#55965));
#55967=SURFACE_STYLE_FILL_AREA(#55966);
#55968=SURFACE_SIDE_STYLE('',(#55967));
#55969=SURFACE_STYLE_USAGE(.BOTH.,#55968);
#55970=PRESENTATION_STYLE_ASSIGNMENT((#55969));
#55971=COLOUR_RGB('Light Blue',0.38,0.62,0.78);
#55972=FILL_AREA_STYLE_COLOUR('',#55971);
#55973=FILL_AREA_STYLE('',(#55972));
#55974=SURFACE_STYLE_FILL_AREA(#55973);
#55975=SURFACE_SIDE_STYLE('',(#55974));
#55976=SURFACE_STYLE_USAGE(.BOTH.,#55975);
#55977=PRESENTATION_STYLE_ASSIGNMENT((#55976));
#55978=COLOUR_RGB('Sky Blue',0.24,0.69,0.87);
#55979=FILL_AREA_STYLE_COLOUR('',#55978);
#55980=FILL_AREA_STYLE('',(#55979));
#55981=SURFACE_STYLE_FILL_AREA(#55980);
#55982=SURFACE_SIDE_STYLE('',(#55981));
#55983=SURFACE_STYLE_USAGE(.BOTH.,#55982);
#55984=PRESENTATION_STYLE_ASSIGNMENT((#55983));
#55985=COLOUR_RGB('Grey',0.48,0.52,0.57);
#55986=FILL_AREA_STYLE_COLOUR('',#55985);
#55987=FILL_AREA_STYLE('',(#55986));
#55988=SURFACE_STYLE_FILL_AREA(#55987);
#55989=SURFACE_SIDE_STYLE('',(#55988));
#55990=SURFACE_STYLE_USAGE(.BOTH.,#55989);
#55991=PRESENTATION_STYLE_ASSIGNMENT((#55990));
#55992=COLOUR_RGB('Black',0.12,0.14,0.17);
#55993=FILL_AREA_STYLE_COLOUR('',#55992);
#55994=FILL_AREA_STYLE('',(#55993));
#55995=SURFACE_STYLE_FILL_AREA(#55994);
#55996=SURFACE_SIDE_STYLE('',(#55995));
#55997=SURFACE_STYLE_USAGE(.BOTH.,#55996);
#55998=PRESENTATION_STYLE_ASSIGNMENT((#55997));
#55999=COLOUR_RGB('Off White',0.89,0.88,0.83);
#56000=FILL_AREA_STYLE_COLOUR('',#55999);
#56001=FILL_AREA_STYLE('',(#56000));
#56002=SURFACE_STYLE_FILL_AREA(#56001);
#56003=SURFACE_SIDE_STYLE('',(#56002));
#56004=SURFACE_STYLE_USAGE(.BOTH.,#56003);
#56005=PRESENTATION_STYLE_ASSIGNMENT((#56004));
ENDSEC;
END-ISO-10303-21;
